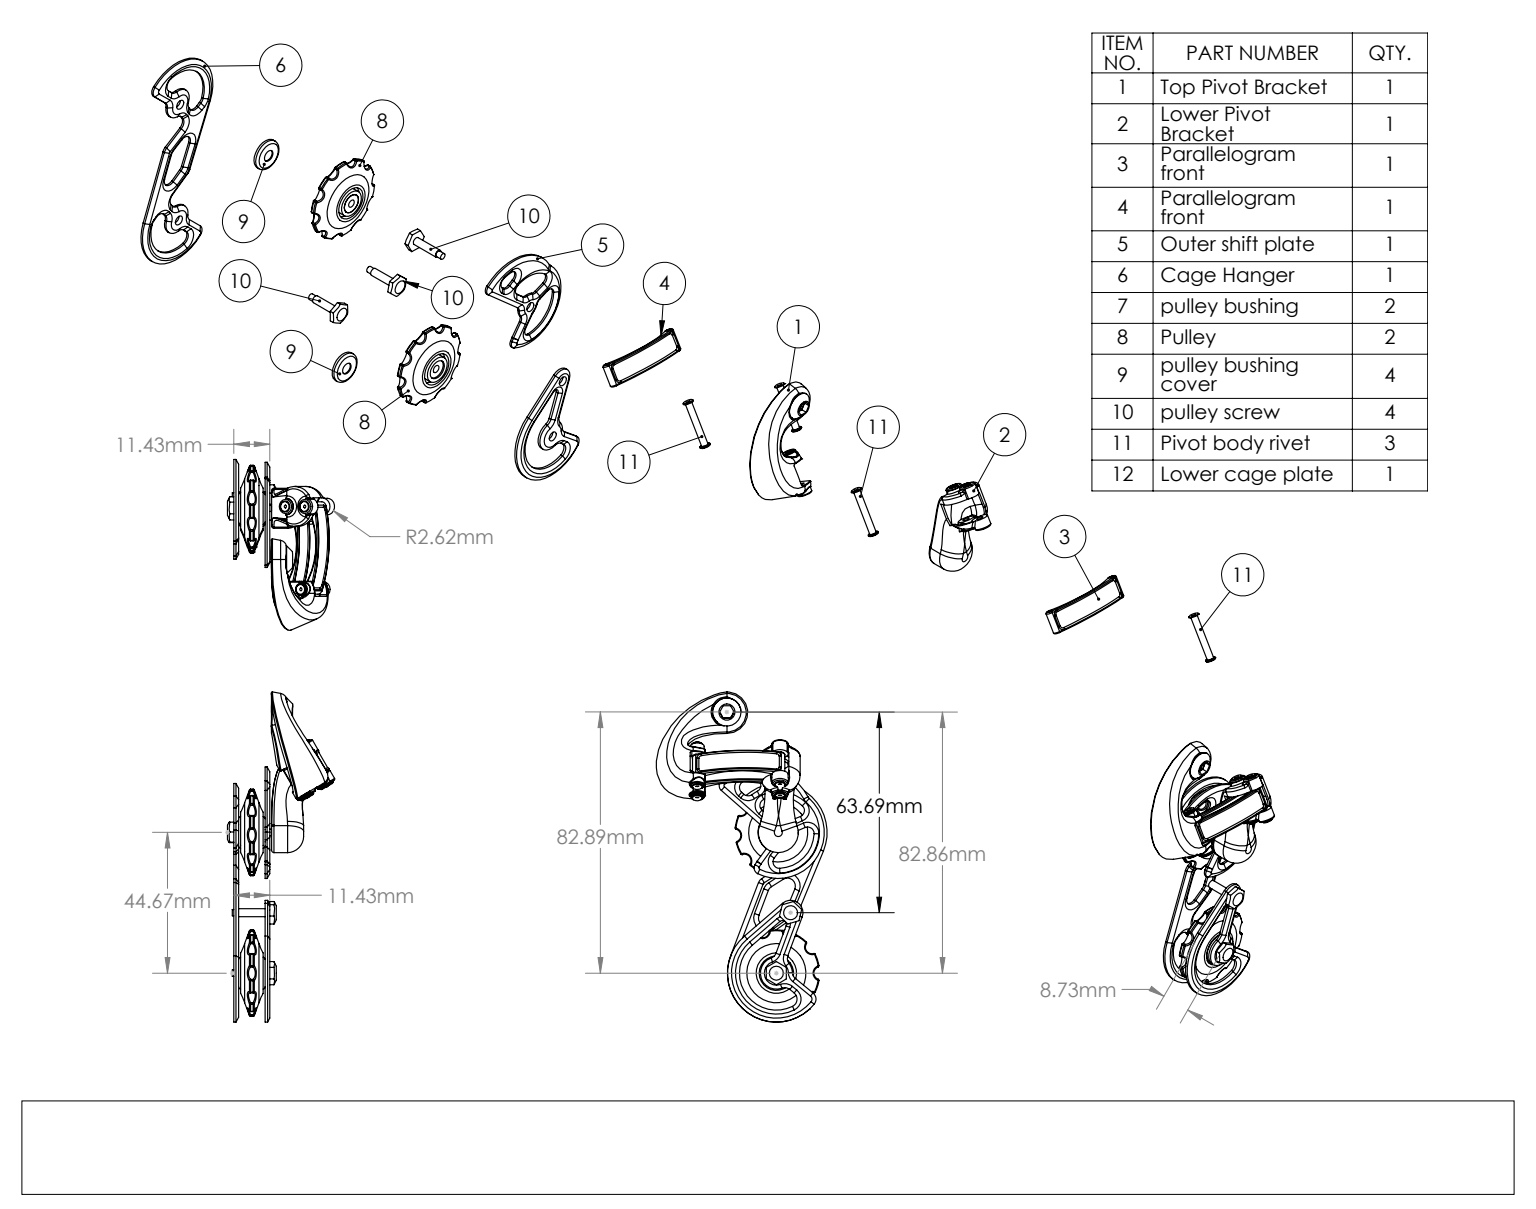
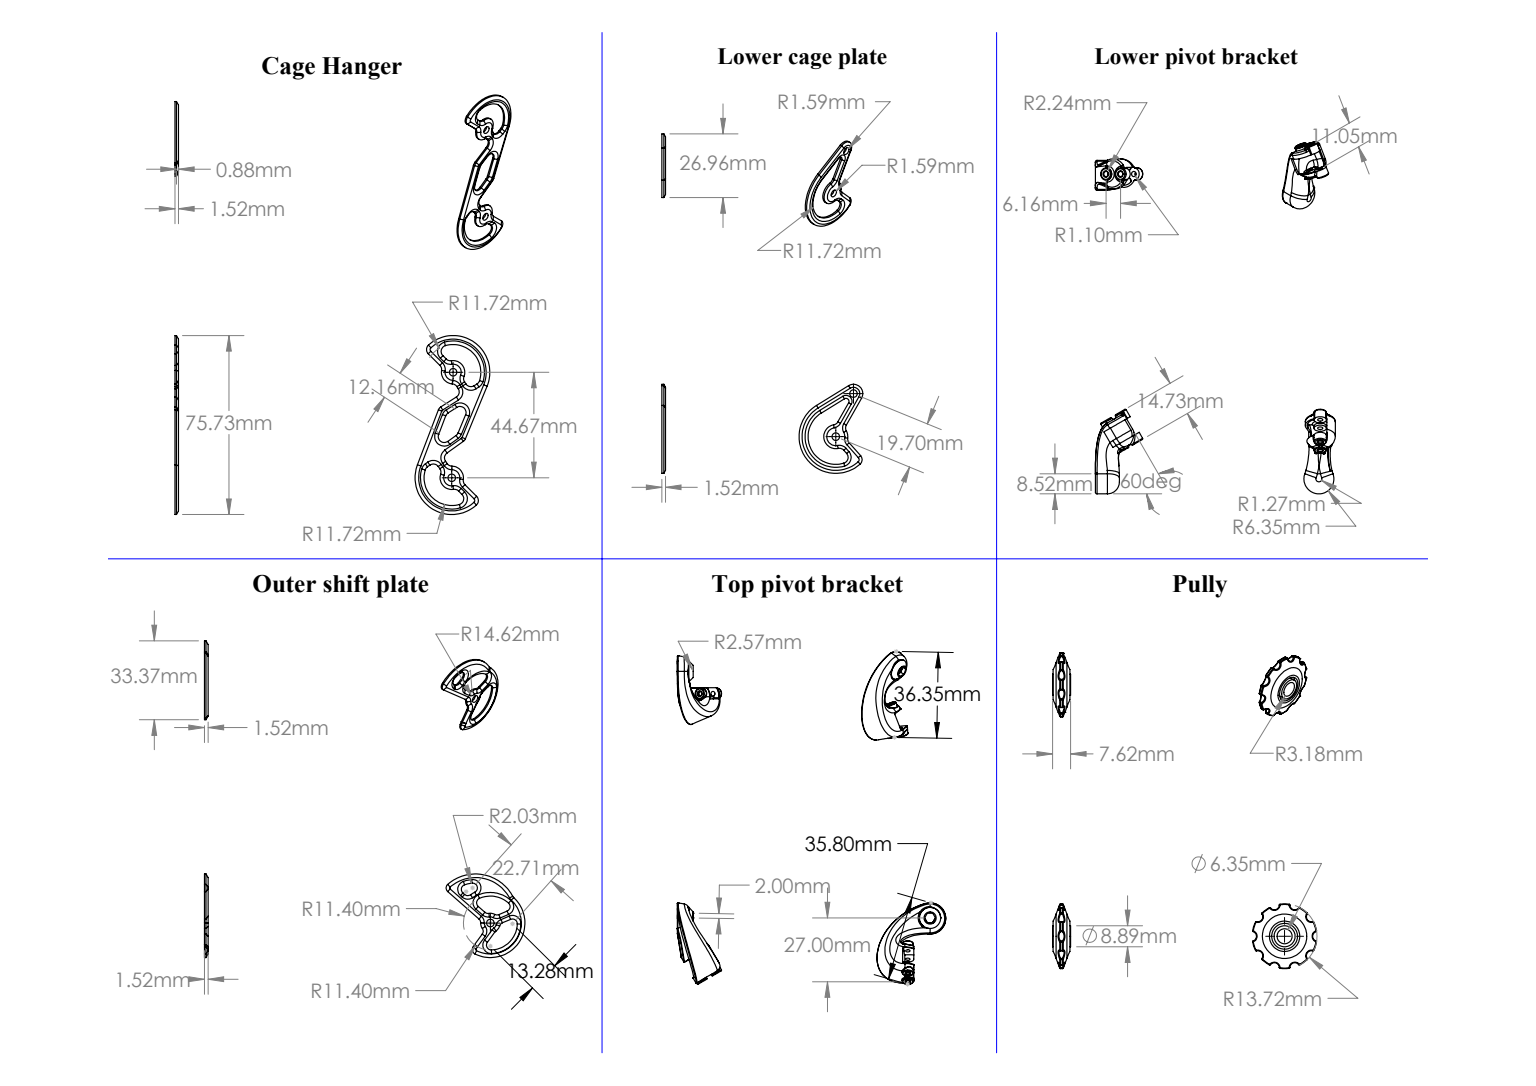
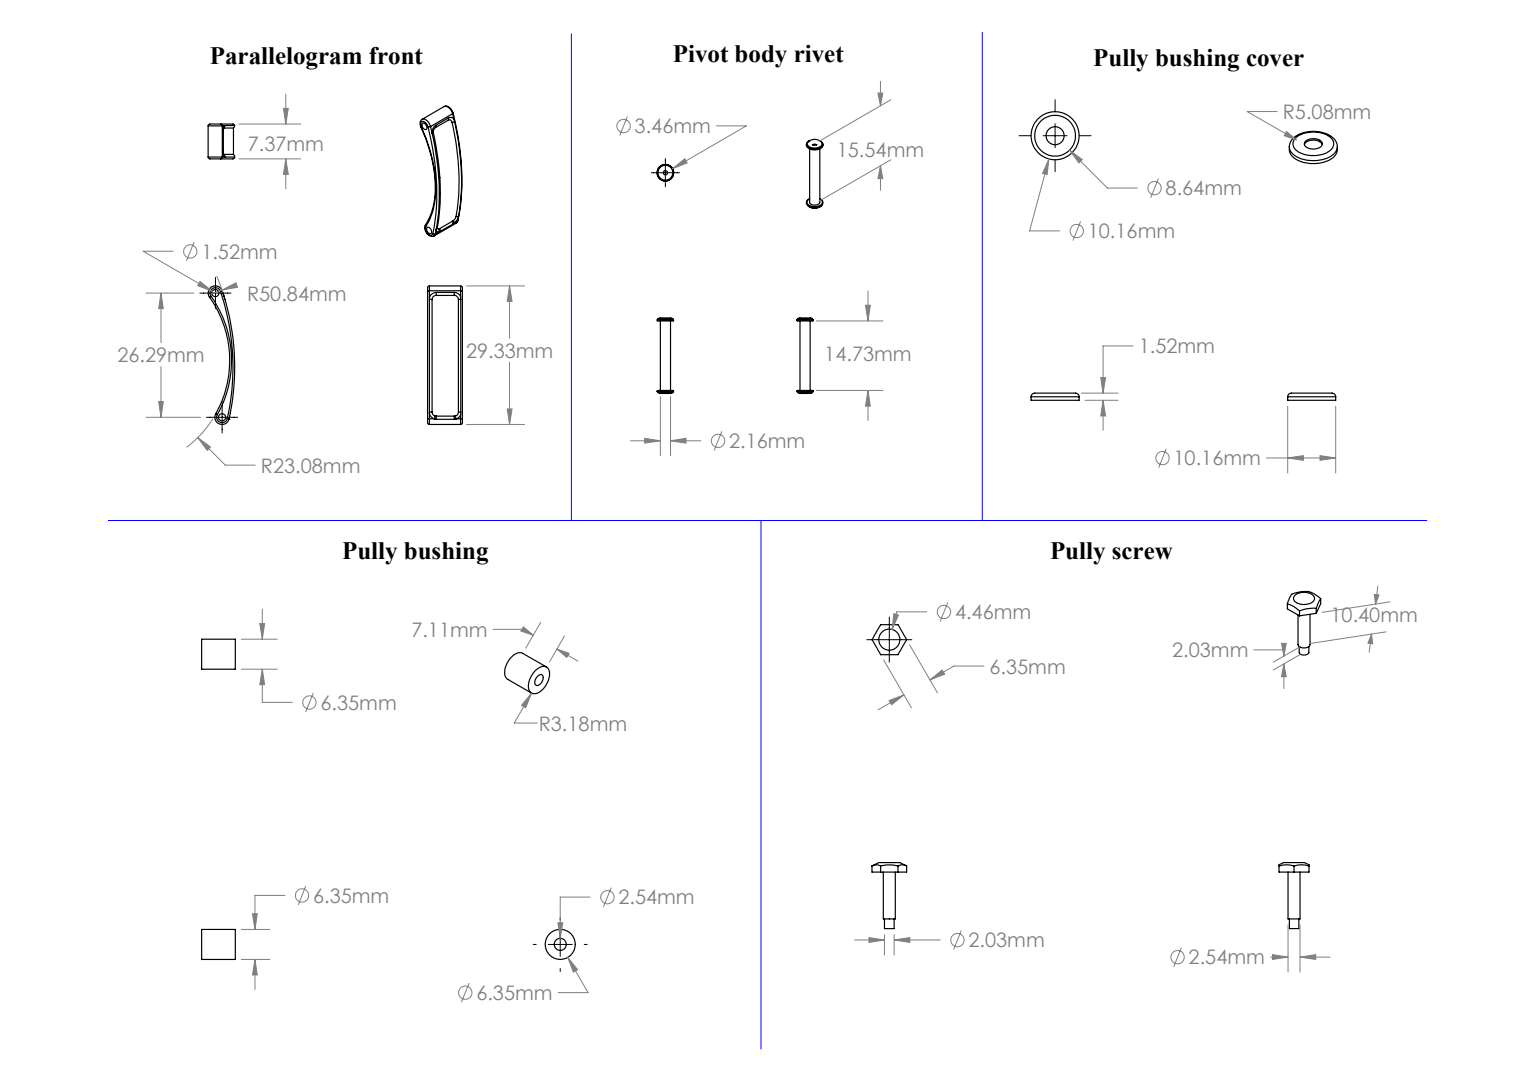
ISO-10303-21;
HEADER;
FILE_DESCRIPTION (('STEP AP214'),
    '1' );
FILE_NAME ('MAT-032',
    '2026-10-12T23:53:07',
    ( '' ),
    ( '' ),
    'SwSTEP 2.0',
    'SolidWorks 2024',
    '' );
FILE_SCHEMA (( 'AUTOMOTIVE_DESIGN' ));
ENDSEC;

DATA;
#1 = CARTESIAN_POINT ( 'NONE',  ( 0.4999436808859595294, -1.292550018364103881, 0.6106580130240608639 ) ) ;
#3 = EDGE_LOOP ( 'NONE', ( #27545, #19145, #8078, #4181 ) ) ;
#2 = CARTESIAN_POINT ( 'NONE',  ( 0.6766858697071348461, -1.447219178500369852, 0.5182417262812423209 ) ) ;
#4 = CARTESIAN_POINT ( 'NONE',  ( 0.4897881687547872565, -1.080982661159355818, 0.5914788577480112330 ) ) ;
#5 = EDGE_LOOP ( 'NONE', ( #28695, #28375, #39300, #8290 ) ) ;
#6 = PERSON_AND_ORGANIZATION ( #28500, #32463 ) ;
#7 = CARTESIAN_POINT ( 'NONE',  ( 0.01548846960707511190, -0.5198120922912051745, -0.07362328916749329155 ) ) ;
#8 = EDGE_LOOP ( 'NONE', ( #25751, #37385, #3783, #18392 ) ) ;
#9 = ORIENTED_EDGE ( 'NONE', *, *, #10978, .F. ) ;
#10 = CARTESIAN_POINT ( 'NONE',  ( 0.3847673884423530866, -1.587979917868051594, 0.7195363636215315051 ) ) ;
#12 = CARTESIAN_POINT ( 'NONE',  ( 0.1868532161955482884, -0.6181774020623623800, -0.006882278619014759076 ) ) ;
#11 = CARTESIAN_POINT ( 'NONE',  ( 0.06449619071327084008, -0.8352737646558907603, 0.1359541117914142838 ) ) ;
#13 = CARTESIAN_POINT ( 'NONE',  ( 0.06860968454252140691, -0.5593946951873564055, 0.07183308462254860138 ) ) ;
#14 = VERTEX_POINT ( 'NONE', #12483 ) ;
#15 = ORIENTED_EDGE ( 'NONE', *, *, #31298, .F. ) ;
#16 = CARTESIAN_POINT ( 'NONE',  ( 0.4409725506264777772, -1.045015864252073712, 0.6370139139982947674 ) ) ;
#17 = CARTESIAN_POINT ( 'NONE',  ( 0.1277648457822606887, -0.6229659815690001823, 0.3707106540332985034 ) ) ;
#18 = ORIENTED_EDGE ( 'NONE', *, *, #35646, .F. ) ;
#19 = CARTESIAN_POINT ( 'NONE',  ( 0.2420619479266831187, -1.321943518198432033, -0.3144976166544464768 ) ) ;
#20 = CARTESIAN_POINT ( 'NONE',  ( 0.6117213743483401744, -1.432107776390856513, -0.6250000000000000000 ) ) ;
#21 = CYLINDRICAL_SURFACE ( 'NONE', #16555, 0.1000000000000000056 ) ;
#22 = ADVANCED_FACE ( 'NONE', ( #25039 ), #12689, .F. ) ;
#23 = CARTESIAN_POINT ( 'NONE',  ( 0.5982604594170003454, -1.483634568127149889, -0.3944719512476840273 ) ) ;
#24 = ADVANCED_FACE ( 'NONE', ( #40477 ), #35210, .T. ) ;
#25 = CARTESIAN_POINT ( 'NONE',  ( 0.3439459955960700865, -1.757593179262507466, 0.4441638180110000222 ) ) ;
#26 = DIRECTION ( 'NONE',  ( 0.000000000000000000, 0.000000000000000000, 1.000000000000000000 ) ) ;
#27 = CARTESIAN_POINT ( 'NONE',  ( 0.1178002186443738025, -1.269485432265525793, 0.6202127893679206805 ) ) ;
#28 = CARTESIAN_POINT ( 'NONE',  ( 0.2462190030042624156, -1.768833963249898611, -0.6590625227467041825 ) ) ;
#29 = CARTESIAN_POINT ( 'NONE',  ( -0.01548846960707524721, 0.000000000000000000, 0.000000000000000000 ) ) ;
#30 = APPROVAL_STATUS ( 'not_yet_approved' ) ;
#31 = CARTESIAN_POINT ( 'NONE',  ( 0.1947294528115406376, -0.9190940877486376559, 0.2754987677893815934 ) ) ;
#32 = PLANE ( 'NONE',  #30520 ) ;
#33 = CARTESIAN_POINT ( 'NONE',  ( 0.4569214742076340707, -1.218928684383336236, 0.5856983068965044836 ) ) ;
#34 = CARTESIAN_POINT ( 'NONE',  ( 0.3193861777821562220, -1.171684894966655399, 0.5563056129421823925 ) ) ;
#35 = CARTESIAN_POINT ( 'NONE',  ( 0.1851448419613674068, -1.516587896426844662, 0.7176110508928341680 ) ) ;
#36 = LINE ( 'NONE', #30842, #35705 ) ;
#37 = DIRECTION ( 'NONE',  ( -6.162975822039154730E-33, 0.000000000000000000, -1.000000000000000000 ) ) ;
#38 = CARTESIAN_POINT ( 'NONE',  ( 0.5966652623928320187, -1.460067201996130271, 0.6057417262805135927 ) ) ;
#39 = EDGE_CURVE ( 'NONE', #17084, #9403, #40506, .T. ) ;
#40 = ORIENTED_EDGE ( 'NONE', *, *, #699, .T. ) ;
#41 = ORIENTED_EDGE ( 'NONE', *, *, #38593, .T. ) ;
#42 = CARTESIAN_POINT ( 'NONE',  ( -0.1105199412301896417, -0.5049077968913929793, 0.1209919789212513253 ) ) ;
#43 = ORIENTED_EDGE ( 'NONE', *, *, #31016, .F. ) ;
#44 = CARTESIAN_POINT ( 'NONE',  ( 0.2625221014770238726, -1.677489247281143347, 0.5299707248247536029 ) ) ;
#45 = CARTESIAN_POINT ( 'NONE',  ( -0.03650581953630592513, -0.4542932396444835375, -0.2355374485430490328 ) ) ;
#46 = CARTESIAN_POINT ( 'NONE',  ( 0.5765142360455419723, -1.424711725393718265, 0.6097170742772620722 ) ) ;
#48 = ORIENTED_EDGE ( 'NONE', *, *, #29288, .T. ) ;
#47 = CARTESIAN_POINT ( 'NONE',  ( 0.001926542279114920901, -0.5275834520082917090, 0.09413269016402606160 ) ) ;
#49 = EDGE_LOOP ( 'NONE', ( #33530, #28150, #39778, #7630 ) ) ;
#50 = FACE_OUTER_BOUND ( 'NONE', #29896, .T. ) ;
#51 = VERTEX_POINT ( 'NONE', #15776 ) ;
#52 = CARTESIAN_POINT ( 'NONE',  ( 0.2972168835034767476, -1.656689438746897558, 0.5739732049407664238 ) ) ;
#54 = CARTESIAN_POINT ( 'NONE',  ( 0.08190433410803919789, -1.308169647316527184, 0.5665045013630258808 ) ) ;
#53 = CARTESIAN_POINT ( 'NONE',  ( 0.5200734380266420764, -1.679028703643771436, -0.4374651140121203485 ) ) ;
#55 = LINE ( 'NONE', #28391, #16768 ) ;
#56 = CALENDAR_DATE ( 2026, 13, 10 ) ;
#58 = ORIENTED_EDGE ( 'NONE', *, *, #32260, .T. ) ;
#57 = EDGE_LOOP ( 'NONE', ( #4186, #2029, #37849, #1328 ) ) ;
#59 = FACE_OUTER_BOUND ( 'NONE', #105, .T. ) ;
#60 = DIRECTION ( 'NONE',  ( 0.8660512985181130219, 0.4999551463232377868, 0.000000000000000000 ) ) ;
#61 = PERSON ( 'NAUO-PER8', 'UNSPECIFIED', 'UNSPECIFIED', ('UNSPECIFIED'), ('UNSPECIFIED'), ('UNSPECIFIED') ) ;
#62 = DIRECTION ( 'NONE',  ( 0.3468893892380631727, 0.9373665302208734618, -0.03180785525186744650 ) ) ;
#63 = CARTESIAN_POINT ( 'NONE',  ( 0.2884976522880303706, -0.9761975876302364519, 0.7460397395601686688 ) ) ;
#64 = CARTESIAN_POINT ( 'NONE',  ( 0.1828007326059407633, -0.8784064217732538982, 0.5457344770029756154 ) ) ;
#65 = CARTESIAN_POINT ( 'NONE',  ( 0.2745644270868899950, -1.657411742223986018, 0.7254928767627549790 ) ) ;
#66 = ADVANCED_FACE ( 'NONE', ( #33910 ), #4970, .T. ) ;
#67 = CARTESIAN_POINT ( 'NONE',  ( 0.3207235327959215287, -1.760688231293898953, 0.5959548780354907427 ) ) ;
#68 = FACE_OUTER_BOUND ( 'NONE', #7963, .T. ) ;
#69 = FACE_OUTER_BOUND ( 'NONE', #19030, .T. ) ;
#70 = CARTESIAN_POINT ( 'NONE',  ( 0.4763501221259694440, -1.554011115824661893, -0.5166151207188711680 ) ) ;
#71 = DIRECTION ( 'NONE',  ( 2.465190328815661892E-32, 1.000000000000000000, -5.978086547377980964E-31 ) ) ;
#72 = DIRECTION ( 'NONE',  ( -0.9999999999999998890, -5.551115123125780853E-17, -5.551115123125781470E-17 ) ) ;
#73 = AXIS2_PLACEMENT_3D ( 'NONE', #22419, #1050, #19125 ) ;
#74 = PLANE ( 'NONE',  #31747 ) ;
#75 = CARTESIAN_POINT ( 'NONE',  ( 0.07120675875603865723, -0.8149881486554784171, 0.8228864848196146831 ) ) ;
#76 = CARTESIAN_POINT ( 'NONE',  ( 0.09717445250287677638, -1.337075187059802994, 0.7110840001749388906 ) ) ;
#77 = APPLICATION_PROTOCOL_DEFINITION ( 'international standard', 'automotive_design', 2000, #10342 ) ;
#78 = CARTESIAN_POINT ( 'NONE',  ( 0.3560095073596968307, -0.8726986411092064744, 0.7484988241699506162 ) ) ;
#79 = AXIS2_PLACEMENT_3D ( 'NONE', #37935, #9745, #19216 ) ;
#80 = CARTESIAN_POINT ( 'NONE',  ( -0.04157143636675594833, 0.4416880288200871196, 0.1614235308635322275 ) ) ;
#81 = CARTESIAN_POINT ( 'NONE',  ( 0.6872956252228072938, -1.545186843986040115, 0.5945327379366810439 ) ) ;
#82 = CARTESIAN_POINT ( 'NONE',  ( 0.4855256156385516775, -1.649569844525025530, -0.6308821889615696676 ) ) ;
#83 = PLANE ( 'NONE',  #29685 ) ;
#84 = ORIENTED_EDGE ( 'NONE', *, *, #28072, .F. ) ;
#85 = FACE_OUTER_BOUND ( 'NONE', #18714, .T. ) ;
#86 = CARTESIAN_POINT ( 'NONE',  ( 0.1825910822803085698, -1.345967781949698239, 0.9412546887375772275 ) ) ;
#87 = CARTESIAN_POINT ( 'NONE',  ( 0.5953442517954894431, -1.487188481951640773, 0.5814371352277787341 ) ) ;
#89 = ORIENTED_EDGE ( 'NONE', *, *, #20270, .F. ) ;
#88 = DIRECTION ( 'NONE',  ( 1.000000000000000000, 0.000000000000000000, 0.000000000000000000 ) ) ;
#90 = CARTESIAN_POINT ( 'NONE',  ( 0.1967848402874973202, -0.7048484731626001309, 0.3032743993732655574 ) ) ;
#92 = ORIENTED_EDGE ( 'NONE', *, *, #28854, .F. ) ;
#91 = ORIENTED_EDGE ( 'NONE', *, *, #5942, .F. ) ;
#93 = DIRECTION ( 'NONE',  ( 0.000000000000000000, 0.9510565162951657436, 0.3090169943749095927 ) ) ;
#94 = CARTESIAN_POINT ( 'NONE',  ( 0.3337487181682026183, -1.684227851221292038, -0.6212492361075898639 ) ) ;
#95 = LINE ( 'NONE', #12201, #34463 ) ;
#96 = PERSON_AND_ORGANIZATION_ROLE ( 'classification_officer' ) ;
#97 = CIRCLE ( 'NONE', #11204, 0.5399999999999999245 ) ;
#98 = ORIENTED_EDGE ( 'NONE', *, *, #22101, .F. ) ;
#99 = CARTESIAN_POINT ( 'NONE',  ( 0.09103128088014370012, -0.7737444593052549280, 0.2676987870228014210 ) ) ;
#100 = CARTESIAN_POINT ( 'NONE',  ( 0.3114310930860528792, -1.743835956959021161, 0.7216218591552465700 ) ) ;
#101 = AXIS2_PLACEMENT_3D ( 'NONE', #14971, #21565, #27524 ) ;
#102 = CARTESIAN_POINT ( 'NONE',  ( 0.5255678041659990196, -1.526919996939806623, 0.5791403307438186543 ) ) ;
#103 = CARTESIAN_POINT ( 'NONE',  ( -0.08000000000000000167, -2.183180860297908144, -0.4937760292030871079 ) ) ;
#104 = CARTESIAN_POINT ( 'NONE',  ( -0.1710642717957937542, 0.4986889573705819423, 0.1482573527501182542 ) ) ;
#105 = EDGE_LOOP ( 'NONE', ( #14125, #9497, #24205 ) ) ;
#106 = VECTOR ( 'NONE', #18794, 39.37007874015748143 ) ;
#107 = CARTESIAN_POINT ( 'NONE',  ( -0.01736481776669303659, -0.6872203660140440151, -0.01676916986599873496 ) ) ;
#108 = CARTESIAN_POINT ( 'NONE',  ( 0.6985683150901143001, -1.438855895731389056, 0.5688516854839209547 ) ) ;
#109 = CARTESIAN_POINT ( 'NONE',  ( 0.5745725605903601041, -1.619018034204693146, 0.5636810530413540743 ) ) ;
#110 = CARTESIAN_POINT ( 'NONE',  ( -0.002236529766539807878, -0.8463514994925549484, 0.1275420592413386567 ) ) ;
#111 = CYLINDRICAL_SURFACE ( 'NONE', #1726, 0.7043128707267513056 ) ;
#112 = CARTESIAN_POINT ( 'NONE',  ( 0.4203826191881492313, -1.700944664958275343, -0.4172566670736511107 ) ) ;
#113 = CARTESIAN_POINT ( 'NONE',  ( 0.01632176102313256591, -1.052923364454138255, 0.5995154855756178458 ) ) ;
#114 = CARTESIAN_POINT ( 'NONE',  ( 0.5138184642618360831, -1.118801421376873551, 0.5693865086028936373 ) ) ;
#115 = DATE_AND_TIME ( #15705, #6911 ) ;
#116 = CARTESIAN_POINT ( 'NONE',  ( 0.3610818047233222972, -1.951413994126270257, -0.4993772958782550786 ) ) ;
#117 = AXIS2_PLACEMENT_3D ( 'NONE', #32026, #16389, #31621 ) ;
#118 = CARTESIAN_POINT ( 'NONE',  ( 0.6078054091579164764, -1.478899637288701996, 0.5472081702953829341 ) ) ;
#119 = VECTOR ( 'NONE', #8950, 39.37007874015748143 ) ;
#120 = CARTESIAN_POINT ( 'NONE',  ( -0.04762200653274516887, 0.04294689284307845467, 0.4802757286815055315 ) ) ;
#121 = ORIENTED_EDGE ( 'NONE', *, *, #38880, .F. ) ;
#122 = CARTESIAN_POINT ( 'NONE',  ( -0.1212602504878775439, -0.5073146173917505442, 0.3032895567580813356 ) ) ;
#123 = CIRCLE ( 'NONE', #23102, 0.02999999999999997113 ) ;
#124 = DIRECTION ( 'NONE',  ( -1.000000000000000000, -2.341930812374887555E-31, 1.664003471950578127E-31 ) ) ;
#125 = CIRCLE ( 'NONE', #26384, 0.1000000000000000194 ) ;
#126 = CARTESIAN_POINT ( 'NONE',  ( 0.08704502409080258629, -0.7188400997375623547, 0.02651060292151286024 ) ) ;
#127 = ORIENTED_EDGE ( 'NONE', *, *, #21048, .F. ) ;
#128 = EDGE_CURVE ( 'NONE', #3309, #37479, #16156, .T. ) ;
#129 = ADVANCED_FACE ( 'NONE', ( #22978 ), #24068, .T. ) ;
#130 = CARTESIAN_POINT ( 'NONE',  ( -0.004104496411111036719, -0.9055868175180781243, 0.5348166647311645150 ) ) ;
#132 = ORIENTED_EDGE ( 'NONE', *, *, #28235, .F. ) ;
#131 = ORIENTED_EDGE ( 'NONE', *, *, #7728, .F. ) ;
#133 = ADVANCED_FACE ( 'NONE', ( #4027 ), #10817, .T. ) ;
#134 = DIRECTION ( 'NONE',  ( -1.000000000000000000, 0.000000000000000000, 0.000000000000000000 ) ) ;
#135 = ORIENTED_EDGE ( 'NONE', *, *, #17010, .F. ) ;
#136 = DIRECTION ( 'NONE',  ( 1.000000000000000000, 2.276539994720204558E-15, -1.138269997360102279E-15 ) ) ;
#137 = CARTESIAN_POINT ( 'NONE',  ( 0.3648774902654713936, -1.763897834913869644, -0.5277763367469582301 ) ) ;
#138 = EDGE_CURVE ( 'NONE', #15118, #39770, #26750, .T. ) ;
#140 = DIRECTION ( 'NONE',  ( -0.9823715787225880680, 0.000000000000000000, -0.1869387100578417116 ) ) ;
#139 = CARTESIAN_POINT ( 'NONE',  ( 0.05491348488830435220, 0.4316112672892343238, 0.1667783590291176121 ) ) ;
#141 = CARTESIAN_POINT ( 'NONE',  ( 0.04762035657658141713, -0.2475516194925235502, -0.4138014489398372242 ) ) ;
#142 = ORIENTED_EDGE ( 'NONE', *, *, #5731, .F. ) ;
#143 = EDGE_CURVE ( 'NONE', #32215, #37335, #22584, .T. ) ;
#144 = CARTESIAN_POINT ( 'NONE',  ( 0.1448932857592245271, -0.7256843399750660950, 0.5340175887863652937 ) ) ;
#145 = EDGE_LOOP ( 'NONE', ( #25548, #19484 ) ) ;
#146 = DIRECTION ( 'NONE',  ( 0.000000000000000000, 0.000000000000000000, 1.000000000000000000 ) ) ;
#147 = CARTESIAN_POINT ( 'NONE',  ( 0.4408799025385287673, -1.573480893639235711, 0.5609592079540931531 ) ) ;
#149 = CARTESIAN_POINT ( 'NONE',  ( 0.5621007238609228018, -1.618750287028627222, 0.5241914645917098436 ) ) ;
#148 = CARTESIAN_POINT ( 'NONE',  ( 0.5164807395112145372, -1.614047142484251740, -0.4728386827019681049 ) ) ;
#150 = CYLINDRICAL_SURFACE ( 'NONE', #28383, 0.1249999999999999584 ) ;
#151 = CARTESIAN_POINT ( 'NONE',  ( 0.1406250000000003053, -0.9233928627580062498, 0.1457185332388702126 ) ) ;
#152 = VECTOR ( 'NONE', #11344, 39.37007874015748854 ) ;
#153 = CARTESIAN_POINT ( 'NONE',  ( 0.2614565024141663474, -0.7584087153545726601, 0.1023043458361302949 ) ) ;
#154 = CARTESIAN_POINT ( 'NONE',  ( 0.2153966442130109959, -1.622051466259873287, -0.3272083645034317145 ) ) ;
#155 = CARTESIAN_POINT ( 'NONE',  ( 0.5811800998074035940, -1.495285155999573012, 0.5781461679035739820 ) ) ;
#156 = CARTESIAN_POINT ( 'NONE',  ( -0.04574984450155351878, 0.3363984555176486313, -0.3523422282978309616 ) ) ;
#157 = VECTOR ( 'NONE', #34614, 39.37007874015748143 ) ;
#158 =( BOUNDED_SURFACE ( )  B_SPLINE_SURFACE ( 3, 2, ( 
 ( #37955, #25824, #4400 ),
 ( #1341, #3597, #16958 ),
 ( #29091, #25426, #31783 ),
 ( #29309, #38557, #10179 ),
 ( #16166, #7070, #22943 ),
 ( #35460, #3797, #13468 ),
 ( #22335, #22748, #16353 ),
 ( #28703, #19641, #16549 ),
 ( #567, #9766, #13063 ),
 ( #749, #35275, #26035 ),
 ( #23144, #13657, #1157 ),
 ( #25614, #32175, #3986 ),
 ( #9969, #38145, #28888 ),
 ( #35066, #26222, #4194 ),
 ( #6872, #19447, #10570 ),
 ( #35672, #7261, #19835 ),
 ( #31985, #32369, #7475 ),
 ( #16761, #20052, #32585 ),
 ( #8302, #7875, #1760 ),
 ( #23745, #5201, #39365 ),
 ( #10788, #32982, #35881 ),
 ( #33586, #30307, #14068 ),
 ( #30113, #14672, #23360 ),
 ( #7693, #30518, #11184 ),
 ( #21059, #4581, #20448 ),
 ( #39175, #20873, #26422 ),
 ( #5396, #17958, #13849 ),
 ( #38958, #20258, #17571 ),
 ( #32780, #14272, #17754 ),
 ( #36267, #17153, #29702 ),
 ( #27027, #1547, #39554 ),
 ( #4788, #26644, #2134 ),
 ( #33394, #17363, #11000 ),
 ( #23558, #23959, #20665 ),
 ( #36076, #26836, #29918 ),
 ( #8088, #33199, #27242 ),
 ( #11387, #5004, #1944 ),
 ( #39773, #14459, #36488 ),
 ( #11603, #24165, #36689 ),
 ( #8495, #40164, #36882 ),
 ( #5611, #8690, #39969 ),
 ( #18367, #37696, #18167 ),
 ( #12206, #18792, #21268 ),
 ( #33805, #40579, #11994 ),
 ( #100, #31343, #6225 ),
 ( #27841, #30721, #24953 ),
 ( #37289, #15080, #31131 ),
 ( #9103, #30913, #3148 ) ),
 .UNSPECIFIED., .F., .F., .T. ) 
 B_SPLINE_SURFACE_WITH_KNOTS ( ( 4, 2, 2, 2, 2, 2, 2, 2, 2, 2, 2, 2, 2, 2, 2, 2, 2, 2, 2, 2, 2, 2, 2, 4 ),
 ( 3, 3 ),
 ( 0.009784760482578789414, 0.01303178080197338849, 0.01465529096167068890, 0.01627880112136798757, 0.01952582144076258491, 0.02114933160045988358, 0.02277284176015718226, 0.02926688239894638041, 0.03251390271834098122, 0.03576092303773557857, 0.03900794335713017591, 0.04225496367652477325, 0.04387847383622207192, 0.04550198399591937060, 0.04712549415561667621, 0.04874900431531397488, 0.05037251447501127355, 0.05199602463470857916, 0.05361953479440587783, 0.05443128987425452370, 0.05524304495410317650, 0.05686655511380047517, 0.05849006527349777385, 0.06173708559289237119 ),
 ( 0.000000000000000000, 1.000000000000000000 ),
 .UNSPECIFIED. ) 
 GEOMETRIC_REPRESENTATION_ITEM ( )  RATIONAL_B_SPLINE_SURFACE ( (
 ( 1.000000000000000000, 0.6287678658096880202, 1.000000000000000000),
 ( 1.000000000000000000, 0.6288662671286704420, 1.000000000000000000),
 ( 1.000000000000000000, 0.6274741409696639183, 1.000000000000000000),
 ( 1.000000000000000000, 0.6287776757897947100, 1.000000000000000000),
 ( 1.000000000000000000, 0.6296837007773170569, 1.000000000000000000),
 ( 1.000000000000000000, 0.6313229865883394076, 1.000000000000000000),
 ( 1.000000000000000000, 0.6321460476172471310, 1.000000000000000000),
 ( 1.000000000000000000, 0.6347778756843863723, 1.000000000000000000),
 ( 1.000000000000000000, 0.6367158758108866223, 1.000000000000000000),
 ( 1.000000000000000000, 0.6398588341727308171, 1.000000000000000000),
 ( 1.000000000000000000, 0.6409477486316274009, 1.000000000000000000),
 ( 1.000000000000000000, 0.6432257032707729971, 1.000000000000000000),
 ( 1.000000000000000000, 0.6444106978184096501, 1.000000000000000000),
 ( 1.000000000000000000, 0.6505171573845394128, 1.000000000000000000),
 ( 1.000000000000000000, 0.6559831852215063375, 1.000000000000000000),
 ( 1.000000000000000000, 0.6631771220578878134, 1.000000000000000000),
 ( 1.000000000000000000, 0.6653492434363603714, 1.000000000000000000),
 ( 1.000000000000000000, 0.6687561138349609191, 1.000000000000000000),
 ( 1.000000000000000000, 0.6700066037122677232, 1.000000000000000000),
 ( 1.000000000000000000, 0.6713450054086019803, 1.000000000000000000),
 ( 1.000000000000000000, 0.6714450553368720431, 1.000000000000000000),
 ( 1.000000000000000000, 0.6706951819970428108, 1.000000000000000000),
 ( 1.000000000000000000, 0.6697953818427609951, 1.000000000000000000),
 ( 1.000000000000000000, 0.6680617541732161158, 1.000000000000000000),
 ( 1.000000000000000000, 0.6674309137187000029, 1.000000000000000000),
 ( 1.000000000000000000, 0.6661647704555568872, 1.000000000000000000),
 ( 1.000000000000000000, 0.6655247572274053391, 1.000000000000000000),
 ( 1.000000000000000000, 0.6643577078737322728, 1.000000000000000000),
 ( 1.000000000000000000, 0.6638299590325124067, 1.000000000000000000),
 ( 1.000000000000000000, 0.6631078123530266266, 1.000000000000000000),
 ( 1.000000000000000000, 0.6629281639512619728, 1.000000000000000000),
 ( 1.000000000000000000, 0.6631493259863866507, 1.000000000000000000),
 ( 1.000000000000000000, 0.6635445073558746687, 1.000000000000000000),
 ( 1.000000000000000000, 0.6652273697468563673, 1.000000000000000000),
 ( 1.000000000000000000, 0.6664745574001266215, 1.000000000000000000),
 ( 1.000000000000000000, 0.6697857743441212319, 1.000000000000000000),
 ( 1.000000000000000000, 0.6718404721287462023, 1.000000000000000000),
 ( 1.000000000000000000, 0.6753207313297656667, 1.000000000000000000),
 ( 1.000000000000000000, 0.6765490974884642572, 1.000000000000000000),
 ( 1.000000000000000000, 0.6790248312221631721, 1.000000000000000000),
 ( 1.000000000000000000, 0.6802787004308656904, 1.000000000000000000),
 ( 1.000000000000000000, 0.6840080678706492723, 1.000000000000000000),
 ( 1.000000000000000000, 0.6864616782751722379, 1.000000000000000000),
 ( 1.000000000000000000, 0.6908458362598728364, 1.000000000000000000),
 ( 1.000000000000000000, 0.6927390833103468371, 1.000000000000000000),
 ( 1.000000000000000000, 0.6973153832233414118, 1.000000000000000000),
 ( 1.000000000000000000, 0.6988858220003437705, 1.000000000000000000),
 ( 1.000000000000000000, 0.6986036234954329238, 1.000000000000000000) ) ) 
 REPRESENTATION_ITEM ( '' )  SURFACE ( )  );
#159 = AXIS2_PLACEMENT_3D ( 'NONE', #8390, #5286, #20960 ) ;
#160 = EDGE_CURVE ( 'NONE', #40387, #17181, #6292, .T. ) ;
#161 = DIRECTION ( 'NONE',  ( -1.000000000000000000, -0.000000000000000000, -0.000000000000000000 ) ) ;
#162 = APPLIED_PERSON_AND_ORGANIZATION_ASSIGNMENT ( #34122, #22406, ( #37836 ) ) ;
#163 = DIRECTION ( 'NONE',  ( -1.000000000000000000, -0.000000000000000000, -0.000000000000000000 ) ) ;
#164 = VECTOR ( 'NONE', #40560, 39.37007874015748143 ) ;
#165 = CARTESIAN_POINT ( 'NONE',  ( 0.3175065632424611817, -1.048436534473135895, 0.7840659024250604681 ) ) ;
#166 = DIRECTION ( 'NONE',  ( -1.000000000000000000, -2.280301054154495132E-31, 1.664003471950577689E-31 ) ) ;
#167 = CARTESIAN_POINT ( 'NONE',  ( 0.5193158764790237747, -1.143105642405225053, 0.8514134314631569556 ) ) ;
#168 = CARTESIAN_POINT ( 'NONE',  ( -0.05279185365593578455, 0.2420570131477374765, 0.4010466975930304101 ) ) ;
#169 = CARTESIAN_POINT ( 'NONE',  ( 0.04665094350991502714, -1.166787722506144265, 0.6642627002602656816 ) ) ;
#170 = B_SPLINE_CURVE_WITH_KNOTS ( 'NONE', 3,
 ( #2399, #24613, #27897, #39613, #37341, #14514 ),
 .UNSPECIFIED., .F., .F.,
 ( 4, 2, 4 ),
 ( 0.0002303018524726754336, 0.0008163183685728737319, 0.001402334884673072084 ),
 .UNSPECIFIED. ) ;
#171 = B_SPLINE_CURVE_WITH_KNOTS ( 'NONE', 3,
 ( #36912, #8724, #30944, #15317 ),
 .UNSPECIFIED., .F., .F.,
 ( 4, 4 ),
 ( 4.416736787580399614E-17, 0.0002767382645091641977 ),
 .UNSPECIFIED. ) ;
#173 = TOROIDAL_SURFACE ( 'NONE', #9991, 0.06434668806854092205, 0.005000000000000000104 ) ;
#172 = CARTESIAN_POINT ( 'NONE',  ( 0.5874764043858021756, -1.597120814744488193, -0.4448059412197695184 ) ) ;
#174 = CARTESIAN_POINT ( 'NONE',  ( 0.1876874445810236824, -0.7927434498347614156, 0.2846742484563515863 ) ) ;
#175 = DIRECTION ( 'NONE',  ( 0.000000000000000000, 0.7516797646744243222, -0.6595282642760672553 ) ) ;
#176 = CARTESIAN_POINT ( 'NONE',  ( 0.09624682736800391214, 0.06028806207340059453, 0.08329560493130624965 ) ) ;
#177 = EDGE_CURVE ( 'NONE', #19587, #15800, #10226, .T. ) ;
#178 = CARTESIAN_POINT ( 'NONE',  ( 0.1779133654309061896, -1.234518891347017533, -0.6184399470714002645 ) ) ;
#179 = ORIENTED_EDGE ( 'NONE', *, *, #9391, .T. ) ;
#180 = CARTESIAN_POINT ( 'NONE',  ( 0.03113248654051816583, -0.2276394436010286959, -0.1339480508475833498 ) ) ;
#181 = CARTESIAN_POINT ( 'NONE',  ( 0.4006050890619684002, -1.646293961035435460, -0.3940011403029922699 ) ) ;
#182 = CARTESIAN_POINT ( 'NONE',  ( 0.6604279980842809872, -1.474831068641988763, 0.4182417262808776348 ) ) ;
#183 = CIRCLE ( 'NONE', #23151, 2.001674066779347783 ) ;
#184 = CARTESIAN_POINT ( 'NONE',  ( 0.5203474827567471372, -1.645139592123281203, -0.4526729257047640287 ) ) ;
#185 = CARTESIAN_POINT ( 'NONE',  ( 0.3311937503011831985, -1.162386653964609939, 0.5777461324143994270 ) ) ;
#186 = EDGE_LOOP ( 'NONE', ( #31291, #14570, #23539, #27301 ) ) ;
#187 = ADVANCED_FACE ( 'NONE', ( #3432 ), #37791, .T. ) ;
#188 = DIRECTION ( 'NONE',  ( -0.05576617208936890391, -0.2535907321052876529, -0.9657027879429589401 ) ) ;
#189 = AXIS2_PLACEMENT_3D ( 'NONE', #3943, #19789, #32329 ) ;
#190 = CONICAL_SURFACE ( 'NONE', #23156, 0.4614999999999880864, 1.047197551196599408 ) ;
#191 = CARTESIAN_POINT ( 'NONE',  ( 0.2591027371085388720, -1.332731507978919705, 0.5181001316254452149 ) ) ;
#192 = CARTESIAN_POINT ( 'NONE',  ( -0.02000000000000000042, -2.183180860297908144, -0.4937760292030871079 ) ) ;
#193 = CARTESIAN_POINT ( 'NONE',  ( 0.04047170147977072197, 0.2415774042519071296, -0.4392095914548690416 ) ) ;
#194 = EDGE_CURVE ( 'NONE', #7245, #4305, #16385, .T. ) ;
#195 = CARTESIAN_POINT ( 'NONE',  ( 0.5122077321654537885, -1.314614967837785198, 0.5911197364003766275 ) ) ;
#197 = DIRECTION ( 'NONE',  ( 0.000000000000000000, 0.000000000000000000, 1.000000000000000000 ) ) ;
#196 = CARTESIAN_POINT ( 'NONE',  ( -1.019575837292305831, -0.04310840302198155199, 0.3750000000000002220 ) ) ;
#198 = CARTESIAN_POINT ( 'NONE',  ( 0.1892170003689550017, -0.8723299121346327345, 0.2416867767302488257 ) ) ;
#199 = VERTEX_POINT ( 'NONE', #1000 ) ;
#200 = DATE_TIME_ROLE ( 'creation_date' ) ;
#201 = EDGE_CURVE ( 'NONE', #33071, #36154, #13038, .T. ) ;
#202 = CARTESIAN_POINT ( 'NONE',  ( 0.04650976029988308780, -1.055486831112860902, 0.7228979986002838087 ) ) ;
#203 = ORIENTED_EDGE ( 'NONE', *, *, #10449, .T. ) ;
#204 = CARTESIAN_POINT ( 'NONE',  ( 0.04803016009707758438, -0.5362635619093905071, 0.1457185332388692967 ) ) ;
#206 = CARTESIAN_POINT ( 'NONE',  ( 0.1846550159866843510, -0.8403219816448772583, 0.07989493322373726614 ) ) ;
#205 = DIRECTION ( 'NONE',  ( 1.000000000000000000, -0.000000000000000000, -0.000000000000000000 ) ) ;
#207 = CARTESIAN_POINT ( 'NONE',  ( 0.06829125384024312129, -0.5762991475062954061, 0.04819365463926665594 ) ) ;
#208 = ORIENTED_EDGE ( 'NONE', *, *, #30408, .T. ) ;
#209 = ORIENTED_EDGE ( 'NONE', *, *, #39795, .T. ) ;
#210 = CARTESIAN_POINT ( 'NONE',  ( 0.5379134690603978308, -1.159344755639895030, 0.5916774385555967353 ) ) ;
#211 = CARTESIAN_POINT ( 'NONE',  ( 0.2895267596155666756, -1.012179684896779674, 0.7737674755748008559 ) ) ;
#212 = ORIENTED_EDGE ( 'NONE', *, *, #27885, .F. ) ;
#213 = CARTESIAN_POINT ( 'NONE',  ( 0.1867098991225878413, -0.7409322124881813076, 0.03654140106717494729 ) ) ;
#214 = CARTESIAN_POINT ( 'NONE',  ( 0.4697623592636160361, -1.061459377010899541, -0.6056023639864149821 ) ) ;
#215 = CARTESIAN_POINT ( 'NONE',  ( 0.01548846960707511190, 0.09061086148575973886, 0.5171215251571029681 ) ) ;
#216 = EDGE_CURVE ( 'NONE', #890, #37816, #37994, .T. ) ;
#217 = CARTESIAN_POINT ( 'NONE',  ( 0.6518945859131652920, -1.452672594389344596, -0.6204649030305892099 ) ) ;
#218 = CARTESIAN_POINT ( 'NONE',  ( 0.05999999999999990757, 0.4357424459509064985, 0.2678820090948821342 ) ) ;
#219 = CIRCLE ( 'NONE', #2141, 0.04330708661417340122 ) ;
#220 = CARTESIAN_POINT ( 'NONE',  ( -0.1172401355130585354, -0.4876450271194930908, 0.3356658914665637816 ) ) ;
#221 = CARTESIAN_POINT ( 'NONE',  ( -0.1212602504878774051, -0.5073146173917495450, 0.1497995784944541608 ) ) ;
#222 = DIRECTION ( 'NONE',  ( 0.01455087615875037474, 0.9998941303973200023, 4.192763588336697022E-17 ) ) ;
#223 = CIRCLE ( 'NONE', #16616, 0.009999999999999996739 ) ;
#224 = DIRECTION ( 'NONE',  ( 0.4999551463232372317, -0.8660512985181135770, 0.000000000000000000 ) ) ;
#225 = AXIS2_PLACEMENT_3D ( 'NONE', #2754, #12223, #24786 ) ;
#226 = CARTESIAN_POINT ( 'NONE',  ( -0.02000000000000000042, -1.999693152383498207, -0.3073943322174670922 ) ) ;
#227 = CARTESIAN_POINT ( 'NONE',  ( -0.005948725901132494338, -2.107936428766274073, -0.7005084057759867200 ) ) ;
#228 = CARTESIAN_POINT ( 'NONE',  ( 0.3622253751127874066, -1.756884464425453984, -0.4902987826081479650 ) ) ;
#229 = PERSON_AND_ORGANIZATION_ROLE ( 'design_supplier' ) ;
#230 = LINE ( 'NONE', #12724, #21231 ) ;
#231 = CARTESIAN_POINT ( 'NONE',  ( 0.1959177972118346378, -1.369282659305815386, 0.4807434598345527443 ) ) ;
#232 = PLANE ( 'NONE',  #32346 ) ;
#233 = CARTESIAN_POINT ( 'NONE',  ( -0.2746410161513782033, -1.835749455202394298, -0.2938319975228648739 ) ) ;
#234 = CIRCLE ( 'NONE', #1526, 0.01499999999999997689 ) ;
#235 = CARTESIAN_POINT ( 'NONE',  ( 0.1623712441042921006, -1.412506991498796660, 0.8192480828659791658 ) ) ;
#236 = CARTESIAN_POINT ( 'NONE',  ( 6.601686217279748340E-05, -0.6230491400307559546, -0.09540615510927821785 ) ) ;
#237 = CARTESIAN_POINT ( 'NONE',  ( 0.1717449021412840726, -1.802002661843876696, -0.6814448880503549688 ) ) ;
#238 = CYLINDRICAL_SURFACE ( 'NONE', #20468, 0.06000000000000031697 ) ;
#239 = ORIENTED_EDGE ( 'NONE', *, *, #16957, .F. ) ;
#240 = ORIENTED_EDGE ( 'NONE', *, *, #36669, .T. ) ;
#241 = EDGE_CURVE ( 'NONE', #4902, #25362, #16461, .T. ) ;
#242 = CARTESIAN_POINT ( 'NONE',  ( 0.6473787150721044270, -1.455279521797666176, -0.6250000000000000000 ) ) ;
#243 = VERTEX_POINT ( 'NONE', #32631 ) ;
#244 = DIRECTION ( 'NONE',  ( 0.000000000000000000, 0.000000000000000000, -1.000000000000000000 ) ) ;
#245 = CARTESIAN_POINT ( 'NONE',  ( -0.03309057659885150660, -0.5154121718708730704, -0.07470590733143653295 ) ) ;
#246 = VECTOR ( 'NONE', #25682, 39.37007874015748143 ) ;
#247 = EDGE_CURVE ( 'NONE', #13465, #5600, #27350, .T. ) ;
#248 = CARTESIAN_POINT ( 'NONE',  ( 0.5830587952300703147, -1.433043469348942667, 0.7044988243964402930 ) ) ;
#250 = EDGE_LOOP ( 'NONE', ( #22940, #10850, #32575, #22840 ) ) ;
#249 = CARTESIAN_POINT ( 'NONE',  ( -0.1045574869087414066, -0.4741643323009803734, 0.09813923389047436718 ) ) ;
#251 = ORIENTED_EDGE ( 'NONE', *, *, #36675, .F. ) ;
#252 = DIRECTION ( 'NONE',  ( -7.000205099780314469E-17, -1.000000000000000000, 6.590151126658399604E-16 ) ) ;
#253 = VECTOR ( 'NONE', #21136, 39.37007874015748143 ) ;
#254 = ORIENTED_EDGE ( 'NONE', *, *, #22555, .F. ) ;
#255 = AXIS2_PLACEMENT_3D ( 'NONE', #6297, #37978, #40241 ) ;
#256 = CARTESIAN_POINT ( 'NONE',  ( 0.01082074132985459333, -0.5320958912064523982, 0.1749010329950502485 ) ) ;
#258 = DIRECTION ( 'NONE',  ( -0.1520288461498812416, 0.000000000000000000, -0.9883760569430726228 ) ) ;
#257 = CARTESIAN_POINT ( 'NONE',  ( 0.5254844390776584051, -1.675905034379785441, -0.4432393896124048327 ) ) ;
#259 = DIRECTION ( 'NONE',  ( 0.000000000000000000, 0.000000000000000000, -1.000000000000000000 ) ) ;
#260 = EDGE_CURVE ( 'NONE', #19095, #7024, #37850, .T. ) ;
#261 = CARTESIAN_POINT ( 'NONE',  ( 0.1896903302788489343, -0.9196856789278203825, -0.03797464539687132185 ) ) ;
#262 = AXIS2_PLACEMENT_3D ( 'NONE', #17751, #2132, #10998 ) ;
#263 = LINE ( 'NONE', #2895, #2757 ) ;
#265 = ORIENTED_EDGE ( 'NONE', *, *, #7185, .T. ) ;
#264 = ORIENTED_EDGE ( 'NONE', *, *, #34115, .T. ) ;
#266 = CYLINDRICAL_SURFACE ( 'NONE', #14545, 0.08139150547213670761 ) ;
#267 = DIRECTION ( 'NONE',  ( 0.000000000000000000, 0.000000000000000000, 1.000000000000000000 ) ) ;
#268 = AXIS2_PLACEMENT_3D ( 'NONE', #15055, #5784, #18341 ) ;
#269 = CARTESIAN_POINT ( 'NONE',  ( 0.1499999999999994671, 0.3880410510314737382, -0.3755318131855000519 ) ) ;
#270 = DIRECTION ( 'NONE',  ( 0.8660512985181133550, 0.4999551463232373982, 0.000000000000000000 ) ) ;
#271 = AXIS2_PLACEMENT_3D ( 'NONE', #761, #13482, #6887 ) ;
#272 = CARTESIAN_POINT ( 'NONE',  ( 0.2940074227696489184, -1.028172634779288996, 0.7298538202148366905 ) ) ;
#273 = CARTESIAN_POINT ( 'NONE',  ( 0.2184614013223490359, -1.436573476884752676, 0.9287958070571558089 ) ) ;
#274 = EDGE_CURVE ( 'NONE', #16107, #30911, #31280, .T. ) ;
#275 = B_SPLINE_CURVE_WITH_KNOTS ( 'NONE', 3,
 ( #22885, #22270, #22466, #4121, #25752, #3529, #19580, #35404, #26164, #7198, #13001, #13395, #38277, #34994, #25549, #32115, #16292, #38493 ),
 .UNSPECIFIED., .F., .F.,
 ( 4, 2, 2, 2, 2, 2, 2, 2, 4 ),
 ( 0.001290851923713245844, 0.001894763156073155964, 0.002498674388433065868, 0.003102585620792975771, 0.003706496853152886108, 0.004310408085512795577, 0.004914319317872705914, 0.005518230550232615383, 0.006122141782592525720 ),
 .UNSPECIFIED. ) ;
#276 = CARTESIAN_POINT ( 'NONE',  ( 0.2650312354662574532, -1.481736570352484073, 1.013012391360898823 ) ) ;
#277 = EDGE_CURVE ( 'NONE', #20339, #32089, #8062, .T. ) ;
#278 = DIRECTION ( 'NONE',  ( 0.000000000000000000, -3.330669073875469621E-16, -1.000000000000000000 ) ) ;
#279 = DIRECTION ( 'NONE',  ( -1.387778780781449620E-15, -6.590151126658398618E-16, -1.000000000000000000 ) ) ;
#280 = CARTESIAN_POINT ( 'NONE',  ( -0.3000000000000000999, -4.289222312108804225, -0.5708809693675255259 ) ) ;
#281 = CARTESIAN_POINT ( 'NONE',  ( 0.3787041472384312102, -1.708164842082610768, -0.4136294741777339912 ) ) ;
#282 = DIRECTION ( 'NONE',  ( 1.000000000000000000, 0.000000000000000000, 0.000000000000000000 ) ) ;
#283 = CIRCLE ( 'NONE', #37664, 0.07999999999999996003 ) ;
#284 = CARTESIAN_POINT ( 'NONE',  ( -0.3000000000000000999, -2.457388234162025675, -0.5792354969483111127 ) ) ;
#285 = CARTESIAN_POINT ( 'NONE',  ( -0.1743922129835730472, -0.5166151207188712791, 0.08499999999999964528 ) ) ;
#286 = CARTESIAN_POINT ( 'NONE',  ( 0.05954370505521044965, -1.068900277825352907, 0.7381710695662248023 ) ) ;
#287 = DATE_AND_TIME ( #31912, #1733 ) ;
#288 = VECTOR ( 'NONE', #22622, 39.37007874015748143 ) ;
#289 = CARTESIAN_POINT ( 'NONE',  ( -0.05268932808080252495, 0.4428506128075219150, 0.1535014714534106983 ) ) ;
#290 = VECTOR ( 'NONE', #11669, 39.37007874015748143 ) ;
#291 = AXIS2_PLACEMENT_3D ( 'NONE', #15248, #34163, #18534 ) ;
#292 = ORIENTED_EDGE ( 'NONE', *, *, #19551, .T. ) ;
#293 = DIRECTION ( 'NONE',  ( 0.000000000000000000, 0.000000000000000000, -1.000000000000000000 ) ) ;
#294 = EDGE_LOOP ( 'NONE', ( #20612, #17660, #15719, #33560 ) ) ;
#295 = CARTESIAN_POINT ( 'NONE',  ( 0.1145935282722230358, -1.416615153024734397, 0.5154658030382857081 ) ) ;
#296 = CARTESIAN_POINT ( 'NONE',  ( 0.2587121583883757459, -1.613885124491862610, 0.8258352243388695779 ) ) ;
#297 = EDGE_CURVE ( 'NONE', #16265, #14568, #3667, .T. ) ;
#298 = CARTESIAN_POINT ( 'NONE',  ( 0.1324595997283633808, -0.5754775961032010390, 0.2510594539120258872 ) ) ;
#300 = ORIENTED_EDGE ( 'NONE', *, *, #29321, .T. ) ;
#299 = CARTESIAN_POINT ( 'NONE',  ( 0.3434800707737146741, -1.169184835483404905, 0.4282596159937968605 ) ) ;
#302 = ORIENTED_EDGE ( 'NONE', *, *, #13793, .F. ) ;
#301 = ORIENTED_EDGE ( 'NONE', *, *, #27603, .T. ) ;
#303 = CARTESIAN_POINT ( 'NONE',  ( 0.6611732595943385915, -1.536511864384403125, 0.7149362408420358861 ) ) ;
#304 = ORIENTED_EDGE ( 'NONE', *, *, #18503, .T. ) ;
#305 = FACE_OUTER_BOUND ( 'NONE', #5750, .T. ) ;
#306 = APPROVAL_STATUS ( 'not_yet_approved' ) ;
#307 = VECTOR ( 'NONE', #3224, 39.37007874015748143 ) ;
#308 = CARTESIAN_POINT ( 'NONE',  ( 0.3098923999789689465, -1.765709567672198554, 0.5653262919047477020 ) ) ;
#309 = ORIENTED_EDGE ( 'NONE', *, *, #24920, .F. ) ;
#310 = CARTESIAN_POINT ( 'NONE',  ( 0.08557407651291307205, -0.7673689209508794962, 0.1706946678738483492 ) ) ;
#311 = AXIS2_PLACEMENT_3D ( 'NONE', #4661, #14149, #11266 ) ;
#312 = DIRECTION ( 'NONE',  ( 8.881784197001246407E-16, -2.361472542561082612E-16, 1.000000000000000000 ) ) ;
#313 = CARTESIAN_POINT ( 'NONE',  ( 0.4632380810071169974, -1.418384998081447357, 0.8128757890859310553 ) ) ;
#314 = CARTESIAN_POINT ( 'NONE',  ( 0.5747203984579013492, -1.612743926285909346, -0.5166151207188712791 ) ) ;
#315 = CARTESIAN_POINT ( 'NONE',  ( -0.1542132178619276262, 0.4779941576916627022, 0.1100664889103354915 ) ) ;
#316 = ORIENTED_EDGE ( 'NONE', *, *, #23007, .T. ) ;
#317 = CARTESIAN_POINT ( 'NONE',  ( 0.4382936615902019439, -1.691409853567093613, 0.6111383081645538340 ) ) ;
#318 = CARTESIAN_POINT ( 'NONE',  ( 0.6861498661271836497, -1.412370093654202963, 0.8150029156550121501 ) ) ;
#319 = VECTOR ( 'NONE', #8754, 39.37007874015748854 ) ;
#320 = DIRECTION ( 'NONE',  ( 0.000000000000000000, 0.8159412518334724362, 0.5781348229923756188 ) ) ;
#321 = CARTESIAN_POINT ( 'NONE',  ( 0.6089727181761853680, -1.479025121845506385, 0.5718834518386042287 ) ) ;
#322 = AXIS2_PLACEMENT_3D ( 'NONE', #31448, #24882, #34726 ) ;
#323 = CARTESIAN_POINT ( 'NONE',  ( -0.1553124468364829591, 0.4816356660588166916, 0.3589899338161261499 ) ) ;
#324 =( CONVERSION_BASED_UNIT ( 'INCH', #19000 ) LENGTH_UNIT ( ) NAMED_UNIT ( #4430 ) );
#325 = EDGE_CURVE ( 'NONE', #12308, #507, #36520, .T. ) ;
#326 = CARTESIAN_POINT ( 'NONE',  ( 0.05583995664670776682, -1.335624775257321817, 0.3157417262808777658 ) ) ;
#327 = CARTESIAN_POINT ( 'NONE',  ( -0.2746410161513776482, -3.941790907013290823, -0.009415996779116623042 ) ) ;
#328 = DIRECTION ( 'NONE',  ( 0.000000000000000000, 0.8660477418057301868, -0.4999613074160793036 ) ) ;
#329 = CARTESIAN_POINT ( 'NONE',  ( 0.1932042024315755446, -0.7994606748157702114, 0.2910003379690608294 ) ) ;
#330 = APPROVAL_STATUS ( 'not_yet_approved' ) ;
#331 = DIRECTION ( 'NONE',  ( -7.771561172376107616E-16, 7.170354002788761615E-17, -1.000000000000000000 ) ) ;
#332 = VECTOR ( 'NONE', #28229, 39.37007874015748143 ) ;
#333 = AXIS2_PLACEMENT_3D ( 'NONE', #23656, #17661, #2039 ) ;
#334 = CARTESIAN_POINT ( 'NONE',  ( 0.5142508901037518010, -1.533077155716542572, 0.5735235060962670106 ) ) ;
#335 = CARTESIAN_POINT ( 'NONE',  ( -0.04085667396267392976, -0.02117046819984700137, 0.4712948116111314589 ) ) ;
#336 = AXIS2_PLACEMENT_3D ( 'NONE', #23789, #35713, #20491 ) ;
#337 = ORIENTED_EDGE ( 'NONE', *, *, #31529, .T. ) ;
#338 = CARTESIAN_POINT ( 'NONE',  ( 0.3516101416147200953, -1.741639419776285891, -0.7019724635597545115 ) ) ;
#339 = DIRECTION ( 'NONE',  ( 0.000000000000000000, 0.000000000000000000, -1.000000000000000000 ) ) ;
#340 = CARTESIAN_POINT ( 'NONE',  ( 0.1860255769997808117, -0.8548752387040396972, 0.1809200802102173822 ) ) ;
#341 = EDGE_LOOP ( 'NONE', ( #30120, #14606, #19680, #33856 ) ) ;
#342 = CARTESIAN_POINT ( 'NONE',  ( 0.4091335057472371695, -1.131547141905885789, 0.4177417262808780229 ) ) ;
#343 = CIRCLE ( 'NONE', #37090, 0.1000000000000008521 ) ;
#344 = CARTESIAN_POINT ( 'NONE',  ( -0.009649777317831131213, -0.8763596202099832588, 0.4395725020134745309 ) ) ;
#346 = ORIENTED_EDGE ( 'NONE', *, *, #34113, .T. ) ;
#345 = EDGE_LOOP ( 'NONE', ( #25760, #18511, #17241, #27769 ) ) ;
#347 = CARTESIAN_POINT ( 'NONE',  ( -0.01548846960707531660, -0.2306506793134033284, 0.4716198300880330985 ) ) ;
#348 = AXIS2_PLACEMENT_3D ( 'NONE', #34589, #18959, #3519 ) ;
#349 = EDGE_LOOP ( 'NONE', ( #38087, #24896, #35519, #8395 ) ) ;
#350 = DIRECTION ( 'NONE',  ( 1.664003471950577032E-31, 3.330669073875470607E-16, 1.000000000000000000 ) ) ;
#351 = CARTESIAN_POINT ( 'NONE',  ( 0.3840974138826053763, -1.688245147359099363, -0.3350098725068151317 ) ) ;
#352 = CARTESIAN_POINT ( 'NONE',  ( -0.2399999999999999079, -1.804235510932644004, -0.1501860188971498311 ) ) ;
#353 = CARTESIAN_POINT ( 'NONE',  ( 0.1909286924077255032, -1.257064795538239022, -0.7462941026102624109 ) ) ;
#354 = VERTEX_POINT ( 'NONE', #32817 ) ;
#355 = CARTESIAN_POINT ( 'NONE',  ( -0.2399999999999999079, -1.739646749720735741, -0.3661865639197241507 ) ) ;
#356 = VERTEX_POINT ( 'NONE', #17196 ) ;
#357 = VERTEX_POINT ( 'NONE', #20912 ) ;
#358 = CARTESIAN_POINT ( 'NONE',  ( 0.1233651857933633078, -0.6859638927695101973, 0.4603130361914588020 ) ) ;
#359 = ORIENTED_EDGE ( 'NONE', *, *, #38638, .T. ) ;
#360 = ORIENTED_EDGE ( 'NONE', *, *, #18286, .F. ) ;
#361 = CYLINDRICAL_SURFACE ( 'NONE', #26001, 0.06250000000000001388 ) ;
#362 = CARTESIAN_POINT ( 'NONE',  ( 0.1767352294523506506, -0.9049482756361506564, 0.7300595450672812126 ) ) ;
#364 = DIRECTION ( 'NONE',  ( 0.8150167559926670968, 0.5794373887239150367, 0.000000000000000000 ) ) ;
#363 = CARTESIAN_POINT ( 'NONE',  ( 0.002296835029420831766, -0.5198933010532058585, 0.1654604498185965056 ) ) ;
#365 = LINE ( 'NONE', #31390, #21816 ) ;
#366 = CARTESIAN_POINT ( 'NONE',  ( 0.4548150350199453018, -1.105354657904178861, 0.5682417262808776570 ) ) ;
#367 = ORIENTED_EDGE ( 'NONE', *, *, #29637, .T. ) ;
#368 = AXIS2_PLACEMENT_3D ( 'NONE', #20608, #11332, #1490 ) ;
#369 = DIRECTION ( 'NONE',  ( 0.000000000000000000, 0.000000000000000000, 1.000000000000000000 ) ) ;
#370 = CARTESIAN_POINT ( 'NONE',  ( 0.3938780453836632223, -1.723328632354485634, -0.3054719800402591612 ) ) ;
#371 = CIRCLE ( 'NONE', #14113, 0.08000000000000000167 ) ;
#372 = CARTESIAN_POINT ( 'NONE',  ( 0.1936977043547155886, -0.7769779101379276076, 0.5892091259747814780 ) ) ;
#373 = B_SPLINE_CURVE_WITH_KNOTS ( 'NONE', 3,
 ( #29818, #10683, #13963, #23257 ),
 .UNSPECIFIED., .F., .F.,
 ( 4, 4 ),
 ( 8.673617379883828435E-19, 0.0003934542678113513874 ),
 .UNSPECIFIED. ) ;
#374 = CARTESIAN_POINT ( 'NONE',  ( -0.03654364704248851820, 0.3642884434513001812, 0.3592365245254293682 ) ) ;
#375 = TOROIDAL_SURFACE ( 'NONE', #39044, 0.04500000000000032446, 0.01499999999999999944 ) ;
#376 = AXIS2_PLACEMENT_3D ( 'NONE', #39921, #11130, #1488 ) ;
#377 = CYLINDRICAL_SURFACE ( 'NONE', #1513, 0.08749999999977554899 ) ;
#378 = APPLIED_APPROVAL_ASSIGNMENT ( #13213, ( #20515 ) ) ;
#379 = LINE ( 'NONE', #28716, #2161 ) ;
#380 = CARTESIAN_POINT ( 'NONE',  ( 0.4446247626930326380, -1.240635375613917901, 0.8187945045632878394 ) ) ;
#381 = CARTESIAN_POINT ( 'NONE',  ( -0.002282498291095993656, -0.8555267327002353817, 0.1457185332388701293 ) ) ;
#382 = EDGE_CURVE ( 'NONE', #8839, #6763, #10547, .T. ) ;
#383 = VECTOR ( 'NONE', #13117, 39.37007874015748143 ) ;
#384 = CARTESIAN_POINT ( 'NONE',  ( 0.2254586261693722060, -0.6723955984770768612, 0.4589204916406527945 ) ) ;
#385 = CARTESIAN_POINT ( 'NONE',  ( 0.5383058276557359800, -1.161081979360616190, 0.5534299176528929554 ) ) ;
#386 = CARTESIAN_POINT ( 'NONE',  ( 0.02977708404944962722, -1.115570236398492066, 0.6630177360434016398 ) ) ;
#387 = EDGE_CURVE ( 'NONE', #5797, #36330, #29303, .T. ) ;
#388 = CARTESIAN_POINT ( 'NONE',  ( 0.05279755784604305002, 0.4315508301037734862, -0.1821553064136585964 ) ) ;
#389 = CARTESIAN_POINT ( 'NONE',  ( 0.2110034642138055860, -1.187742706213460453, -0.5155029497116575543 ) ) ;
#390 = B_SPLINE_CURVE_WITH_KNOTS ( 'NONE', 3,
 ( #34289, #36761, #25033, #40256, #31227, #40473, #12295, #18058, #9393, #6095 ),
 .UNSPECIFIED., .F., .F.,
 ( 4, 2, 2, 2, 4 ),
 ( 0.0003323657284514935093, 0.0008074047817991935900, 0.001282443835146893779, 0.001757482888494593751, 0.002232521941842293724 ),
 .UNSPECIFIED. ) ;
#391 = ADVANCED_FACE ( 'NONE', ( #29743 ), #11571, .T. ) ;
#392 = CARTESIAN_POINT ( 'NONE',  ( 0.02231181081520647314, 0.2417894035777236605, -0.4519954025055041846 ) ) ;
#393 = CARTESIAN_POINT ( 'NONE',  ( 0.6298776228253546439, -1.586001970545553252, 0.4270054416526937735 ) ) ;
#394 = VERTEX_POINT ( 'NONE', #5240 ) ;
#395 = DIRECTION ( 'NONE',  ( -0.8660512985181134660, -0.4999551463232372872, 0.000000000000000000 ) ) ;
#396 = CARTESIAN_POINT ( 'NONE',  ( 0.2698036132048247104, -0.9625005881386677897, 0.7146062034794288254 ) ) ;
#397 = AXIS2_PLACEMENT_3D ( 'NONE', #958, #6665, #10380 ) ;
#398 = CARTESIAN_POINT ( 'NONE',  ( 0.3641487592347181779, -1.992207614157224249, -0.4748857690446578461 ) ) ;
#399 = CARTESIAN_POINT ( 'NONE',  ( 0.5319948190214550676, -1.638784817636518287, -0.4758175433331751081 ) ) ;
#400 = CARTESIAN_POINT ( 'NONE',  ( 0.03113248654051816583, 0.5209315849442470725, 0.3202538583802974070 ) ) ;
#401 = AXIS2_PLACEMENT_3D ( 'NONE', #26984, #15048, #39733 ) ;
#402 = ORIENTED_EDGE ( 'NONE', *, *, #3753, .T. ) ;
#403 = CARTESIAN_POINT ( 'NONE',  ( 0.1999999999999787226, -2.097675824466502803, -0.4688691127277801463 ) ) ;
#404 = ADVANCED_FACE ( 'NONE', ( #14313 ), #17794, .F. ) ;
#405 = CARTESIAN_POINT ( 'NONE',  ( 0.1873756208929918121, -1.374400995849163198, 0.4173619172664751464 ) ) ;
#406 = LOCAL_TIME ( 0, 53, 7.000000000000000000, #6026 ) ;
#407 = DIRECTION ( 'NONE',  ( 0.000000000000000000, 0.000000000000000000, -1.000000000000000000 ) ) ;
#408 = APPROVAL ( #6631, 'UNSPECIFIED' ) ;
#409 = SPHERICAL_SURFACE ( 'NONE', #10121, 0.01499999999999999944 ) ;
#410 = CARTESIAN_POINT ( 'NONE',  ( 0.5095436923513168015, -1.308647369734698085, 0.6228639752712391564 ) ) ;
#412 = CARTESIAN_POINT ( 'NONE',  ( -0.05464101615137763324, -1.772778095317936620, -0.3120197613628935551 ) ) ;
#411 = LINE ( 'NONE', #35317, #2910 ) ;
#413 = CARTESIAN_POINT ( 'NONE',  ( 0.4929465528686915454, -1.082715557938388029, 0.5653634300333020279 ) ) ;
#414 = ORIENTED_EDGE ( 'NONE', *, *, #21024, .T. ) ;
#415 = APPROVAL_ROLE ( '' ) ;
#416 = VECTOR ( 'NONE', #18339, 39.37007874015748143 ) ;
#417 = ORIENTED_EDGE ( 'NONE', *, *, #17337, .F. ) ;
#418 =( BOUNDED_SURFACE ( )  B_SPLINE_SURFACE ( 3, 2, ( 
 ( #38846, #4085, #28600 ),
 ( #35565, #1253, #6769 ),
 ( #34961, #10292, #22857 ),
 ( #35775, #4301, #13147 ),
 ( #7364, #19941, #16866 ),
 ( #3495, #19138, #19347 ),
 ( #25936, #31677, #16055 ),
 ( #3704, #25711, #38242 ),
 ( #10073, #19552, #4493 ),
 ( #39066, #10892, #23650 ),
 ( #2246, #24251, #26526 ),
 ( #5099, #33483, #26737 ),
 ( #17055, #20556, #36171 ),
 ( #17464, #39663, #33090 ),
 ( #29601, #39459, #26926 ),
 ( #14785, #11284, #4686 ),
 ( #13956, #29809, #23464 ),
 ( #17256, #32688, #23851 ),
 ( #1443, #35980, #4898 ),
 ( #30203, #7585, #1847 ),
 ( #36376, #11500, #8195 ),
 ( #7786, #27132, #11696 ),
 ( #36590, #17853, #20355 ),
 ( #20767, #32876, #1650 ),
 ( #8392, #7980, #39877 ),
 ( #33290, #30017, #2034 ),
 ( #14362, #14169, #17657 ),
 ( #14565, #39267, #11090 ),
 ( #24064, #20963, #5289 ),
 ( #27346, #30415, #20160 ) ),
 .UNSPECIFIED., .F., .F., .F. ) 
 B_SPLINE_SURFACE_WITH_KNOTS ( ( 4, 2, 2, 2, 2, 2, 2, 2, 2, 2, 2, 2, 2, 2, 4 ),
 ( 3, 3 ),
 ( 1.192622389734054877E-18, 0.0008889885672519496837, 0.001333482850877924092, 0.001777977134503898283, 0.002222471418129872475, 0.002666965701755846883, 0.003111459985381820857, 0.003555954269007795265, 0.004000448552633769674, 0.004444942836259744082, 0.004889437119885718490, 0.005333931403511692898, 0.005778425687137667306, 0.006222919970763641714, 0.007111908538015589663 ),
 ( 0.000000000000000000, 1.000000000000000000 ),
 .UNSPECIFIED. ) 
 GEOMETRIC_REPRESENTATION_ITEM ( )  RATIONAL_B_SPLINE_SURFACE ( (
 ( 1.000000000000000000, 0.7087966873486397645, 1.000000000000000000),
 ( 1.000000000000000000, 0.7254043283289703936, 1.000000000000000000),
 ( 1.000000000000000000, 0.7477302227775445287, 1.000000000000000000),
 ( 1.000000000000000000, 0.7823973320993324876, 1.000000000000000000),
 ( 1.000000000000000000, 0.7940349421475684233, 1.000000000000000000),
 ( 1.000000000000000000, 0.8170648074608825029, 1.000000000000000000),
 ( 1.000000000000000000, 0.8285120912207648569, 1.000000000000000000),
 ( 1.000000000000000000, 0.8502521819941248893, 1.000000000000000000),
 ( 1.000000000000000000, 0.8606365733870987578, 1.000000000000000000),
 ( 1.000000000000000000, 0.8803670527789597688, 1.000000000000000000),
 ( 1.000000000000000000, 0.8897136316908171860, 1.000000000000000000),
 ( 1.000000000000000000, 0.9068004400909128737, 1.000000000000000000),
 ( 1.000000000000000000, 0.9146221070091428151, 1.000000000000000000),
 ( 1.000000000000000000, 0.9288284161271825878, 1.000000000000000000),
 ( 1.000000000000000000, 0.9352460323245295193, 1.000000000000000000),
 ( 1.000000000000000000, 0.9462102292809775328, 1.000000000000000000),
 ( 1.000000000000000000, 0.9508087505105436987, 1.000000000000000000),
 ( 1.000000000000000000, 0.9581430234375604149, 1.000000000000000000),
 ( 1.000000000000000000, 0.9608521639589725494, 1.000000000000000000),
 ( 1.000000000000000000, 0.9639951171735293700, 1.000000000000000000),
 ( 1.000000000000000000, 0.9644675829175349824, 1.000000000000000000),
 ( 1.000000000000000000, 0.9630894221799249921, 1.000000000000000000),
 ( 1.000000000000000000, 0.9612789446135701077, 1.000000000000000000),
 ( 1.000000000000000000, 0.9555297994135374395, 1.000000000000000000),
 ( 1.000000000000000000, 0.9515877792135777336, 1.000000000000000000),
 ( 1.000000000000000000, 0.9419945274880047181, 1.000000000000000000),
 ( 1.000000000000000000, 0.9363124543101019048, 1.000000000000000000),
 ( 1.000000000000000000, 0.9165938519170033771, 1.000000000000000000),
 ( 1.000000000000000000, 0.9002247319857109575, 1.000000000000000000),
 ( 1.000000000000000000, 0.8810606863760693797, 1.000000000000000000) ) ) 
 REPRESENTATION_ITEM ( '' )  SURFACE ( )  );
#419 = CARTESIAN_POINT ( 'NONE',  ( 0.04148277367085517059, -0.5962918094959076543, 0.3490695081863538496 ) ) ;
#421 = CARTESIAN_POINT ( 'NONE',  ( 0.2484857473122376870, -1.339293634572156000, -0.5155029497116575543 ) ) ;
#420 = CARTESIAN_POINT ( 'NONE',  ( 0.08668618681611810206, -0.7427351849914437532, 0.03552623599536654242 ) ) ;
#422 = CARTESIAN_POINT ( 'NONE',  ( 0.5054609057099638258, -1.017757956463559710, -0.5155029497116575543 ) ) ;
#423 = ORIENTED_EDGE ( 'NONE', *, *, #13770, .T. ) ;
#424 = ORIENTED_EDGE ( 'NONE', *, *, #40222, .F. ) ;
#425 = CARTESIAN_POINT ( 'NONE',  ( -0.1157263453858495550, -0.4799749855354071837, 0.1178658435936998650 ) ) ;
#426 = CARTESIAN_POINT ( 'NONE',  ( 0.5604574556245232042, -1.488111770035372983, 0.6880931705970741996 ) ) ;
#427 = ORIENTED_EDGE ( 'NONE', *, *, #16448, .F. ) ;
#428 = CARTESIAN_POINT ( 'NONE',  ( 0.06747690200236802771, -1.330070943150462925, 0.5060650602545776477 ) ) ;
#429 = B_SPLINE_CURVE_WITH_KNOTS ( 'NONE', 3,
 ( #33409, #30321, #2154, #27259, #8510, #21076, #33600, #25899, #40396, #39981, #9535, #33825, #37107, #27858, #12221, #14899, #24784, #31148, #37303, #15091, #9116, #21681, #34211, #36898, #18379, #6023 ),
 .UNSPECIFIED., .F., .F.,
 ( 4, 2, 2, 2, 2, 2, 2, 2, 2, 2, 2, 2, 4 ),
 ( 0.02890318467689641582, 0.02962064806864088753, 0.03033811146038536272, 0.03177303824387431308, 0.03320796502736327038, 0.03464289181085222769, 0.03607781859434118499, 0.03751274537783013535, 0.04038259894480807077, 0.04325245251178599926, 0.04612230607876392774, 0.04899215964574185622, 0.05186201321271978470 ),
 .UNSPECIFIED. ) ;
#430 = CARTESIAN_POINT ( 'NONE',  ( 0.06724117332272876169, -1.895739979645849838, -0.3418766208214948921 ) ) ;
#431 = CARTESIAN_POINT ( 'NONE',  ( 0.1499999999999994948, 0.2306506793134049660, -0.4716198300880325434 ) ) ;
#432 = DIRECTION ( 'NONE',  ( -7.000205099780314469E-17, -1.000000000000000000, 6.590151126658399604E-16 ) ) ;
#433 = VERTEX_POINT ( 'NONE', #39601 ) ;
#434 = CARTESIAN_POINT ( 'NONE',  ( -0.02000000000000000042, -1.599201040860868339, 0.1642182323853691728 ) ) ;
#435 = DIRECTION ( 'NONE',  ( 0.000000000000000000, 0.000000000000000000, -1.000000000000000000 ) ) ;
#436 = CARTESIAN_POINT ( 'NONE',  ( -0.1211772861969157844, -0.5069185045468641571, 0.1468025672055966735 ) ) ;
#437 = AXIS2_PLACEMENT_3D ( 'NONE', #21342, #24418, #27501 ) ;
#438 = ADVANCED_FACE ( 'NONE', ( #1586, #1798 ), #33433, .F. ) ;
#439 = DIRECTION ( 'NONE',  ( 0.000000000000000000, 0.000000000000000000, -1.000000000000000000 ) ) ;
#440 = EDGE_CURVE ( 'NONE', #15736, #13839, #35714, .T. ) ;
#441 = SPHERICAL_SURFACE ( 'NONE', #7998, 0.01499999999999999944 ) ;
#442 = DIRECTION ( 'NONE',  ( 0.4999551463232373427, -0.8660512985181134660, 0.000000000000000000 ) ) ;
#443 = DIRECTION ( 'NONE',  ( 0.000000000000000000, -0.9215515678030121727, -0.3882559824134206306 ) ) ;
#444 = PERSON_AND_ORGANIZATION ( #28500, #32463 ) ;
#445 = SECURITY_CLASSIFICATION ( '', '', #25659 ) ;
#446 = EDGE_CURVE ( 'NONE', #15271, #15727, #25800, .T. ) ;
#447 = EDGE_CURVE ( 'NONE', #8445, #7904, #17904, .T. ) ;
#448 = CARTESIAN_POINT ( 'NONE',  ( 0.4885592119991905014, -1.080308374838712782, 0.5952236481819053182 ) ) ;
#449 = CARTESIAN_POINT ( 'NONE',  ( 0.1676694287369189240, -1.385544946528693089, 0.5182417262812420988 ) ) ;
#450 = EDGE_CURVE ( 'NONE', #9282, #2281, #5151, .T. ) ;
#451 = CARTESIAN_POINT ( 'NONE',  ( 0.5494247343383880100, -1.165528289934207429, 0.5856983068965392336 ) ) ;
#452 = CARTESIAN_POINT ( 'NONE',  ( 0.2633622372885912610, -1.685028111793015926, 0.5636491875944877883 ) ) ;
#453 = CARTESIAN_POINT ( 'NONE',  ( 0.1861033513463754285, -1.549633035783825497, 0.5860151309145639198 ) ) ;
#454 = CARTESIAN_POINT ( 'NONE',  ( 0.5843363353628658885, -1.492391990693552328, -0.4353912382336290188 ) ) ;
#455 = DIRECTION ( 'NONE',  ( 0.000000000000000000, 3.330669073875469621E-16, 1.000000000000000000 ) ) ;
#456 = CARTESIAN_POINT ( 'NONE',  ( 0.3377018382744822467, -1.172509963254503518, 0.4282583286688060875 ) ) ;
#457 = ORIENTED_EDGE ( 'NONE', *, *, #17968, .F. ) ;
#458 = ORIENTED_EDGE ( 'NONE', *, *, #30646, .F. ) ;
#459 = ADVANCED_FACE ( 'NONE', ( #34241 ), #21807, .T. ) ;
#460 = ORIENTED_EDGE ( 'NONE', *, *, #16592, .T. ) ;
#461 = CARTESIAN_POINT ( 'NONE',  ( 0.7053289366243524761, -1.513890837374202158, 0.5668602961216192559 ) ) ;
#462 = CARTESIAN_POINT ( 'NONE',  ( -0.04582889109739221589, -0.4790149006698679046, -0.08746027838083869632 ) ) ;
#463 = CARTESIAN_POINT ( 'NONE',  ( 0.3843292633124594238, -1.119501845244787130, 0.8107229143054137666 ) ) ;
#465 = ORIENTED_EDGE ( 'NONE', *, *, #25908, .T. ) ;
#464 = DIRECTION ( 'NONE',  ( 0.000000000000000000, -0.5877852522924817968, -0.8090169943749412340 ) ) ;
#466 = VECTOR ( 'NONE', #25583, 39.37007874015748854 ) ;
#467 = ORIENTED_EDGE ( 'NONE', *, *, #19807, .T. ) ;
#468 = CARTESIAN_POINT ( 'NONE',  ( 0.5641757645307916569, -1.616462539050035785, 0.4683090780955098120 ) ) ;
#469 = ORIENTED_EDGE ( 'NONE', *, *, #4281, .F. ) ;
#470 = CARTESIAN_POINT ( 'NONE',  ( 0.3010413997904062278, -1.655300281042359600, 0.6398421476192419632 ) ) ;
#472 = CARTESIAN_POINT ( 'NONE',  ( -0.02869712619511769966, -0.4519224903895721068, 0.2102851490355757691 ) ) ;
#471 = CARTESIAN_POINT ( 'NONE',  ( 0.5368241748133022462, -1.669358817950476137, -0.4818844110025696237 ) ) ;
#473 = CARTESIAN_POINT ( 'NONE',  ( -0.2399999999999999079, -2.427691829037316396, -0.9241619397096791921 ) ) ;
#474 = DIRECTION ( 'NONE',  ( 0.8660512985181135770, 0.4999551463232370652, 0.000000000000000000 ) ) ;
#475 = CARTESIAN_POINT ( 'NONE',  ( 0.01173648626945268322, -0.6872203660140956405, -0.1131804859792006068 ) ) ;
#476 = CARTESIAN_POINT ( 'NONE',  ( -0.1127677449505191248, -0.5183788106019665554, 0.3108513529153781318 ) ) ;
#478 = VERTEX_POINT ( 'NONE', #40208 ) ;
#477 = ORIENTED_EDGE ( 'NONE', *, *, #21320, .F. ) ;
#479 = CARTESIAN_POINT ( 'NONE',  ( 0.3902040701542698331, -1.764767632342756798, -0.4833641654129184895 ) ) ;
#480 = CIRCLE ( 'NONE', #25394, 0.4615209409081865166 ) ;
#481 = CARTESIAN_POINT ( 'NONE',  ( 0.1854061228264040906, -0.8389673959738600528, 0.1645307725974398116 ) ) ;
#482 = CARTESIAN_POINT ( 'NONE',  ( -0.05078493045284376145, -0.4330747843660891494, 0.1920285438095919728 ) ) ;
#483 = CARTESIAN_POINT ( 'NONE',  ( 0.5876954366397778573, -1.441089883205937117, 0.7245674945195832439 ) ) ;
#484 = CARTESIAN_POINT ( 'NONE',  ( 0.2595046455490389592, -0.9774713019456258145, 0.6992928735491890091 ) ) ;
#485 = CYLINDRICAL_SURFACE ( 'NONE', #13922, 0.1000000000000000194 ) ;
#486 = CARTESIAN_POINT ( 'NONE',  ( 0.4848298080272115396, -1.171730077801051539, 0.4182417262808777458 ) ) ;
#487 = CARTESIAN_POINT ( 'NONE',  ( -0.2399999999999999079, -2.718308734057149678, -0.5229705402004846126 ) ) ;
#488 = EDGE_CURVE ( 'NONE', #27736, #11923, #6051, .T. ) ;
#489 = CARTESIAN_POINT ( 'NONE',  ( 0.7476847780466161497, -1.513986987551942498, 0.3667417262808780887 ) ) ;
#490 = CARTESIAN_POINT ( 'NONE',  ( 0.4237998664792062553, -1.180002069003335929, 0.7229979235705997764 ) ) ;
#491 = CARTESIAN_POINT ( 'NONE',  ( 0.3998481532917401160, -1.682844229318920304, -0.4042724543747899246 ) ) ;
#492 = EDGE_CURVE ( 'NONE', #18074, #24668, #16830, .T. ) ;
#493 = AXIS2_PLACEMENT_3D ( 'NONE', #36564, #2611, #5267 ) ;
#494 = DIRECTION ( 'NONE',  ( 0.000000000000000000, 0.000000000000000000, -1.000000000000000000 ) ) ;
#495 = EDGE_CURVE ( 'NONE', #990, #7711, #37493, .T. ) ;
#496 = CARTESIAN_POINT ( 'NONE',  ( 0.09580854502948936424, -0.9100554415251292939, 0.8942175666832257175 ) ) ;
#497 = CARTESIAN_POINT ( 'NONE',  ( 0.1189259589201130257, -1.413964385820541736, 0.5805317459970470440 ) ) ;
#498 = SHAPE_DEFINITION_REPRESENTATION ( #951, #40103 ) ;
#499 = APPLIED_APPROVAL_ASSIGNMENT ( #11774, ( #30020 ) ) ;
#500 = EDGE_CURVE ( 'NONE', #40212, #36370, #23396, .T. ) ;
#501 = DIRECTION ( 'NONE',  ( 0.000000000000000000, -0.7185945389471800615, 0.6954292836768448671 ) ) ;
#502 = CARTESIAN_POINT ( 'NONE',  ( -0.03875673594170897518, 0.4622647171927845577, 0.1151965740700969104 ) ) ;
#503 = CARTESIAN_POINT ( 'NONE',  ( 0.01548846960721238578, 0.07651041855108486889, -0.5222379212565272377 ) ) ;
#504 = CIRCLE ( 'NONE', #8333, 0.02999999999999995379 ) ;
#505 = ORIENTED_EDGE ( 'NONE', *, *, #13643, .T. ) ;
#506 = CARTESIAN_POINT ( 'NONE',  ( 0.1962654359417508876, -0.5719901442833904559, 0.2972479173850666734 ) ) ;
#507 = VERTEX_POINT ( 'NONE', #18837 ) ;
#508 = CARTESIAN_POINT ( 'NONE',  ( 0.1070125746715546999, -1.413633491471445458, 0.5553720351514388476 ) ) ;
#509 = DIRECTION ( 'NONE',  ( -7.771561172376107616E-16, 7.170354002788761615E-17, -1.000000000000000000 ) ) ;
#510 = EDGE_CURVE ( 'NONE', #1876, #18789, #14721, .T. ) ;
#511 = CARTESIAN_POINT ( 'NONE',  ( 0.1313907764345140505, -0.5643515122363669256, 0.2179657342365748374 ) ) ;
#513 = EDGE_LOOP ( 'NONE', ( #35888, #34743, #40576, #33330 ) ) ;
#512 = CARTESIAN_POINT ( 'NONE',  ( 0.4843318811940854340, -1.649192016167395192, -0.4000974106332781388 ) ) ;
#514 = EDGE_CURVE ( 'NONE', #10550, #11729, #5072, .T. ) ;
#516 = ORIENTED_EDGE ( 'NONE', *, *, #2607, .T. ) ;
#515 = ORIENTED_EDGE ( 'NONE', *, *, #8471, .T. ) ;
#517 = CARTESIAN_POINT ( 'NONE',  ( 0.6572694620505376006, -1.525419925066909155, 0.7402068353553745705 ) ) ;
#518 = ORIENTED_EDGE ( 'NONE', *, *, #17003, .T. ) ;
#519 = CARTESIAN_POINT ( 'NONE',  ( -0.05464101615137796630, -1.646519645934556131, -0.1171471737359304072 ) ) ;
#520 = COORDINATED_UNIVERSAL_TIME_OFFSET ( 0, 0, .AHEAD. ) ;
#521 = DIRECTION ( 'NONE',  ( 1.000000000000000000, 0.000000000000000000, 0.000000000000000000 ) ) ;
#522 = EDGE_LOOP ( 'NONE', ( #22192, #34276, #11323, #16636 ) ) ;
#523 = CARTESIAN_POINT ( 'NONE',  ( 0.1213365863176824183, -0.8079515073422893767, 0.4383441164392827272 ) ) ;
#524 = DIRECTION ( 'NONE',  ( 0.000000000000000000, -0.5877852522924708056, 0.8090169943749491166 ) ) ;
#525 = CARTESIAN_POINT ( 'NONE',  ( 0.5391969560877111212, -1.519063423995081097, 0.5750070075651220192 ) ) ;
#526 = CARTESIAN_POINT ( 'NONE',  ( -0.2746410161513779258, -3.705001275441084818, -0.3950781284944322458 ) ) ;
#527 = CARTESIAN_POINT ( 'NONE',  ( -0.1566201954065912505, 0.4859225043295721247, 0.1133527062597488727 ) ) ;
#528 = VERTEX_POINT ( 'NONE', #1489 ) ;
#529 = CARTESIAN_POINT ( 'NONE',  ( 0.4741118015397497998, -1.670572742253769727, 0.5762195691663208885 ) ) ;
#530 = CARTESIAN_POINT ( 'NONE',  ( 0.6665471296844990290, -1.561491147660964307, 0.5827599307756513580 ) ) ;
#531 = ORIENTED_EDGE ( 'NONE', *, *, #39085, .F. ) ;
#532 = CARTESIAN_POINT ( 'NONE',  ( 0.4528004050422974602, -1.638392014206256020, -0.6172987386429681367 ) ) ;
#533 = CARTESIAN_POINT ( 'NONE',  ( 0.6089456720007967450, -1.479017793199127073, 0.5713140754762677798 ) ) ;
#534 = CARTESIAN_POINT ( 'NONE',  ( 0.05562144613422553147, -0.4441896308501024349, 0.1229845283801415390 ) ) ;
#535 = ADVANCED_FACE ( 'NONE', ( #35824 ), #9561, .F. ) ;
#536 = CARTESIAN_POINT ( 'NONE',  ( 0.1437340355044557927, -1.283861693981850349, 0.4177417262808780229 ) ) ;
#537 = CARTESIAN_POINT ( 'NONE',  ( 0.4422358757816878816, -1.108045738334233254, -0.3965663110662911994 ) ) ;
#538 = ADVANCED_FACE ( 'NONE', ( #23087 ), #29927, .T. ) ;
#539 = CARTESIAN_POINT ( 'NONE',  ( 1.365923996832131609E-16, -0.9481888444201341803, 0.1298224387748352637 ) ) ;
#540 = CARTESIAN_POINT ( 'NONE',  ( 0.5133443775832216005, -1.117606250044787863, 0.5819851345710455037 ) ) ;
#541 = PERSON_AND_ORGANIZATION_ROLE ( 'classification_officer' ) ;
#542 = DIRECTION ( 'NONE',  ( -6.162975822039154730E-33, 0.000000000000000000, -1.000000000000000000 ) ) ;
#543 = CARTESIAN_POINT ( 'NONE',  ( -0.02231181081520762152, 0.5045902076536090686, -0.09028112709016213044 ) ) ;
#544 = CARTESIAN_POINT ( 'NONE',  ( -0.03301200226531592757, 0.08829440931815854543, 0.5134711413293278071 ) ) ;
#545 = VERTEX_POINT ( 'NONE', #9758 ) ;
#546 = CARTESIAN_POINT ( 'NONE',  ( 0.4409062655693438137, -1.690090444797295977, -0.7462941026102624109 ) ) ;
#547 = CARTESIAN_POINT ( 'NONE',  ( -0.2746410161513779258, -3.291368864184587739, -0.6988176298300774469 ) ) ;
#548 = CARTESIAN_POINT ( 'NONE',  ( 0.08873715221104290507, -0.6057874258154822833, 0.05339092507093272377 ) ) ;
#549 = ORIENTED_EDGE ( 'NONE', *, *, #6752, .T. ) ;
#550 = CARTESIAN_POINT ( 'NONE',  ( 0.05560027925352286488, -1.335209592177159843, 0.5707417262808780478 ) ) ;
#551 = AXIS2_PLACEMENT_3D ( 'NONE', #7637, #29451, #26365 ) ;
#552 = CARTESIAN_POINT ( 'NONE',  ( 0.08948292566159925243, -1.134162181311695550, 0.7575026790715814196 ) ) ;
#554 = ORIENTED_EDGE ( 'NONE', *, *, #5489, .T. ) ;
#553 = VERTEX_POINT ( 'NONE', #13801 ) ;
#555 = DIRECTION ( 'NONE',  ( -0.4999551463232372317, 0.8660512985181134660, 0.000000000000000000 ) ) ;
#556 = VERTEX_POINT ( 'NONE', #32526 ) ;
#557 = DIRECTION ( 'NONE',  ( 0.000000000000000000, 0.6595282642760673664, 0.7516797646744242112 ) ) ;
#558 = CARTESIAN_POINT ( 'NONE',  ( 0.2436109149983881617, -1.585023087768267169, -0.3520240440213115996 ) ) ;
#560 = DIRECTION ( 'NONE',  ( 0.000000000000000000, 0.000000000000000000, -1.000000000000000000 ) ) ;
#559 = CARTESIAN_POINT ( 'NONE',  ( 0.04140212552917706818, 0.4420250499596288241, 0.1614397576335226681 ) ) ;
#561 = CARTESIAN_POINT ( 'NONE',  ( -2.112273405726188513E-14, -2.097675824466503691, -0.2588528740066097233 ) ) ;
#562 = ORIENTED_EDGE ( 'NONE', *, *, #194, .F. ) ;
#563 = CARTESIAN_POINT ( 'NONE',  ( 0.008263909818985001182, -0.6872203660130532521, -0.01225013371141639093 ) ) ;
#564 = ORIENTED_EDGE ( 'NONE', *, *, #37908, .F. ) ;
#565 = CARTESIAN_POINT ( 'NONE',  ( 0.09048026637970207897, -0.6074845422973050857, 0.1898228571399218079 ) ) ;
#566 = ORIENTED_EDGE ( 'NONE', *, *, #18209, .T. ) ;
#567 = CARTESIAN_POINT ( 'NONE',  ( 0.01057740630157828245, -0.5480095452971527337, 0.4707834600657733182 ) ) ;
#568 = CARTESIAN_POINT ( 'NONE',  ( 0.4695802469098975807, -1.548054174230837576, 0.6821400120564988789 ) ) ;
#570 = CARTESIAN_POINT ( 'NONE',  ( -0.2666757540196703080, 0.4921670437878978843, 0.3599999999999995981 ) ) ;
#569 = CARTESIAN_POINT ( 'NONE',  ( 0.05836881057500214326, -0.8816445732772075772, 0.7596868123788362848 ) ) ;
#571 = CARTESIAN_POINT ( 'NONE',  ( 0.007603976726586691992, -0.8548043520540634654, 0.3312797348522363849 ) ) ;
#572 = CARTESIAN_POINT ( 'NONE',  ( 0.1428380884784982152, -0.9251932626566119477, 0.2341808872370881034 ) ) ;
#573 = UNCERTAINTY_MEASURE_WITH_UNIT (LENGTH_MEASURE( 1.000000000000000082E-05 ), #35025, 'distance_accuracy_value', 'NONE');
#574 = CARTESIAN_POINT ( 'NONE',  ( 0.3999999999999786504, -2.166079853131637201, -0.5407606602423821185 ) ) ;
#575 = CARTESIAN_POINT ( 'NONE',  ( 0.1887412855916204002, -0.4595320686313496550, 0.1406012133455269986 ) ) ;
#576 = CARTESIAN_POINT ( 'NONE',  ( 0.1264400783069879464, -0.5746782940434723708, 0.2522357024984944740 ) ) ;
#577 = CARTESIAN_POINT ( 'NONE',  ( -0.05082303569918707187, 0.2375724430107450658, 0.4097459652473644520 ) ) ;
#578 = PERSON ( 'NAUO-PER14', 'UNSPECIFIED', 'UNSPECIFIED', ('UNSPECIFIED'), ('UNSPECIFIED'), ('UNSPECIFIED') ) ;
#579 = CYLINDRICAL_SURFACE ( 'NONE', #19254, 0.01500000000000003934 ) ;
#580 = DIRECTION ( 'NONE',  ( 1.000000000000000000, 0.000000000000000000, 0.000000000000000000 ) ) ;
#581 = AXIS2_PLACEMENT_3D ( 'NONE', #9769, #38747, #35070 ) ;
#582 = ORIENTED_EDGE ( 'NONE', *, *, #14495, .T. ) ;
#583 = CARTESIAN_POINT ( 'NONE',  ( 0.1989132775362471572, -0.6135140644431382739, 0.3133236772439795259 ) ) ;
#584 = CARTESIAN_POINT ( 'NONE',  ( 0.3402959632056916650, -1.632552626064600165, -0.5940485371126216219 ) ) ;
#585 = CARTESIAN_POINT ( 'NONE',  ( 0.03820476523828830046, -1.111795898603934907, 0.6475194386861253815 ) ) ;
#586 = CARTESIAN_POINT ( 'NONE',  ( 0.05634402396114631534, 0.4396062797411924294, -0.1319984305213748876 ) ) ;
#587 = CARTESIAN_POINT ( 'NONE',  ( 0.1962011474396041510, -0.6975759447675977665, 0.3321746956187077715 ) ) ;
#588 = CARTESIAN_POINT ( 'NONE',  ( 0.2113308451705910584, -0.9022860825909653215, 0.6394510361928067432 ) ) ;
#589 = CARTESIAN_POINT ( 'NONE',  ( 0.03158843595483473710, -0.05459869295505930670, 0.4890616322892847312 ) ) ;
#590 = DIRECTION ( 'NONE',  ( -1.000000000000000000, 0.000000000000000000, 0.000000000000000000 ) ) ;
#591 = VERTEX_POINT ( 'NONE', #28693 ) ;
#592 = DIRECTION ( 'NONE',  ( -1.000000000000000000, -2.280301054154496446E-31, -1.355854680848613603E-31 ) ) ;
#593 = CARTESIAN_POINT ( 'NONE',  ( 0.3892234394240923212, -1.604307713088686027, -0.4126549618408641429 ) ) ;
#594 = DIRECTION ( 'NONE',  ( 0.000000000000000000, 0.9510565162951594154, -0.3090169943749291326 ) ) ;
#595 = CARTESIAN_POINT ( 'NONE',  ( -0.01548846960721204577, 0.07651041855109251555, 0.5222379212565261275 ) ) ;
#596 = ORIENTED_EDGE ( 'NONE', *, *, #21802, .F. ) ;
#597 = CARTESIAN_POINT ( 'NONE',  ( -0.01548846960712817709, -0.2450655194479502419, -0.4674710490748132941 ) ) ;
#598 = CARTESIAN_POINT ( 'NONE',  ( 0.1514479621444425883, -1.394758587859710852, 0.5685195609790014704 ) ) ;
#599 = CARTESIAN_POINT ( 'NONE',  ( -0.01548846960707477016, 0.4638115001430989648, -0.2459753896937820483 ) ) ;
#600 = CARTESIAN_POINT ( 'NONE',  ( 0.4002945597911881093, -1.748174800066815138, -0.4981529669132083171 ) ) ;
#601 = CARTESIAN_POINT ( 'NONE',  ( 0.4500029371338000184, -1.216587125310998552, 0.7147167669989350491 ) ) ;
#603 = CARTESIAN_POINT ( 'NONE',  ( 0.2664054812813116402, -1.675250450210487241, 0.5049835301735086102 ) ) ;
#602 = CARTESIAN_POINT ( 'NONE',  ( 0.1809966328114128442, -1.222385076516254054, -0.5155029497116575543 ) ) ;
#604 = CARTESIAN_POINT ( 'NONE',  ( 0.4929286275565831765, -1.082705722935900727, 0.5701913825460898089 ) ) ;
#605 = ORIENTED_EDGE ( 'NONE', *, *, #38870, .F. ) ;
#606 = SHAPE_DEFINITION_REPRESENTATION ( #16679, #25967 ) ;
#607 = CARTESIAN_POINT ( 'NONE',  ( 0.07366741488480997579, -1.208427444596519740, 0.7550469801918410218 ) ) ;
#608 = ORIENTED_EDGE ( 'NONE', *, *, #35307, .F. ) ;
#609 = CARTESIAN_POINT ( 'NONE',  ( 0.3400902099693209890, -1.481225204631317904, 0.8578335710567297490 ) ) ;
#611 = DIRECTION ( 'NONE',  ( 0.8660512985181135770, 0.4999551463232370652, 0.000000000000000000 ) ) ;
#610 = CARTESIAN_POINT ( 'NONE',  ( 0.08694964513190821254, -0.7344668046902962377, 0.009253963018792546111 ) ) ;
#612 = CARTESIAN_POINT ( 'NONE',  ( 0.1907332430659512135, -1.952008480481784547, -0.3293335493387484769 ) ) ;
#613 = ORIENTED_EDGE ( 'NONE', *, *, #446, .T. ) ;
#614 = B_SPLINE_CURVE_WITH_KNOTS ( 'NONE', 3,
 ( #11813, #21512, #9126, #40607, #122 ),
 .UNSPECIFIED., .F., .F.,
 ( 4, 1, 4 ),
 ( 0.003975523017580721505, 0.004090739973965705316, 0.004205956930350687392 ),
 .UNSPECIFIED. ) ;
#615 = CARTESIAN_POINT ( 'NONE',  ( -0.1172150163384020338, -0.4875187859579048211, 0.1204312767266917522 ) ) ;
#616 = CARTESIAN_POINT ( 'NONE',  ( 0.5675435908986786737, -1.503183644517305906, 0.5857270473429870838 ) ) ;
#617 = VERTEX_POINT ( 'NONE', #3589 ) ;
#618 = CARTESIAN_POINT ( 'NONE',  ( 0.3885003709713005238, -1.773188177334034110, -0.5275292682893175655 ) ) ;
#619 = CYLINDRICAL_SURFACE ( 'NONE', #2298, 0.2500000000000000000 ) ;
#620 = FACE_BOUND ( 'NONE', #11288, .T. ) ;
#621 = FACE_OUTER_BOUND ( 'NONE', #9902, .T. ) ;
#622 = PRODUCT_DEFINITION_SHAPE ( 'NONE', 'NONE',  #17711 ) ;
#623 = CARTESIAN_POINT ( 'NONE',  ( 0.6634599440086400568, -1.584707707048322867, -0.5155029497116575543 ) ) ;
#624 = CARTESIAN_POINT ( 'NONE',  ( 0.05999999999999990757, 0.6304109427692223822, -0.1442409525262416947 ) ) ;
#625 = CARTESIAN_POINT ( 'NONE',  ( 0.3868393977302779785, -1.755942212376543354, -0.5592601700348395211 ) ) ;
#626 = CARTESIAN_POINT ( 'NONE',  ( 0.5012199843439465452, -1.111650260509063681, 0.8688705274730272876 ) ) ;
#627 = DIRECTION ( 'NONE',  ( 0.8660512985181134660, 0.4999551463232371762, 0.000000000000000000 ) ) ;
#628 = EDGE_CURVE ( 'NONE', #28266, #4670, #1089, .T. ) ;
#629 = CARTESIAN_POINT ( 'NONE',  ( 0.3499317094845083576, -1.754137739073151847, 0.4513909310129906038 ) ) ;
#630 = DIRECTION ( 'NONE',  ( 1.000000000000000000, -0.000000000000000000, -0.000000000000000000 ) ) ;
#631 = DATE_AND_TIME ( #25284, #14123 ) ;
#632 = PRODUCT_RELATED_PRODUCT_CATEGORY ( 'detail', '', ( #39358 ) ) ;
#633 = CARTESIAN_POINT ( 'NONE',  ( 0.6461037703316800940, -1.403558513617581660, -0.6142287214927136807 ) ) ;
#634 = CARTESIAN_POINT ( 'NONE',  ( 0.3445792654416063305, -1.157027493435655918, 0.4460452011843933917 ) ) ;
#635 = DIRECTION ( 'NONE',  ( -0.8660512985181135770, -0.4999551463232370097, 0.000000000000000000 ) ) ;
#636 = DIRECTION ( 'NONE',  ( 1.000000000000000000, 1.138269997360102279E-15, -8.537024980200767584E-16 ) ) ;
#637 = CARTESIAN_POINT ( 'NONE',  ( 0.2520126056674420467, -1.649747432069603059, 0.6712725404530499596 ) ) ;
#638 = CARTESIAN_POINT ( 'NONE',  ( 0.0002505691696624545153, -0.4999728502647474704, -0.01895684034646696187 ) ) ;
#639 = CARTESIAN_POINT ( 'NONE',  ( 0.000000000000000000, 0.000000000000000000, 0.000000000000000000 ) ) ;
#640 = CARTESIAN_POINT ( 'NONE',  ( -0.2300000000000000100, 0.5182417262804744906, 0.3749999999999995559 ) ) ;
#641 = VERTEX_POINT ( 'NONE', #3184 ) ;
#642 = ORIENTED_EDGE ( 'NONE', *, *, #31346, .T. ) ;
#643 =( BOUNDED_SURFACE ( )  B_SPLINE_SURFACE ( 3, 2, ( 
 ( #31943, #16120, #9724 ),
 ( #35014, #9306, #18989 ),
 ( #12403, #315, #6228 ),
 ( #31522, #527, #31347 ),
 ( #22706, #35237, #15690 ),
 ( #12601, #31731, #15897 ),
 ( #37700, #3334, #13022 ),
 ( #25571, #25780, #38100 ),
 ( #34807, #7038, #6611 ),
 ( #9918, #22489, #2952 ),
 ( #15504, #16316, #22293 ),
 ( #28239, #28852, #12820 ),
 ( #24956, #712, #104 ),
 ( #40582, #21885, #34413 ) ),
 .UNSPECIFIED., .F., .F., .T. ) 
 B_SPLINE_SURFACE_WITH_KNOTS ( ( 4, 2, 2, 2, 2, 2, 4 ),
 ( 3, 3 ),
 ( 0.001271275560265211274, 0.001846161198739981746, 0.002133604017977366873, 0.002421046837214752001, 0.002708489656452137129, 0.002995932475689522256, 0.003570818114164292512 ),
 ( 0.000000000000000000, 1.000000000000000000 ),
 .UNSPECIFIED. ) 
 GEOMETRIC_REPRESENTATION_ITEM ( )  RATIONAL_B_SPLINE_SURFACE ( (
 ( 1.000000000000000000, 0.9128709291753037691, 1.000000000000000000),
 ( 1.000000000000000000, 0.9128716273348949084, 1.000000000000000000),
 ( 1.000000000000000000, 0.9128126260588453889, 1.000000000000000000),
 ( 1.000000000000000000, 0.9126599423562549163, 1.000000000000000000),
 ( 1.000000000000000000, 0.9125975471393394933, 1.000000000000000000),
 ( 1.000000000000000000, 0.9124617177696037196, 1.000000000000000000),
 ( 1.000000000000000000, 0.9123879986972855960, 1.000000000000000000),
 ( 1.000000000000000000, 0.9122366710452365357, 1.000000000000000000),
 ( 1.000000000000000000, 0.9121592624379363246, 1.000000000000000000),
 ( 1.000000000000000000, 0.9120163032376494838, 1.000000000000000000),
 ( 1.000000000000000000, 0.9119498413173655615, 1.000000000000000000),
 ( 1.000000000000000000, 0.9117793221106540447, 1.000000000000000000),
 ( 1.000000000000000000, 0.9117124009643396976, 1.000000000000000000),
 ( 1.000000000000000000, 0.9117127123830720548, 1.000000000000000000) ) ) 
 REPRESENTATION_ITEM ( '' )  SURFACE ( )  );
#644 = EDGE_CURVE ( 'NONE', #23751, #21815, #37287, .T. ) ;
#645 = CARTESIAN_POINT ( 'NONE',  ( -0.01548846960707477016, 0.4638115001430989648, -0.2459753896937820483 ) ) ;
#646 = ORIENTED_EDGE ( 'NONE', *, *, #34266, .F. ) ;
#647 = LINE ( 'NONE', #13136, #19124 ) ;
#648 = CARTESIAN_POINT ( 'NONE',  ( 0.1876053338355621880, -0.6785855078148245179, 0.1477569985384105666 ) ) ;
#649 = CARTESIAN_POINT ( 'NONE',  ( 0.4721946110347202130, -1.256212455760594038, 0.8113655170462841237 ) ) ;
#651 = ORIENTED_EDGE ( 'NONE', *, *, #25142, .T. ) ;
#650 = DIRECTION ( 'NONE',  ( 0.8660512985181135770, 0.4999551463232372317, 0.000000000000000000 ) ) ;
#652 = VERTEX_POINT ( 'NONE', #25416 ) ;
#653 = CARTESIAN_POINT ( 'NONE',  ( 0.5670603610380426929, -1.614819920947217824, 0.4627456299544086549 ) ) ;
#654 = ADVANCED_FACE ( 'NONE', ( #34847 ), #18926, .T. ) ;
#655 = EDGE_LOOP ( 'NONE', ( #20187, #33191, #212, #10371 ) ) ;
#656 = CARTESIAN_POINT ( 'NONE',  ( 0.2973196733566817462, -1.656726351290948918, 0.5753164574205285042 ) ) ;
#658 = CARTESIAN_POINT ( 'NONE',  ( 0.1120274473155025569, -0.8465630035012994270, -0.03607198864310506847 ) ) ;
#657 = LINE ( 'NONE', #28987, #16108 ) ;
#659 = LINE ( 'NONE', #6982, #22105 ) ;
#660 = CARTESIAN_POINT ( 'NONE',  ( 0.03113248654051816583, 0.000000000000000000, 0.000000000000000000 ) ) ;
#661 = EDGE_CURVE ( 'NONE', #11375, #1766, #37947, .T. ) ;
#662 = EDGE_CURVE ( 'NONE', #20865, #4083, #9046, .T. ) ;
#663 = DIRECTION ( 'NONE',  ( -1.000000000000000000, -7.857794173099924470E-32, -8.628166150854818811E-32 ) ) ;
#665 = ORIENTED_EDGE ( 'NONE', *, *, #11458, .F. ) ;
#664 = ORIENTED_EDGE ( 'NONE', *, *, #20227, .F. ) ;
#666 = ADVANCED_FACE ( 'NONE', ( #19028 ), #1210, .T. ) ;
#667 = CARTESIAN_POINT ( 'NONE',  ( 0.3211423535335589663, -1.297371328969667337, 0.4638875385414486519 ) ) ;
#668 = CARTESIAN_POINT ( 'NONE',  ( 0.2544129889468665917, -0.8811365994555702130, 0.5079734207411469304 ) ) ;
#669 = LINE ( 'NONE', #6570, #17377 ) ;
#670 = CARTESIAN_POINT ( 'NONE',  ( 0.6077710551370157921, -1.479885162639095642, 0.5931706700332087800 ) ) ;
#671 = CARTESIAN_POINT ( 'NONE',  ( 0.1556509205458345979, -0.8505966782751922528, 0.4456406740063399430 ) ) ;
#672 = CARTESIAN_POINT ( 'NONE',  ( 0.3187641638634987618, -1.760284878867080183, 0.5597302103697527897 ) ) ;
#673 = CARTESIAN_POINT ( 'NONE',  ( -0.2399999999999999079, -3.555454838273126139, -0.1971986823720165982 ) ) ;
#674 = CARTESIAN_POINT ( 'NONE',  ( 0.3409152363046951129, -1.516880185093671063, -0.7462941026102624109 ) ) ;
#675 = CARTESIAN_POINT ( 'NONE',  ( 0.6163017222665648776, -1.575337489768728449, 0.4182417262808778013 ) ) ;
#676 = EDGE_CURVE ( 'NONE', #19999, #32724, #28478, .T. ) ;
#677 = CARTESIAN_POINT ( 'NONE',  ( 0.3176952829412639789, -1.763573368804407293, 0.5240040142934835332 ) ) ;
#678 = DIRECTION ( 'NONE',  ( 0.2335885271325809920, 0.1348462688778665763, 0.9629397093077787240 ) ) ;
#679 = CARTESIAN_POINT ( 'NONE',  ( 0.05561310505367090401, -0.2871713500421218535, 0.3605322861779084453 ) ) ;
#680 = CARTESIAN_POINT ( 'NONE',  ( -0.2789010053595594729, 0.4834754829570393486, 0.3749999999999995559 ) ) ;
#681 = CARTESIAN_POINT ( 'NONE',  ( 0.1088350085164224712, -1.405274509034461161, 0.6288405113567394622 ) ) ;
#682 = COORDINATED_UNIVERSAL_TIME_OFFSET ( 0, 0, .AHEAD. ) ;
#683 = DIRECTION ( 'NONE',  ( 1.000000000000000000, 4.553079989440409115E-15, -1.138269997360102279E-15 ) ) ;
#684 = CARTESIAN_POINT ( 'NONE',  ( 0.3729107345132364748, -1.707610029665299178, -0.6887163269807711208 ) ) ;
#685 = CARTESIAN_POINT ( 'NONE',  ( -0.04230170315644025264, 0.4483301424763313503, 0.1366247710447713870 ) ) ;
#686 = CARTESIAN_POINT ( 'NONE',  ( 0.3795613398208534384, -1.760143698493221942, -0.5723197561600823491 ) ) ;
#687 = EDGE_CURVE ( 'NONE', #37027, #22774, #24185, .T. ) ;
#688 = ORIENTED_EDGE ( 'NONE', *, *, #21311, .T. ) ;
#689 = CARTESIAN_POINT ( 'NONE',  ( -0.2399999999999999079, -3.952397508731088749, -0.4603303359695052888 ) ) ;
#690 = ORIENTED_EDGE ( 'NONE', *, *, #721, .T. ) ;
#691 = CARTESIAN_POINT ( 'NONE',  ( 0.1082355115415229163, -1.414758509789771024, 0.5473920290540288391 ) ) ;
#692 = LINE ( 'NONE', #25755, #31554 ) ;
#693 = CARTESIAN_POINT ( 'NONE',  ( 0.5957873154750314981, -1.486690956665239760, 0.5986609531166485754 ) ) ;
#695 = ORIENTED_EDGE ( 'NONE', *, *, #38154, .F. ) ;
#694 = CARTESIAN_POINT ( 'NONE',  ( 0.5119721139670522225, -1.648521794865212220, -0.4427754798362790734 ) ) ;
#697 = ORIENTED_EDGE ( 'NONE', *, *, #128, .F. ) ;
#696 = ORIENTED_EDGE ( 'NONE', *, *, #15763, .F. ) ;
#698 = DIRECTION ( 'NONE',  ( 1.000000000000000000, 0.000000000000000000, 0.000000000000000000 ) ) ;
#699 = EDGE_CURVE ( 'NONE', #12256, #34558, #5748, .T. ) ;
#700 = ORIENTED_EDGE ( 'NONE', *, *, #14172, .F. ) ;
#701 = DIRECTION ( 'NONE',  ( -9.860761315262649757E-32, -0.8518913899333641071, -0.5237184928541297468 ) ) ;
#702 = CARTESIAN_POINT ( 'NONE',  ( -0.1710642718812835639, 0.4986889572247753533, 0.1481991563822706581 ) ) ;
#703 = EDGE_CURVE ( 'NONE', #23099, #24229, #34003, .T. ) ;
#704 = CARTESIAN_POINT ( 'NONE',  ( 0.002121429450436813045, -0.9534082139883235385, -0.06462206035643694446 ) ) ;
#705 = ORIENTED_EDGE ( 'NONE', *, *, #4864, .T. ) ;
#706 = ADVANCED_FACE ( 'NONE', ( #10944 ), #34677, .T. ) ;
#707 = CARTESIAN_POINT ( 'NONE',  ( 0.08602377501804453486, -0.7462434654154141978, 0.1699095607782871165 ) ) ;
#708 = CYLINDRICAL_SURFACE ( 'NONE', #23368, 0.01500000000000000291 ) ;
#709 = CARTESIAN_POINT ( 'NONE',  ( 0.5385507356656885625, -1.518881873005200722, 0.5634855329511206934 ) ) ;
#710 = ORIENTED_EDGE ( 'NONE', *, *, #5045, .F. ) ;
#711 = CARTESIAN_POINT ( 'NONE',  ( 0.6205222882181153921, -1.535344779211800015, -0.6305106974072310910 ) ) ;
#712 = CARTESIAN_POINT ( 'NONE',  ( -0.1642263572652833681, 0.5103503757440389643, 0.1470331037154066212 ) ) ;
#713 = CIRCLE ( 'NONE', #2666, 0.01000000000000002970 ) ;
#714 = CARTESIAN_POINT ( 'NONE',  ( 0.3524912763923935266, -1.753296592790281716, 0.5876423733645496084 ) ) ;
#715 = CARTESIAN_POINT ( 'NONE',  ( 0.6988690859294481861, -1.438864552056196455, 0.5752383414672479489 ) ) ;
#716 = AXIS2_PLACEMENT_3D ( 'NONE', #34831, #37505, #34436 ) ;
#717 = CARTESIAN_POINT ( 'NONE',  ( 0.5001471755736989211, -1.324671238001419171, 0.8078733825486025255 ) ) ;
#718 = DIRECTION ( 'NONE',  ( 0.7956551220374313838, 0.4593167559955297352, 0.3949190352937462234 ) ) ;
#719 = ADVANCED_FACE ( 'NONE', ( #36020 ), #10368, .F. ) ;
#720 = CARTESIAN_POINT ( 'NONE',  ( 0.05573493074139709846, -1.335442843293342063, 0.4177417262808780229 ) ) ;
#721 = EDGE_CURVE ( 'NONE', #15639, #25087, #28195, .T. ) ;
#722 = DIRECTION ( 'NONE',  ( 2.532366176626905388E-12, 0.3090169943749593862, 0.9510565162951497564 ) ) ;
#723 = CARTESIAN_POINT ( 'NONE',  ( 0.05217694232180475344, -1.283001185023028068, 0.6381678350426021051 ) ) ;
#724 = CARTESIAN_POINT ( 'NONE',  ( 0.5135987199389938640, -1.118799288056715691, 0.5631670202300380623 ) ) ;
#725 = COORDINATED_UNIVERSAL_TIME_OFFSET ( 0, 0, .AHEAD. ) ;
#726 = DIRECTION ( 'NONE',  ( -1.000000000000000000, -0.000000000000000000, -0.000000000000000000 ) ) ;
#727 = CARTESIAN_POINT ( 'NONE',  ( 0.3832962518680279596, -1.721467521351945917, 0.4207717472948147019 ) ) ;
#728 = CARTESIAN_POINT ( 'NONE',  ( 0.4470380544993052263, -1.155950011936287547, 0.4182417262808778013 ) ) ;
#729 = ORIENTED_EDGE ( 'NONE', *, *, #20999, .T. ) ;
#730 = CARTESIAN_POINT ( 'NONE',  ( 0.4676789493019616883, -1.559177855287317005, 0.5735223705611400824 ) ) ;
#731 = FACE_OUTER_BOUND ( 'NONE', #20393, .T. ) ;
#732 = CIRCLE ( 'NONE', #30256, 0.01500000000000007057 ) ;
#733 = CARTESIAN_POINT ( 'NONE',  ( -0.02000000000000000042, -2.266124458208340187, -0.5531721439363799231 ) ) ;
#734 = ORIENTED_EDGE ( 'NONE', *, *, #40360, .T. ) ;
#735 = CARTESIAN_POINT ( 'NONE',  ( 0.3207919832889619127, -1.182535135427784878, 0.4177417262808780229 ) ) ;
#736 = CARTESIAN_POINT ( 'NONE',  ( 0.6778058174389349766, -1.398346805643282620, 0.6444391890521875554 ) ) ;
#738 = ORIENTED_EDGE ( 'NONE', *, *, #38819, .T. ) ;
#737 = ORIENTED_EDGE ( 'NONE', *, *, #19321, .T. ) ;
#739 = FACE_OUTER_BOUND ( 'NONE', #35381, .T. ) ;
#740 = VECTOR ( 'NONE', #38641, 39.37007874015748143 ) ;
#741 = CARTESIAN_POINT ( 'NONE',  ( -0.01548846960721252282, 0.3688619771570396666, 0.3775276577325177296 ) ) ;
#742 = FACE_OUTER_BOUND ( 'NONE', #16658, .T. ) ;
#743 = CIRCLE ( 'NONE', #36174, 0.3698489655878002824 ) ;
#744 = ADVANCED_FACE ( 'NONE', ( #32924 ), #24766, .F. ) ;
#745 = CARTESIAN_POINT ( 'NONE',  ( 0.02881195911414546548, -0.2420394953216108425, -0.4354516087588616302 ) ) ;
#746 = ORIENTED_EDGE ( 'NONE', *, *, #7185, .F. ) ;
#747 = CARTESIAN_POINT ( 'NONE',  ( 0.5264113014007821834, -1.640729993778253126, 0.5682417262808786562 ) ) ;
#748 = CARTESIAN_POINT ( 'NONE',  ( 0.1407641140263237722, -0.7425519615811172480, 0.5154596140880725041 ) ) ;
#749 = CARTESIAN_POINT ( 'NONE',  ( 0.01618926723855275418, -0.5805349003106968775, 0.5268594266229615908 ) ) ;
#750 = CARTESIAN_POINT ( 'NONE',  ( 0.08568842022380158963, -0.5512911918770847519, 0.2017856240869609075 ) ) ;
#752 = DIRECTION ( 'NONE',  ( 0.000000000000000000, 3.330669073875470114E-16, 1.000000000000000000 ) ) ;
#751 = CARTESIAN_POINT ( 'NONE',  ( 0.4642169916328606205, -1.610048112669862030, -0.3779295768151388901 ) ) ;
#753 = CARTESIAN_POINT ( 'NONE',  ( 0.6217057667416072686, -1.470137463580756476, 0.4986251887174529829 ) ) ;
#754 = CARTESIAN_POINT ( 'NONE',  ( 0.1903653584895528827, -0.9166996592303769953, 0.2311698029113070929 ) ) ;
#755 = VERTEX_POINT ( 'NONE', #9061 ) ;
#756 = ORIENTED_EDGE ( 'NONE', *, *, #8755, .T. ) ;
#757 = DIRECTION ( 'NONE',  ( -1.000000000000000000, 1.421355798447627143E-14, -7.801168736956215639E-16 ) ) ;
#758 = B_SPLINE_CURVE_WITH_KNOTS ( 'NONE', 3,
 ( #1641, #39653, #1839, #39449, #4485, #17649, #7577, #33282, #14355, #5089, #11276, #13746, #23843, #35766, #20151, #14160, #5280, #26312 ),
 .UNSPECIFIED., .F., .F.,
 ( 4, 2, 2, 2, 2, 2, 2, 2, 4 ),
 ( -0.003133633995111071054, -0.002350221109836646283, -0.001566808224562221078, -0.0007833953392877958735, 1.754598662889739202E-08, 0.0007834304312610536683, 0.001566843316535479307, 0.002350256201809904077, 0.003133669087084328848 ),
 .UNSPECIFIED. ) ;
#759 = CARTESIAN_POINT ( 'NONE',  ( 0.1897115188215528769, -0.5340561384918134369, 0.1468274819697357736 ) ) ;
#760 = CARTESIAN_POINT ( 'NONE',  ( -0.04087116408467002249, 0.2599586249408767924, -0.3936479624527424725 ) ) ;
#761 = CARTESIAN_POINT ( 'NONE',  ( -0.1969433606228600808, 0.5138636982738217229, 0.1528658435937000626 ) ) ;
#762 = ADVANCED_FACE ( 'NONE', ( #3496 ), #29429, .T. ) ;
#763 = B_SPLINE_CURVE_WITH_KNOTS ( 'NONE', 3,
 ( #13876, #38772, #7720, #17729, #29528, #2111, #13502 ),
 .UNSPECIFIED., .F., .F.,
 ( 4, 3, 4 ),
 ( -6.000000000366142690E-08, 1.760240343512842892E-21, 0.0002642484537205252570 ),
 .UNSPECIFIED. ) ;
#764 = AXIS2_PLACEMENT_3D ( 'NONE', #30199, #23459, #26922 ) ;
#765 = DIRECTION ( 'NONE',  ( -0.8660512985181134660, -0.4999551463232372872, 0.000000000000000000 ) ) ;
#766 = EDGE_CURVE ( 'NONE', #30726, #17298, #14950, .T. ) ;
#767 = CARTESIAN_POINT ( 'NONE',  ( 0.2674444507101633728, -0.7485333398656358606, 0.5795413912256205391 ) ) ;
#768 = VECTOR ( 'NONE', #1242, 39.37007874015748143 ) ;
#769 = EDGE_CURVE ( 'NONE', #31675, #29116, #15627, .T. ) ;
#770 = CARTESIAN_POINT ( 'NONE',  ( 0.5313858342244102140, -1.164972183933710825, 0.5039547296423043665 ) ) ;
#771 = CARTESIAN_POINT ( 'NONE',  ( 0.04540579952787707901, -1.158556396592530513, 0.6631049105669120092 ) ) ;
#772 = CONICAL_SURFACE ( 'NONE', #33580, 0.04999999999999994726, 1.047197551196598964 ) ;
#773 = CARTESIAN_POINT ( 'NONE',  ( -2.070754768975509919, -0.09959325338431655739, 0.1178658435937004478 ) ) ;
#774 = CYLINDRICAL_SURFACE ( 'NONE', #27850, 0.1000000000000000194 ) ;
#775 = CARTESIAN_POINT ( 'NONE',  ( 0.2569662571990922184, -0.9629747482851543916, 0.6869665874150546747 ) ) ;
#776 = CARTESIAN_POINT ( 'NONE',  ( 0.000000000000000000, 0.08637707520836798714, 0.000000000000000000 ) ) ;
#777 = CARTESIAN_POINT ( 'NONE',  ( 0.6940617502335346689, -1.499911880483144166, 0.4737457937229823668 ) ) ;
#778 = ORIENTED_EDGE ( 'NONE', *, *, #15008, .T. ) ;
#779 = CYLINDRICAL_SURFACE ( 'NONE', #8863, 0.2500000000000000000 ) ;
#780 = CARTESIAN_POINT ( 'NONE',  ( 0.5265030742546764619, -1.341057478605462316, 0.7770388537806591778 ) ) ;
#781 = CARTESIAN_POINT ( 'NONE',  ( 0.5435064000818763397, -1.629330203429091739, -0.4449807330069644462 ) ) ;
#782 = DIRECTION ( 'NONE',  ( 1.000000000000000000, -0.000000000000000000, -0.000000000000000000 ) ) ;
#783 = VECTOR ( 'NONE', #35125, 39.37007874015748143 ) ;
#784 = ORIENTED_EDGE ( 'NONE', *, *, #14738, .F. ) ;
#785 = CARTESIAN_POINT ( 'NONE',  ( -0.02235124290213240730, -0.3550643254722131714, -0.3695962758878534316 ) ) ;
#786 = CARTESIAN_POINT ( 'NONE',  ( 0.1891450095147329813, -0.5717505337550861100, 0.2886938745194108646 ) ) ;
#787 = DIRECTION ( 'NONE',  ( 1.000000000000000000, 0.000000000000000000, 0.000000000000000000 ) ) ;
#788 = CARTESIAN_POINT ( 'NONE',  ( 0.1859432605888821921, -0.7573098151843028480, 0.1022962920937455361 ) ) ;
#789 = CARTESIAN_POINT ( 'NONE',  ( 0.4906812380651594530, -1.277603856553843897, 0.5875273083986286560 ) ) ;
#790 = CIRCLE ( 'NONE', #27688, 0.2200000000000000844 ) ;
#791 = EDGE_CURVE ( 'NONE', #21815, #617, #38610, .T. ) ;
#793 = CARTESIAN_POINT ( 'NONE',  ( -0.02000000000000000042, -2.177105168660885326, -0.3918349584362407212 ) ) ;
#792 = PLANE ( 'NONE',  #28543 ) ;
#794 = CARTESIAN_POINT ( 'NONE',  ( 0.3384799338905536970, -0.9979650346196410338, 0.5984318192120324786 ) ) ;
#795 = ORIENTED_EDGE ( 'NONE', *, *, #11536, .F. ) ;
#796 = CIRCLE ( 'NONE', #23764, 0.1000000000000000194 ) ;
#797 = CARTESIAN_POINT ( 'NONE',  ( -0.1731185243557762099, 0.5373335498847187086, 0.3599999999999999867 ) ) ;
#798 = ORIENTED_EDGE ( 'NONE', *, *, #21242, .F. ) ;
#799 = VERTEX_POINT ( 'NONE', #28189 ) ;
#800 = CARTESIAN_POINT ( 'NONE',  ( 0.1226422125323946705, -0.8479982503710601360, 0.6959758587416453590 ) ) ;
#801 = CARTESIAN_POINT ( 'NONE',  ( 0.06475727327243140097, -0.8283951214762328430, 0.1002009769046496579 ) ) ;
#802 = DIRECTION ( 'NONE',  ( 8.326672684688655318E-16, -2.361472542561083598E-16, 1.000000000000000000 ) ) ;
#803 = ORIENTED_EDGE ( 'NONE', *, *, #30064, .T. ) ;
#804 = AXIS2_PLACEMENT_3D ( 'NONE', #15978, #21964, #31217 ) ;
#805 = CARTESIAN_POINT ( 'NONE',  ( 0.1399999999999994582, 1.942890293094021357E-17, 0.05000000000000000971 ) ) ;
#806 = CARTESIAN_POINT ( 'NONE',  ( 0.5662983945365519522, -1.503052247576714961, 0.5610676162927376032 ) ) ;
#807 = ORIENTED_EDGE ( 'NONE', *, *, #4372, .T. ) ;
#808 = CARTESIAN_POINT ( 'NONE',  ( 0.3916693287292108416, -1.957780039576698217, -0.4986156861099343418 ) ) ;
#809 = CARTESIAN_POINT ( 'NONE',  ( -0.004906298587631805104, -2.107936428766274073, -0.2870436526301869407 ) ) ;
#810 = CARTESIAN_POINT ( 'NONE',  ( 0.3219636445852379070, -1.527820583036367141, -0.7368875844864777314 ) ) ;
#811 = DIRECTION ( 'NONE',  ( 0.4999551463232373427, -0.8660512985181134660, 0.000000000000000000 ) ) ;
#812 = CARTESIAN_POINT ( 'NONE',  ( -2.112273405726188513E-14, -1.835409001655643690, -0.3543101909453316156 ) ) ;
#813 = CARTESIAN_POINT ( 'NONE',  ( 0.1169788285577439829, -1.415237608940837388, 0.5049415650359101448 ) ) ;
#814 = LINE ( 'NONE', #16615, #246 ) ;
#815 = CARTESIAN_POINT ( 'NONE',  ( 0.05999999999999990757, 0.5878163732725504298, -0.1704268771689479434 ) ) ;
#816 = DIRECTION ( 'NONE',  ( 0.000000000000000000, 0.3420201433256706003, -0.9396926207859077618 ) ) ;
#817 = DIRECTION ( 'NONE',  ( 0.000000000000000000, 0.000000000000000000, -1.000000000000000000 ) ) ;
#818 = PERSON_AND_ORGANIZATION_ROLE ( 'design_supplier' ) ;
#819 = AXIS2_PLACEMENT_3D ( 'NONE', #17406, #29967, #8743 ) ;
#820 = EDGE_CURVE ( 'NONE', #1211, #35870, #12969, .T. ) ;
#821 = CARTESIAN_POINT ( 'NONE',  ( 0.6491414849553497346, -1.426744591349599967, -0.6169505267336127252 ) ) ;
#822 = DIRECTION ( 'NONE',  ( -0.9378410757839559242, 0.2807814858886551468, -0.2039996905746456479 ) ) ;
#823 = CARTESIAN_POINT ( 'NONE',  ( 0.1841393808565141010, -0.5721394145837870315, 0.006895157961417135856 ) ) ;
#824 = CARTESIAN_POINT ( 'NONE',  ( 0.4103533436992015671, -1.245885857446504374, 0.5182417262812503145 ) ) ;
#825 = FACE_OUTER_BOUND ( 'NONE', #10244, .T. ) ;
#826 = AXIS2_PLACEMENT_3D ( 'NONE', #29812, #40436, #14173 ) ;
#827 = VECTOR ( 'NONE', #40287, 39.37007874015748143 ) ;
#828 = CARTESIAN_POINT ( 'NONE',  ( 0.003142067210302413628, -0.5716151664902620055, 0.1991251360516817781 ) ) ;
#829 = CARTESIAN_POINT ( 'NONE',  ( 0.5915319031500693159, -1.513102603207748365, -0.3972843660575071101 ) ) ;
#830 = CIRCLE ( 'NONE', #10656, 0.01500000000000000291 ) ;
#831 = CARTESIAN_POINT ( 'NONE',  ( -0.08978098643734171158, 0.000000000000000000, 0.000000000000000000 ) ) ;
#832 = CARTESIAN_POINT ( 'NONE',  ( 0.04582713223189451707, -0.2312054150958140764, 0.4285473768184998589 ) ) ;
#833 = CARTESIAN_POINT ( 'NONE',  ( 0.2059273467974226945, -1.283046334493782803, -0.2869361388274795921 ) ) ;
#834 = EDGE_LOOP ( 'NONE', ( #36795, #19771, #24755, #38611 ) ) ;
#835 = B_SPLINE_CURVE_WITH_KNOTS ( 'NONE', 3,
 ( #23386, #4599, #19860, #4219, #29333, #11019, #38762, #1179, #10594, #17174 ),
 .UNSPECIFIED., .F., .F.,
 ( 4, 2, 2, 2, 4 ),
 ( 4.793059745592843663E-05, 0.001006021979757477577, 0.001964113362059026827, 0.002922204744360576076, 0.003880296126662125325 ),
 .UNSPECIFIED. ) ;
#837 = ORIENTED_EDGE ( 'NONE', *, *, #8785, .F. ) ;
#836 = B_SPLINE_SURFACE_WITH_KNOTS ( 'NONE', 5, 5, ( 
 ( #31533, #22111, #19202, #720, #25171, #326 ),
 ( #12829, #25391, #16517, #536, #13032, #13220 ),
 ( #7045, #37492, #21896, #16324, #34422, #22714 ),
 ( #38111, #6237, #38311, #31744, #9930, #35246 ),
 ( #19614, #37922, #37709, #9533, #4755, #29277 ),
 ( #1514, #35847, #20228, #38720, #10541, #32549 ) ),
 .UNSPECIFIED., .F., .F., .F.,
 ( 6, 6 ),
 ( 6, 6 ),
 ( -6.477000000001651436, 6.477000000001639002 ),
 ( -2.080605796196421498, 4.396394203803585476 ),
 .UNSPECIFIED. ) ;
#838 = CARTESIAN_POINT ( 'NONE',  ( 0.05561176441985724722, -0.2871508736821620222, -0.3605511861568529430 ) ) ;
#839 = VERTEX_POINT ( 'NONE', #28601 ) ;
#840 = DIRECTION ( 'NONE',  ( 1.000000000000000000, 2.403560570595279103E-31, -1.725633230170969455E-31 ) ) ;
#841 = CARTESIAN_POINT ( 'NONE',  ( 0.5797229963041876655, -1.607661183008572969, -0.4675097618473461059 ) ) ;
#842 = CARTESIAN_POINT ( 'NONE',  ( 0.4354831391633621207, -1.199087596169247094, 0.7698817195160777560 ) ) ;
#844 = ORIENTED_EDGE ( 'NONE', *, *, #14510, .F. ) ;
#843 = DIRECTION ( 'NONE',  ( 1.000000000000000000, 0.000000000000000000, 0.000000000000000000 ) ) ;
#845 = CARTESIAN_POINT ( 'NONE',  ( 0.5544279432241370209, -1.187676084274785548, 0.5985052393047670671 ) ) ;
#846 = DIRECTION ( 'NONE',  ( 1.000000000000000000, 0.000000000000000000, 0.000000000000000000 ) ) ;
#847 = ORIENTED_EDGE ( 'NONE', *, *, #8033, .T. ) ;
#848 = DIRECTION ( 'NONE',  ( -0.1280454979611833077, 0.000000000000000000, 0.9917682947401941229 ) ) ;
#849 = VERTEX_POINT ( 'NONE', #9460 ) ;
#850 = CARTESIAN_POINT ( 'NONE',  ( 0.2997655131913015136, -1.638171704166688558, 0.7345980899167104949 ) ) ;
#852 = CARTESIAN_POINT ( 'NONE',  ( -0.01548846960721259221, -0.2450655194478906784, 0.4674710490746316616 ) ) ;
#851 = CARTESIAN_POINT ( 'NONE',  ( -0.2399999999999999079, -2.183180860297908144, -0.4937760292030871079 ) ) ;
#853 = DIRECTION ( 'NONE',  ( -8.881784197001246407E-16, 2.361472542561082612E-16, -1.000000000000000000 ) ) ;
#854 = CARTESIAN_POINT ( 'NONE',  ( 0.1867780286631144093, -0.7337134285967986669, -0.08446770797961487831 ) ) ;
#855 = VECTOR ( 'NONE', #26540, 39.37007874015748143 ) ;
#856 = CARTESIAN_POINT ( 'NONE',  ( 0.07288795999653738256, -1.414255277265392907, -0.3388138788922953060 ) ) ;
#858 = VERTEX_POINT ( 'NONE', #6373 ) ;
#857 = ORIENTED_EDGE ( 'NONE', *, *, #27787, .T. ) ;
#859 = DIRECTION ( 'NONE',  ( 0.000000000000000000, 0.000000000000000000, -1.000000000000000000 ) ) ;
#860 = CARTESIAN_POINT ( 'NONE',  ( 0.1109053458322742519, -0.9286334977625223530, 0.1468672030441772469 ) ) ;
#861 = CARTESIAN_POINT ( 'NONE',  ( -0.02869712619511922275, -0.06034133159975870603, -0.4947855140619938918 ) ) ;
#862 = CARTESIAN_POINT ( 'NONE',  ( 0.5864976212241491682, -1.491712091267360263, 0.6107045218380184881 ) ) ;
#863 = VECTOR ( 'NONE', #31648, 39.37007874015748143 ) ;
#864 = AXIS2_PLACEMENT_3D ( 'NONE', #285, #6192, #12993 ) ;
#865 = CARTESIAN_POINT ( 'NONE',  ( 0.4248423436954585908, -1.212122267013820753, 0.6558017523709199770 ) ) ;
#866 = CARTESIAN_POINT ( 'NONE',  ( 0.01056671636551369080, -0.5306646670528684107, 0.1647702481118153983 ) ) ;
#867 = AXIS2_PLACEMENT_3D ( 'NONE', #16303, #28430, #10117 ) ;
#868 = FACE_OUTER_BOUND ( 'NONE', #23037, .T. ) ;
#869 = CARTESIAN_POINT ( 'NONE',  ( -0.1683849832494448140, 0.4901165368553581092, 0.3263506530378934012 ) ) ;
#870 = DIRECTION ( 'NONE',  ( 1.000000000000000000, 0.000000000000000000, 0.000000000000000000 ) ) ;
#871 = CARTESIAN_POINT ( 'NONE',  ( 0.01548846960707528191, -0.09061086148585918709, 0.5171215251570857596 ) ) ;
#872 = CARTESIAN_POINT ( 'NONE',  ( 0.4333792208851959815, -1.117102659751931792, -0.6448351790779591752 ) ) ;
#873 = PERSON_AND_ORGANIZATION_ROLE ( 'creator' ) ;
#874 = CARTESIAN_POINT ( 'NONE',  ( 0.04229974373173746999, -0.2684538943183488180, 0.3841910309322000838 ) ) ;
#875 = EDGE_CURVE ( 'NONE', #7023, #10339, #36997, .T. ) ;
#876 = EDGE_CURVE ( 'NONE', #33794, #23035, #20325, .T. ) ;
#877 = CARTESIAN_POINT ( 'NONE',  ( 0.1788174026987448817, -0.4928320601422241931, 0.1325682524468290158 ) ) ;
#878 = DIRECTION ( 'NONE',  ( 1.386669559958804888E-32, 0.8983234858819696411, 0.4393346272636231564 ) ) ;
#879 = EDGE_CURVE ( 'NONE', #19095, #17240, #22904, .T. ) ;
#880 = LINE ( 'NONE', #19969, #39598 ) ;
#881 = CARTESIAN_POINT ( 'NONE',  ( 0.1741751201940545390, -1.802433987137200599, -0.6515250642801660996 ) ) ;
#882 = ADVANCED_FACE ( 'NONE', ( #3705 ), #35378, .F. ) ;
#883 = AXIS2_PLACEMENT_3D ( 'NONE', #24131, #20412, #8048 ) ;
#884 = CARTESIAN_POINT ( 'NONE',  ( -0.02872242845530577349, 0.5252126300208015408, 0.08844866507292889479 ) ) ;
#885 = DIRECTION ( 'NONE',  ( -1.000000000000000000, -2.276539994720197063E-15, 0.000000000000000000 ) ) ;
#886 = B_SPLINE_CURVE_WITH_KNOTS ( 'NONE', 3,
 ( #29139, #8133, #1587, #11038, #14314, #7524, #10418, #35498, #20708, #13892, #33240, #14111, #16809, #20102, #39002, #7305, #32818, #7733, #17197, #13699, #10834, #35926, #4833, #26266, #4439, #16999 ),
 .UNSPECIFIED., .F., .F.,
 ( 4, 2, 2, 2, 2, 2, 2, 2, 2, 2, 2, 2, 4 ),
 ( 0.000000000000000000, 0.0006636363572759321466, 0.001327272714551864293, 0.001659090893189832426, 0.001990909071827800560, 0.002322727250465768476, 0.002654545429103736826, 0.003318181786379673093, 0.003649999965017641009, 0.003981818143655608058, 0.004313636322293576408, 0.004645454500931543891, 0.005309090858207477122 ),
 .UNSPECIFIED. ) ;
#887 = EDGE_CURVE ( 'NONE', #19917, #25255, #28631, .T. ) ;
#888 = AXIS2_PLACEMENT_3D ( 'NONE', #11720, #40510, #18097 ) ;
#889 = AXIS2_PLACEMENT_3D ( 'NONE', #14092, #32801, #28026 ) ;
#890 = VERTEX_POINT ( 'NONE', #1064 ) ;
#891 = CARTESIAN_POINT ( 'NONE',  ( 0.1905436384893607615, -0.5945559727383887827, 0.3046096357648226949 ) ) ;
#892 = VERTEX_POINT ( 'NONE', #10676 ) ;
#893 = DIRECTION ( 'NONE',  ( 1.000000000000000000, 0.000000000000000000, 0.000000000000000000 ) ) ;
#894 = DIRECTION ( 'NONE',  ( 1.000000000000000000, 1.707404996040165152E-15, 0.000000000000000000 ) ) ;
#895 = AXIS2_PLACEMENT_3D ( 'NONE', #6787, #28205, #31908 ) ;
#896 = CARTESIAN_POINT ( 'NONE',  ( 0.1315527212125843504, -0.5529222810202329974, 0.1699692310456895061 ) ) ;
#898 = ORIENTED_EDGE ( 'NONE', *, *, #29268, .T. ) ;
#897 = CARTESIAN_POINT ( 'NONE',  ( -0.05464101615137773038, -2.698373762442814350, -0.2370085142459261718 ) ) ;
#900 = ORIENTED_EDGE ( 'NONE', *, *, #32662, .T. ) ;
#899 = ORIENTED_EDGE ( 'NONE', *, *, #34731, .T. ) ;
#901 = DIRECTION ( 'NONE',  ( -0.8660512985181135770, -0.4999551463232370652, 0.000000000000000000 ) ) ;
#902 = EDGE_LOOP ( 'NONE', ( #39014, #5058, #6053, #24549 ) ) ;
#903 = CIRCLE ( 'NONE', #4766, 0.02999999999999999195 ) ;
#904 = EDGE_CURVE ( 'NONE', #20709, #39668, #32268, .T. ) ;
#905 = CARTESIAN_POINT ( 'NONE',  ( 0.3757471142192211344, -1.766731021160330428, -0.5680748514784754732 ) ) ;
#906 = APPROVAL ( #38025, 'UNSPECIFIED' ) ;
#907 = CARTESIAN_POINT ( 'NONE',  ( 0.6273212425683272198, -1.617116560674602521, -0.5218031926565810386 ) ) ;
#908 = COORDINATED_UNIVERSAL_TIME_OFFSET ( 0, 0, .AHEAD. ) ;
#909 = DIRECTION ( 'NONE',  ( -4.930380657631323784E-32, -0.7472307839325098566, -0.6645646360916346307 ) ) ;
#910 = ORIENTED_EDGE ( 'NONE', *, *, #11433, .T. ) ;
#911 = CARTESIAN_POINT ( 'NONE',  ( 0.1954888443903809170, -0.9019706710010376716, 0.6101278593650538706 ) ) ;
#912 = CARTESIAN_POINT ( 'NONE',  ( 0.06924657340765723312, -0.5400045880099078044, 0.1460913089649399643 ) ) ;
#913 = CARTESIAN_POINT ( 'NONE',  ( 0.5403952185064613278, -1.517255356709687808, 0.6224652973508716380 ) ) ;
#914 = DIRECTION ( 'NONE',  ( 1.445848444424219201E-15, -1.000000000000000000, -2.361472542561095431E-16 ) ) ;
#915 = CARTESIAN_POINT ( 'NONE',  ( -0.02000000000000000042, -2.626773565144302935, -0.2526934094652523721 ) ) ;
#916 = CARTESIAN_POINT ( 'NONE',  ( 0.6987898065016509008, -1.520117587203002607, 0.5151143090318311968 ) ) ;
#917 = AXIS2_PLACEMENT_3D ( 'NONE', #1456, #13588, #13971 ) ;
#918 = CARTESIAN_POINT ( 'NONE',  ( 0.3061809949057166524, -1.759155323846213204, 0.5693298920811382668 ) ) ;
#919 = CARTESIAN_POINT ( 'NONE',  ( 0.2927350798622619377, -1.544518291098220697, -0.6925464747855744063 ) ) ;
#920 = CARTESIAN_POINT ( 'NONE',  ( 0.4284865639878338017, -1.682583770571502990, 0.4182417262808776903 ) ) ;
#921 = B_SPLINE_CURVE_WITH_KNOTS ( 'NONE', 3,
 ( #12992, #9882, #6791, #3728, #35998, #1865, #32499, #7606, #4323, #23667, #23271, #10493, #23877, #14379, #30040, #13777, #10914, #19964, #8006, #26157, #20374, #26341, #4512, #16886, #32705, #38675, #26945, #30219, #2051, #23060, #39477, #36401, #11308, #1674, #36192, #10701, #29427, #35590, #8216, #1465 ),
 .UNSPECIFIED., .F., .F.,
 ( 4, 2, 2, 2, 2, 2, 2, 2, 2, 2, 2, 2, 2, 2, 2, 2, 2, 2, 2, 4 ),
 ( 0.000000000000000000, 0.002694941689597518588, 0.005389883379195037176, 0.008084825068792557065, 0.009432295913591315709, 0.01077976675839007435, 0.01212723760318883647, 0.01347470844798758990, 0.01414844387038696923, 0.01482217929278635028, 0.01549591471518572787, 0.01616965013758510719, 0.01684338555998448825, 0.01751712098238386930, 0.01886459182718262795, 0.02021206267198139006, 0.02088579809438077459, 0.02122266580558046858, 0.02139109966118031905, 0.02155953351678016952 ),
 .UNSPECIFIED. ) ;
#922 = VECTOR ( 'NONE', #37613, 39.37007874015748143 ) ;
#923 = CARTESIAN_POINT ( 'NONE',  ( 0.3158858043796832216, -1.003067975662501832, 0.7589385492876046246 ) ) ;
#924 = CARTESIAN_POINT ( 'NONE',  ( -3.231615316776240918E-05, -0.7201627993511090509, -0.1017344997239397197 ) ) ;
#925 =( CONVERSION_BASED_UNIT ( 'INCH', #9929 ) LENGTH_UNIT ( ) NAMED_UNIT ( #28861 ) );
#926 = CARTESIAN_POINT ( 'NONE',  ( 0.006276500232904156859, -0.8404987286125837898, 0.1047677167647131508 ) ) ;
#927 = CARTESIAN_POINT ( 'NONE',  ( 0.01548846960721238578, -0.4730347584884322942, -0.2341461249027902980 ) ) ;
#928 = CARTESIAN_POINT ( 'NONE',  ( -0.002023118427450016753, -0.8974731051190899533, 0.1948784381876195460 ) ) ;
#929 = CARTESIAN_POINT ( 'NONE',  ( 0.3302065591133839240, -0.9317669992161012882, 0.6252562391197076241 ) ) ;
#930 = EDGE_CURVE ( 'NONE', #7674, #5500, #39914, .T. ) ;
#931 = COORDINATED_UNIVERSAL_TIME_OFFSET ( 0, 0, .AHEAD. ) ;
#932 = CARTESIAN_POINT ( 'NONE',  ( 0.3740960844805631957, -1.108072201694596526, 0.5182417262812423209 ) ) ;
#933 = EDGE_CURVE ( 'NONE', #13311, #30248, #7555, .T. ) ;
#934 = CARTESIAN_POINT ( 'NONE',  ( 0.1835961851041346959, -0.5126270562563732813, 0.08826789480522242992 ) ) ;
#935 = ADVANCED_FACE ( 'NONE', ( #4687 ), #15006, .T. ) ;
#936 = CARTESIAN_POINT ( 'NONE',  ( 0.4861084675450336734, -1.181744968368830584, 0.4182417262808778569 ) ) ;
#937 = ORIENTED_EDGE ( 'NONE', *, *, #32050, .F. ) ;
#938 = CARTESIAN_POINT ( 'NONE',  ( -0.2399999999999999079, -3.893469231891077520, -0.3535776419057993225 ) ) ;
#939 = CARTESIAN_POINT ( 'NONE',  ( 0.01055999354153808190, -0.5296565605740091165, 0.1443450864220710561 ) ) ;
#940 = AXIS2_PLACEMENT_3D ( 'NONE', #30986, #31207, #2810 ) ;
#941 = CARTESIAN_POINT ( 'NONE',  ( 0.08738337528432148227, -0.6948978725876520102, 0.02266917563589926354 ) ) ;
#942 = ORIENTED_EDGE ( 'NONE', *, *, #39899, .F. ) ;
#943 = DIRECTION ( 'NONE',  ( 0.000000000000000000, 0.000000000000000000, -1.000000000000000000 ) ) ;
#944 = CARTESIAN_POINT ( 'NONE',  ( 0.4504239474101026652, -1.039103266886249655, 0.7909361398939754872 ) ) ;
#946 = ORIENTED_EDGE ( 'NONE', *, *, #10762, .T. ) ;
#945 = ORIENTED_EDGE ( 'NONE', *, *, #20570, .T. ) ;
#947 = DIRECTION ( 'NONE',  ( -1.000000000000000000, 0.000000000000000000, 0.000000000000000000 ) ) ;
#948 = ORIENTED_EDGE ( 'NONE', *, *, #21075, .T. ) ;
#949 = CARTESIAN_POINT ( 'NONE',  ( -0.2746410161513776482, -3.791721498889941255, -0.2726869407194119077 ) ) ;
#950 = EDGE_CURVE ( 'NONE', #27945, #16911, #15654, .T. ) ;
#951 = PRODUCT_DEFINITION_SHAPE ( 'NONE', 'NONE',  #8373 ) ;
#952 = CARTESIAN_POINT ( 'NONE',  ( 0.3817983344580043181, -1.702428809890406125, -0.3364609660280786785 ) ) ;
#953 = CARTESIAN_POINT ( 'NONE',  ( -0.03174036153403859972, 0.5170813853140294736, -0.08825077997795674478 ) ) ;
#954 = ORIENTED_EDGE ( 'NONE', *, *, #21625, .F. ) ;
#955 = CARTESIAN_POINT ( 'NONE',  ( 0.04687500000000000694, -0.4345172148286636782, 0.1921395889696510262 ) ) ;
#956 = CARTESIAN_POINT ( 'NONE',  ( 0.09733160485405090157, -0.6654810868242956312, 0.3090395299204725110 ) ) ;
#957 = AXIS2_PLACEMENT_3D ( 'NONE', #14940, #29606, #7592 ) ;
#958 = CARTESIAN_POINT ( 'NONE',  ( -0.02000000000000000042, -1.699711333021935777, -0.9366211149475224262 ) ) ;
#959 = CARTESIAN_POINT ( 'NONE',  ( 0.4692883835019161509, -1.557836661473111395, 0.5661479686463081196 ) ) ;
#960 = AXIS2_PLACEMENT_3D ( 'NONE', #23321, #29667, #23920 ) ;
#962 = CARTESIAN_POINT ( 'NONE',  ( -0.2267371898560526788, -0.4872893062166341327, 0.09999999999999975575 ) ) ;
#961 = CARTESIAN_POINT ( 'NONE',  ( 0.08034914622429441267, -0.9725984063009643910, 0.8263393459352617043 ) ) ;
#963 = CARTESIAN_POINT ( 'NONE',  ( 0.1967796840110664081, -0.9202189791215042991, 0.2910963043859624566 ) ) ;
#964 = ORIENTED_EDGE ( 'NONE', *, *, #36877, .T. ) ;
#965 = DIRECTION ( 'NONE',  ( -0.4999551463232373427, 0.8660512985181134660, -0.000000000000000000 ) ) ;
#966 = CARTESIAN_POINT ( 'NONE',  ( 0.1961146565040154666, -0.5779037128980665239, 0.3019974763434182807 ) ) ;
#967 = CARTESIAN_POINT ( 'NONE',  ( -0.03877220711930364633, 0.2524486846094415871, -0.4039751870151973567 ) ) ;
#968 = CARTESIAN_POINT ( 'NONE',  ( -0.2746410161513779258, -3.647187793141847045, -0.4766722536777797115 ) ) ;
#969 = CARTESIAN_POINT ( 'NONE',  ( 0.4634712904840416758, -1.711704060178988129, -0.5155029497116575543 ) ) ;
#970 = CARTESIAN_POINT ( 'NONE',  ( 0.6742391038958878147, -1.391540648348956966, 0.6661449684938977045 ) ) ;
#971 = CIRCLE ( 'NONE', #8802, 0.1033070866141734129 ) ;
#972 = ADVANCED_FACE ( 'NONE', ( #11697 ), #23462, .T. ) ;
#973 = TOROIDAL_SURFACE ( 'NONE', #21338, 0.05000000000000000971, 0.2000000000000000111 ) ;
#974 = CARTESIAN_POINT ( 'NONE',  ( -0.2399999999999999079, -3.899630010830198668, -0.3430483616844877681 ) ) ;
#975 = EDGE_CURVE ( 'NONE', #4341, #5197, #7083, .T. ) ;
#976 = CARTESIAN_POINT ( 'NONE',  ( 0.03875523708677772183, 0.4416911308383487667, -0.1785246905291516251 ) ) ;
#977 = CARTESIAN_POINT ( 'NONE',  ( 0.4872883505774054380, -1.680912827369504425, -0.6127499270552401178 ) ) ;
#978 = EDGE_LOOP ( 'NONE', ( #32766, #807, #4569, #16901 ) ) ;
#979 = CARTESIAN_POINT ( 'NONE',  ( 0.2640953184584151625, -0.9556158622373929212, 0.7086077991120209862 ) ) ;
#980 = DIRECTION ( 'NONE',  ( -1.000000000000000000, -2.280301054154495132E-31, 1.664003471950577689E-31 ) ) ;
#981 = AXIS2_PLACEMENT_3D ( 'NONE', #34205, #18797, #21888 ) ;
#982 = FACE_OUTER_BOUND ( 'NONE', #34433, .T. ) ;
#983 = AXIS2_PLACEMENT_3D ( 'NONE', #32286, #10909, #29616 ) ;
#984 = ORIENTED_EDGE ( 'NONE', *, *, #9908, .F. ) ;
#985 = DIRECTION ( 'NONE',  ( -0.4999551463232371762, 0.8660512985181134660, -0.000000000000000000 ) ) ;
#986 = PLANE ( 'NONE',  #27207 ) ;
#987 = CARTESIAN_POINT ( 'NONE',  ( 0.3051773648903314817, -1.756515850768020304, 0.5493070528972983091 ) ) ;
#988 = CARTESIAN_POINT ( 'NONE',  ( -0.03650577977170611083, -0.08362514765351501678, 0.5048437183011775797 ) ) ;
#989 = CARTESIAN_POINT ( 'NONE',  ( 0.06595730239831418262, -0.8537221610436072083, 0.3900050273732788564 ) ) ;
#990 = VERTEX_POINT ( 'NONE', #22805 ) ;
#991 = CARTESIAN_POINT ( 'NONE',  ( -0.1552056223146404124, 0.4812861443614839807, 0.3591723288241695511 ) ) ;
#992 = ADVANCED_FACE ( 'NONE', ( #34911 ), #9813, .T. ) ;
#993 = DIRECTION ( 'NONE',  ( 1.000000000000000000, 2.341930812374887555E-31, -1.664003471950578127E-31 ) ) ;
#994 = LINE ( 'NONE', #10008, #35547 ) ;
#995 = EDGE_CURVE ( 'NONE', #29245, #13061, #28783, .T. ) ;
#996 = CARTESIAN_POINT ( 'NONE',  ( -2.115421433687637455E-14, -2.107936428766274073, -0.7005084057759867200 ) ) ;
#997 = CIRCLE ( 'NONE', #26580, 0.5302738246768102792 ) ;
#998 = CARTESIAN_POINT ( 'NONE',  ( 0.4104893297753217096, -1.161006097983400709, 0.7058587609593679479 ) ) ;
#1000 = CARTESIAN_POINT ( 'NONE',  ( 0.05999999999999990757, 0.8066736284972624293, -0.2400112280131874720 ) ) ;
#999 = LINE ( 'NONE', #9610, #37082 ) ;
#1001 = CARTESIAN_POINT ( 'NONE',  ( 0.1875000000000002498, -0.9151275355372966436, 0.1457185332388701016 ) ) ;
#1002 = EDGE_LOOP ( 'NONE', ( #38695, #33633, #31555, #292 ) ) ;
#1003 = ADVANCED_FACE ( 'NONE', ( #28935 ), #31589, .T. ) ;
#1005 = CIRCLE ( 'NONE', #38392, 0.1600000000000016964 ) ;
#1004 = CALENDAR_DATE ( 2026, 13, 10 ) ;
#1006 = CARTESIAN_POINT ( 'NONE',  ( 0.3784855106043947814, -1.091058466892998347, -0.5155029497116575543 ) ) ;
#1007 = ORIENTED_EDGE ( 'NONE', *, *, #36131, .T. ) ;
#1008 = CIRCLE ( 'NONE', #33149, 0.1699999999999999012 ) ;
#1009 = AXIS2_PLACEMENT_3D ( 'NONE', #23689, #17303, #8240 ) ;
#1010 = CARTESIAN_POINT ( 'NONE',  ( 0.3934995777983899545, -1.530652811628217425, 0.7930223495936653544 ) ) ;
#1012 = CARTESIAN_POINT ( 'NONE',  ( 0.1905436384893574309, -0.5945559727383904480, 0.3046096357648198638 ) ) ;
#1011 = CARTESIAN_POINT ( 'NONE',  ( -0.1167294259372888832, -0.5331983348239501819, 0.3749999999999990008 ) ) ;
#1013 = CARTESIAN_POINT ( 'NONE',  ( -0.08000000000000000167, -2.183180860297908144, -0.3317586832283064280 ) ) ;
#1014 = PRODUCT_DEFINITION_FORMATION_WITH_SPECIFIED_SOURCE ( 'ANY', '', #19635, .NOT_KNOWN. ) ;
#1015 = ORIENTED_EDGE ( 'NONE', *, *, #2225, .F. ) ;
#1016 = ORIENTED_EDGE ( 'NONE', *, *, #12873, .F. ) ;
#1017 = CARTESIAN_POINT ( 'NONE',  ( 0.4137411116391392918, -1.124414850558264733, 0.5933932595712226865 ) ) ;
#1018 = CARTESIAN_POINT ( 'NONE',  ( 0.1199036801841761174, -0.5680492792121983880, 0.2364068004411575830 ) ) ;
#1019 = ORIENTED_EDGE ( 'NONE', *, *, #18787, .T. ) ;
#1020 = AXIS2_PLACEMENT_3D ( 'NONE', #17478, #14372, #39469 ) ;
#1021 = PLANE ( 'NONE',  #32255 ) ;
#1022 = CARTESIAN_POINT ( 'NONE',  ( 0.03328606440775329356, -1.535999360653146573, -0.3785507177379214272 ) ) ;
#1023 = DIRECTION ( 'NONE',  ( -0.8660512985181139101, -0.4999551463232362325, 5.802457945118985070E-16 ) ) ;
#1024 = DIRECTION ( 'NONE',  ( 0.7956551220374307176, 0.4593167559955306789, -0.3949190352937466675 ) ) ;
#1025 = DIRECTION ( 'NONE',  ( 1.000000000000000000, -0.000000000000000000, -0.000000000000000000 ) ) ;
#1026 = CARTESIAN_POINT ( 'NONE',  ( 0.3927990398488649393, -1.752501822930178310, -0.5454427608432544927 ) ) ;
#1027 = CARTESIAN_POINT ( 'NONE',  ( 0.6791199086483500347, -1.400839286187941957, 0.8214794356666539343 ) ) ;
#1028 = CARTESIAN_POINT ( 'NONE',  ( 0.3916540994123360875, -1.783423193857804234, -0.4823378820693604574 ) ) ;
#1029 = CARTESIAN_POINT ( 'NONE',  ( 0.07556315841227354002, -1.331191507351498160, 0.4849083929475443422 ) ) ;
#1030 = CARTESIAN_POINT ( 'NONE',  ( 0.03159140494780052905, -0.3316214887069903750, -0.3635694333040951909 ) ) ;
#1031 = COORDINATED_UNIVERSAL_TIME_OFFSET ( 0, 0, .AHEAD. ) ;
#1032 = AXIS2_PLACEMENT_3D ( 'NONE', #1803, #8137, #39223 ) ;
#1033 = EDGE_CURVE ( 'NONE', #31843, #3047, #36000, .T. ) ;
#1034 = CARTESIAN_POINT ( 'NONE',  ( 0.6613984642527299673, -1.498580572238303876, -0.6190489083608020637 ) ) ;
#1035 = CIRCLE ( 'NONE', #2321, 0.08000000000000000167 ) ;
#1036 = DIRECTION ( 'NONE',  ( -7.771561172376107616E-16, 7.170354002788761615E-17, -1.000000000000000000 ) ) ;
#1037 = CARTESIAN_POINT ( 'NONE',  ( 0.1848741932763747764, -0.8057379068672942957, 0.02534018588883596781 ) ) ;
#1038 = ADVANCED_FACE ( 'NONE', ( #4840 ), #1389, .F. ) ;
#1039 = CARTESIAN_POINT ( 'NONE',  ( -0.2399999999999999079, -2.109195954094405856, -0.3137251058216021793 ) ) ;
#1040 = CARTESIAN_POINT ( 'NONE',  ( -0.1743922129835729085, -0.5166151207188712791, 0.3599999999999990430 ) ) ;
#1041 = AXIS2_PLACEMENT_3D ( 'NONE', #12619, #5828, #2977 ) ;
#1042 = LOCAL_TIME ( 0, 53, 7.000000000000000000, #10758 ) ;
#1043 = CARTESIAN_POINT ( 'NONE',  ( 0.03132541776874769868, -0.7585458590990268313, 0.6287131927338691639 ) ) ;
#1044 = CARTESIAN_POINT ( 'NONE',  ( 0.5932811311191399373, -1.498634114660479133, -0.3907251365715369573 ) ) ;
#1045 = DIRECTION ( 'NONE',  ( 1.000000000000000000, 1.864905829289486282E-14, 8.132394101956133308E-16 ) ) ;
#1046 = DIRECTION ( 'NONE',  ( 0.000000000000000000, 0.000000000000000000, 1.000000000000000000 ) ) ;
#1047 = DIRECTION ( 'NONE',  ( 0.4999999999999972800, 0.5006794435238202112, -0.7066258520834632906 ) ) ;
#1048 = ORIENTED_EDGE ( 'NONE', *, *, #13178, .F. ) ;
#1049 = ORIENTED_EDGE ( 'NONE', *, *, #6247, .T. ) ;
#1050 = DIRECTION ( 'NONE',  ( -7.000205099780314469E-17, -1.000000000000000000, 6.590151126658399604E-16 ) ) ;
#1051 = ORIENTED_EDGE ( 'NONE', *, *, #37100, .T. ) ;
#1052 = DIRECTION ( 'NONE',  ( 2.682900528199994008E-31, -0.9510565162951504226, 0.3090169943749569437 ) ) ;
#1053 = CARTESIAN_POINT ( 'NONE',  ( 0.5747203984579013492, -1.612743926285909346, -0.5166151207188712791 ) ) ;
#1054 = CARTESIAN_POINT ( 'NONE',  ( 0.5536405708538106873, -1.384481591576937509, 0.6244451514967195305 ) ) ;
#1056 = ORIENTED_EDGE ( 'NONE', *, *, #26817, .F. ) ;
#1055 = CARTESIAN_POINT ( 'NONE',  ( 0.07216878364870175921, 0.000000000000000000, -0.1249999999999971689 ) ) ;
#1057 = CARTESIAN_POINT ( 'NONE',  ( 0.2043709925794569282, -0.7174950807506157435, 0.3538749514786183048 ) ) ;
#1058 = CYLINDRICAL_SURFACE ( 'NONE', #21114, 0.2500000000000000000 ) ;
#1059 = ORIENTED_EDGE ( 'NONE', *, *, #33898, .F. ) ;
#1060 = PLANE ( 'NONE',  #23186 ) ;
#1061 = VERTEX_POINT ( 'NONE', #36322 ) ;
#1062 = CARTESIAN_POINT ( 'NONE',  ( 0.3133035272563549078, -1.575440432857677431, 0.8162228474935855349 ) ) ;
#1064 = CARTESIAN_POINT ( 'NONE',  ( -0.05464101615137762630, -1.772778095317936620, -0.3120197613628934441 ) ) ;
#1063 = CARTESIAN_POINT ( 'NONE',  ( 0.6335899703865320864, -1.596177751663357736, -0.4443638777805991591 ) ) ;
#1065 = CARTESIAN_POINT ( 'NONE',  ( -0.05464101615137785528, -2.314906514113384883, -0.5881050943081593818 ) ) ;
#1066 = CIRCLE ( 'NONE', #11535, 0.1000000000000000194 ) ;
#1067 = CARTESIAN_POINT ( 'NONE',  ( 0.1365034152848375870, -1.346425269259858615, -0.3192896525261769702 ) ) ;
#1068 = ORIENTED_EDGE ( 'NONE', *, *, #17280, .F. ) ;
#1069 = TOROIDAL_SURFACE ( 'NONE', #16131, 0.04749999999977547877, 0.01000000000000000021 ) ;
#1070 = CARTESIAN_POINT ( 'NONE',  ( 0.3211452305271019769, -1.297376312664729081, 0.5471643355025310740 ) ) ;
#1071 = CARTESIAN_POINT ( 'NONE',  ( 0.1862185816537504646, -0.9153565697885686081, 0.1497573156717260934 ) ) ;
#1072 = DIRECTION ( 'NONE',  ( -0.4999551463232372317, 0.8660512985181134660, -0.000000000000000000 ) ) ;
#1073 = CARTESIAN_POINT ( 'NONE',  ( 0.5931681649608109286, -1.450353124920298331, 0.7100355140729243120 ) ) ;
#1074 = CARTESIAN_POINT ( 'NONE',  ( 0.1687818703766520989, -0.9104748073852155787, 0.6043791483695026834 ) ) ;
#1075 = ORGANIZATION ( 'NAUO-ORG1', 'UNSPECIFIED', 'UNSPECIFIED' ) ;
#1076 = CARTESIAN_POINT ( 'NONE',  ( 0.1487034783640427960, -1.203069224257576897, 0.9182092241904131757 ) ) ;
#1077 = CARTESIAN_POINT ( 'NONE',  ( 0.4232662408345057026, -1.152421473039004995, 0.4182417262808778013 ) ) ;
#1078 = CARTESIAN_POINT ( 'NONE',  ( 0.4385112828469532875, -1.229609716458687441, 0.5557375479387191008 ) ) ;
#1079 = DIRECTION ( 'NONE',  ( 0.4999551463232373427, -0.8660512985181134660, 0.000000000000000000 ) ) ;
#1080 = CARTESIAN_POINT ( 'NONE',  ( 0.1999999999999789724, -2.183180860297921466, -0.4937760292030871079 ) ) ;
#1081 = CARTESIAN_POINT ( 'NONE',  ( -0.2399999999999999079, -3.849534981189179028, -0.1910928155360645808 ) ) ;
#1082 = PERSON_AND_ORGANIZATION ( #28500, #32463 ) ;
#1083 = CARTESIAN_POINT ( 'NONE',  ( 0.05269111014006107319, -0.2828051265736319930, 0.3737594984297867851 ) ) ;
#1084 = LINE ( 'NONE', #23272, #31039 ) ;
#1085 = CARTESIAN_POINT ( 'NONE',  ( 0.2737193247896483328, -1.556389522379076906, -0.6850497769148254923 ) ) ;
#1086 = CARTESIAN_POINT ( 'NONE',  ( 0.3453377680719361131, -1.749458763706787545, 0.4498113177181523037 ) ) ;
#1087 = CARTESIAN_POINT ( 'NONE',  ( 0.3580912810175859162, -1.816808367081122366, -0.4824505002470479420 ) ) ;
#1088 = CARTESIAN_POINT ( 'NONE',  ( 0.3059973874268072103, -1.701798401340633982, 0.8340740219765057084 ) ) ;
#1089 = CIRCLE ( 'NONE', #18239, 0.03000000000000022787 ) ;
#1090 = AXIS2_PLACEMENT_3D ( 'NONE', #30733, #23972, #2555 ) ;
#1091 = CARTESIAN_POINT ( 'NONE',  ( 0.3625960434667531151, -1.762758894398492204, -0.5926935080085831142 ) ) ;
#1092 = LINE ( 'NONE', #3739, #26311 ) ;
#1093 = ORIENTED_EDGE ( 'NONE', *, *, #33885, .F. ) ;
#1094 = APPLIED_APPROVAL_ASSIGNMENT ( #40039, ( #6983 ) ) ;
#1095 = CARTESIAN_POINT ( 'NONE',  ( 0.2675603648060154716, -1.673609121357023666, 0.5605535550759273011 ) ) ;
#1096 = CARTESIAN_POINT ( 'NONE',  ( 0.5888117849411206306, -1.461768036186659847, 0.6982214778808412126 ) ) ;
#1098 = ORIENTED_EDGE ( 'NONE', *, *, #7725, .F. ) ;
#1097 = CARTESIAN_POINT ( 'NONE',  ( 0.4799438572844808015, -1.658878325107475904, -0.4199344158348157774 ) ) ;
#1099 = CIRCLE ( 'NONE', #7599, 2.001674066779347783 ) ;
#1101 = ORIENTED_EDGE ( 'NONE', *, *, #2482, .F. ) ;
#1100 = ORIENTED_EDGE ( 'NONE', *, *, #3166, .F. ) ;
#1102 = CARTESIAN_POINT ( 'NONE',  ( 0.6672755688376807992, -1.557826434319784514, 0.6345042746411464485 ) ) ;
#1103 = VERTEX_POINT ( 'NONE', #2193 ) ;
#1104 = CARTESIAN_POINT ( 'NONE',  ( -0.05464101615137796630, -1.706654027108509997, -0.06438491259384498955 ) ) ;
#1105 = CARTESIAN_POINT ( 'NONE',  ( 0.6291611629923075100, -1.616054409175744278, -0.4658884253126942543 ) ) ;
#1106 = PERSON_AND_ORGANIZATION_ROLE ( 'classification_officer' ) ;
#1107 = FACE_OUTER_BOUND ( 'NONE', #32350, .T. ) ;
#1108 = EDGE_LOOP ( 'NONE', ( #15223, #30868, #10948, #31753 ) ) ;
#1109 = CARTESIAN_POINT ( 'NONE',  ( 0.09149069872302392770, -0.8181431826323624090, 0.2735856555635383103 ) ) ;
#1110 = CARTESIAN_POINT ( 'NONE',  ( 0.3336325236675090067, -1.050835064020409160, 0.7593003920438236021 ) ) ;
#1111 = CARTESIAN_POINT ( 'NONE',  ( 0.5388828585122440451, -1.518987218245586135, 0.5695592972482714789 ) ) ;
#1112 = ORIENTED_EDGE ( 'NONE', *, *, #28978, .F. ) ;
#1113 = CARTESIAN_POINT ( 'NONE',  ( 0.1765406453986485269, -0.4888679620873611631, 0.1632814624852850782 ) ) ;
#1114 = CARTESIAN_POINT ( 'NONE',  ( 0.4438420790631848467, -1.592365463309330709, -0.4209907625009123300 ) ) ;
#1115 = DIRECTION ( 'NONE',  ( 0.000000000000000000, 0.9510565162951575280, 0.3090169943749354053 ) ) ;
#1116 = CARTESIAN_POINT ( 'NONE',  ( 0.3915481144911456268, -1.718409356248215447, 0.6204489441750801193 ) ) ;
#1117 = CARTESIAN_POINT ( 'NONE',  ( 0.4999694634270406834, -1.038248053136179960, -0.5155029497116575543 ) ) ;
#1118 = CIRCLE ( 'NONE', #36553, 0.5515209409081861525 ) ;
#1119 = CARTESIAN_POINT ( 'NONE',  ( 0.5053588047760253499, -1.583603243833816787, -0.5401600205605632254 ) ) ;
#1120 = AXIS2_PLACEMENT_3D ( 'NONE', #1706, #14226, #5154 ) ;
#1121 = DIRECTION ( 'NONE',  ( -0.4999551463232371762, 0.8660512985181134660, -0.000000000000000000 ) ) ;
#1122 = FACE_OUTER_BOUND ( 'NONE', #19630, .T. ) ;
#1123 = CARTESIAN_POINT ( 'NONE',  ( 3.244074353476664772E-08, -0.6526340382750903668, -0.1135225766990422963 ) ) ;
#1124 = CARTESIAN_POINT ( 'NONE',  ( 0.3515944374025173902, -1.098270542177856912, 0.7997119400958316859 ) ) ;
#1125 = APPLIED_SECURITY_CLASSIFICATION_ASSIGNMENT ( #20163, ( #40663 ) ) ;
#1126 =( CONVERSION_BASED_UNIT ( 'INCH', #10967 ) LENGTH_UNIT ( ) NAMED_UNIT ( #23398 ) );
#1127 = CARTESIAN_POINT ( 'NONE',  ( 0.2225889308918536924, -1.238345268919997855, 0.5682417262808776570 ) ) ;
#1128 = CARTESIAN_POINT ( 'NONE',  ( 0.02869942827333409746, -0.4892109928530976037, -0.09550568247006177569 ) ) ;
#1129 = AXIS2_PLACEMENT_3D ( 'NONE', #18383, #36706, #24181 ) ;
#1130 = CARTESIAN_POINT ( 'NONE',  ( 0.1227332031174801358, -1.426450801877330088, 0.6430247681006037164 ) ) ;
#1131 = CARTESIAN_POINT ( 'NONE',  ( 0.4929433234940127639, -1.082713786091526353, 0.5692160337251114255 ) ) ;
#1132 = PERSON_AND_ORGANIZATION_ROLE ( 'design_owner' ) ;
#1133 = ADVANCED_FACE ( 'NONE', ( #20922 ), #15017, .T. ) ;
#1134 = APPLIED_PERSON_AND_ORGANIZATION_ASSIGNMENT ( #6396, #18763, ( #8373 ) ) ;
#1135 = FACE_OUTER_BOUND ( 'NONE', #11630, .T. ) ;
#1136 = DIRECTION ( 'NONE',  ( -1.000000000000000000, -2.341930812374887555E-31, 1.664003471950578127E-31 ) ) ;
#1137 = VERTEX_POINT ( 'NONE', #7741 ) ;
#1138 = CARTESIAN_POINT ( 'NONE',  ( 0.3666666666666453800, -2.097675824466503691, -0.7286991843995640483 ) ) ;
#1139 = CARTESIAN_POINT ( 'NONE',  ( -0.3000000000000000999, -3.941790907013290823, -0.5334369376873030477 ) ) ;
#1140 = CARTESIAN_POINT ( 'NONE',  ( -0.01548846960707504251, -0.09061086148575646371, 0.5171215251571040783 ) ) ;
#1141 = ORIENTED_EDGE ( 'NONE', *, *, #11510, .T. ) ;
#1142 = VECTOR ( 'NONE', #31540, 39.37007874015748854 ) ;
#1143 = DIRECTION ( 'NONE',  ( 0.000000000000000000, 0.1725921171157338008, -0.9849933812516248333 ) ) ;
#1144 = CARTESIAN_POINT ( 'NONE',  ( 0.6387812025505826830, -1.332167957021822557, 0.7527387398627037873 ) ) ;
#1146 = ORIENTED_EDGE ( 'NONE', *, *, #3396, .T. ) ;
#1145 = ORIENTED_EDGE ( 'NONE', *, *, #12551, .T. ) ;
#1147 = B_SPLINE_CURVE_WITH_KNOTS ( 'NONE', 3,
 ( #33606, #5416, #27653, #30931, #17981, #19424, #28673, #28867 ),
 .UNSPECIFIED., .F., .F.,
 ( 4, 2, 2, 4 ),
 ( -8.478460988836644674E-17, 0.0008552058350302836837, 0.001282808752545466129, 0.001710411670060648683 ),
 .UNSPECIFIED. ) ;
#1148 = CARTESIAN_POINT ( 'NONE',  ( -0.3000000000000000999, -3.812085038045152974, -0.02801711824816576976 ) ) ;
#1149 = CARTESIAN_POINT ( 'NONE',  ( 0.02953079040095700838, -0.09152108205202422186, -0.5223162075576424090 ) ) ;
#1150 = CARTESIAN_POINT ( 'NONE',  ( 0.3048570497350418518, -1.756853555320991189, 0.5694442476137144826 ) ) ;
#1151 = CARTESIAN_POINT ( 'NONE',  ( -0.03672309138969752362, 0.4682479968340359511, -0.1092356788912411114 ) ) ;
#1152 = VERTEX_POINT ( 'NONE', #1594 ) ;
#1153 = CARTESIAN_POINT ( 'NONE',  ( 0.7175296490783633629, -1.539929330036125421, 0.8144692937752638917 ) ) ;
#1154 = EDGE_CURVE ( 'NONE', #1703, #17938, #16900, .T. ) ;
#1155 = CARTESIAN_POINT ( 'NONE',  ( 0.08811120843107830836, -0.6855307903982026385, 0.1873295917847169478 ) ) ;
#1156 = EDGE_CURVE ( 'NONE', #433, #25927, #7747, .T. ) ;
#1157 = CARTESIAN_POINT ( 'NONE',  ( 0.03015888383791201846, -0.5831136045742685292, 0.5494185303259956354 ) ) ;
#1158 = CARTESIAN_POINT ( 'NONE',  ( 0.4645154715899988407, -1.476824984445624711, 0.7857104932153542443 ) ) ;
#1160 = CARTESIAN_POINT ( 'NONE',  ( -0.1044436713285742807, -0.4741860147766008837, 0.3606502365330823690 ) ) ;
#1159 = CARTESIAN_POINT ( 'NONE',  ( 0.1460326451217981436, -1.211929559011373891, 0.9332704621650906862 ) ) ;
#1161 = CARTESIAN_POINT ( 'NONE',  ( 0.1073778561850880914, -0.9490620967497181981, 0.3854551792646946917 ) ) ;
#1162 = VERTEX_POINT ( 'NONE', #11046 ) ;
#1163 = ADVANCED_FACE ( 'NONE', ( #7927, #20504, #20717, #14322 ), #26881, .F. ) ;
#1164 = CARTESIAN_POINT ( 'NONE',  ( 0.01548846960707511190, 0.09061086148586082467, -0.5171215251570855376 ) ) ;
#1165 = CARTESIAN_POINT ( 'NONE',  ( 0.2082119840840267744, -0.7174231593591114953, 0.6726620554019909770 ) ) ;
#1166 = ADVANCED_FACE ( 'NONE', ( #18848, #18012 ), #37750, .T. ) ;
#1167 = LINE ( 'NONE', #26048, #3608 ) ;
#1168 = CARTESIAN_POINT ( 'NONE',  ( -0.05078493045284195040, -0.4632364064579148066, -0.09920061604309324266 ) ) ;
#1169 = DIRECTION ( 'NONE',  ( 0.000000000000000000, -4.555315873022820117E-16, -1.000000000000000000 ) ) ;
#1170 = APPLICATION_CONTEXT ( 'configuration controlled 3d designs of mechanical parts and assemblies' ) ;
#1171 = CARTESIAN_POINT ( 'NONE',  ( -0.2746410161513779258, -1.804235510932644004, -0.1501860188971498311 ) ) ;
#1172 = CARTESIAN_POINT ( 'NONE',  ( 0.3628146410451159598, -0.9034970372909253422, 0.7254628211502860413 ) ) ;
#1173 = B_SPLINE_SURFACE_WITH_KNOTS ( 'NONE', 3, 3, ( 
 ( #14993, #37206, #12320, #5514, #18686, #2647, #37397, #27955, #24875, #18078, #15609, #9209, #21781 ),
 ( #34310, #27742, #40278, #9026, #6120, #30631, #12506, #27546, #8813, #3065, #21391, #21587, #28155 ),
 ( #19, #19692, #25478, #28557, #31637, #31846, #38409, #28346, #3452, #430, #16010, #22394, #26097 ),
 ( #12926, #18905, #25271, #16608, #38613, #1022, #28944, #13531, #32226, #21996, #22602, #31442, #809 ) ),
 .UNSPECIFIED., .F., .F., .F.,
 ( 4, 4 ),
 ( 4, 3, 3, 3, 4 ),
 ( 0.4849526895556616202, 1.012265746469021233 ),
 ( -2.219619483495854910E-15, 0.2500000000000086597, 0.5000000000000195399, 0.7500000000000304201, 1.000000000000041300 ),
 .UNSPECIFIED. ) ;
#1174 = CARTESIAN_POINT ( 'NONE',  ( 0.5001593862222446507, -1.120530468926300927, 0.4879659633826187171 ) ) ;
#1175 = EDGE_CURVE ( 'NONE', #35830, #5083, #22257, .T. ) ;
#1176 = CARTESIAN_POINT ( 'NONE',  ( 0.01334304990240413324, -0.9205301472758444792, 0.5571205034865969186 ) ) ;
#1177 = PRODUCT_DEFINITION ( 'UNKNOWN', '', #19398, #5857 ) ;
#1178 = CARTESIAN_POINT ( 'NONE',  ( 0.02881408050860729403, 0.4517606495562046520, -0.2100211630561587550 ) ) ;
#1179 = CARTESIAN_POINT ( 'NONE',  ( 0.3264027515311576644, -1.294324649726913634, 0.4430263674525740658 ) ) ;
#1180 = CARTESIAN_POINT ( 'NONE',  ( 0.3700259886275120702, -1.148283099900891058, 0.7265771563811994627 ) ) ;
#1181 = CARTESIAN_POINT ( 'NONE',  ( 0.02869942827333529442, 0.06034320897027924124, 0.4947801815387842250 ) ) ;
#1182 = CYLINDRICAL_SURFACE ( 'NONE', #40304, 0.1946589359789742957 ) ;
#1183 = ORIENTED_EDGE ( 'NONE', *, *, #19480, .T. ) ;
#1184 = CARTESIAN_POINT ( 'NONE',  ( 0.4806319512830223850, -1.112120366466635257, -0.6266239386966213631 ) ) ;
#1185 = CARTESIAN_POINT ( 'NONE',  ( 0.09360223597190081568, -0.5959407479578081590, 0.2661619178395356333 ) ) ;
#1186 = CARTESIAN_POINT ( 'NONE',  ( -1.019575837292303166, -0.04310840302197994911, 0.3749999999999990008 ) ) ;
#1187 = CARTESIAN_POINT ( 'NONE',  ( 0.1169788285577439829, -1.415237608940837388, 0.5049415650359101448 ) ) ;
#1188 = CARTESIAN_POINT ( 'NONE',  ( 0.2764376405909636514, -1.316227483431351875, 0.6113284502048742519 ) ) ;
#1189 = ORIENTED_EDGE ( 'NONE', *, *, #24109, .T. ) ;
#1190 = CARTESIAN_POINT ( 'NONE',  ( -0.03664605387828172994, -0.3149102792626771730, -0.3635688186731564353 ) ) ;
#1191 = DIRECTION ( 'NONE',  ( 0.000000000000000000, 0.000000000000000000, -1.000000000000000000 ) ) ;
#1192 = DIRECTION ( 'NONE',  ( 1.000000000000000000, 2.341930812374887555E-31, -1.664003471950578127E-31 ) ) ;
#1193 = CARTESIAN_POINT ( 'NONE',  ( 0.4806401579603196139, -1.259507117968132528, 0.6434039063252821045 ) ) ;
#1195 = DIRECTION ( 'NONE',  ( 4.622231866529357837E-33, -0.6954292836767063113, -0.7185945389473142875 ) ) ;
#1194 = DIRECTION ( 'NONE',  ( 0.000000000000000000, 0.000000000000000000, -1.000000000000000000 ) ) ;
#1196 = CARTESIAN_POINT ( 'NONE',  ( 0.2734279889346977188, -0.9622732688880970553, 0.5233991146725487376 ) ) ;
#1197 = VERTEX_POINT ( 'NONE', #24398 ) ;
#1198 = CARTESIAN_POINT ( 'NONE',  ( -0.1531325081225953788, 0.4743613400439437022, 0.3600421117866457466 ) ) ;
#1199 = VERTEX_POINT ( 'NONE', #30966 ) ;
#1200 = EDGE_CURVE ( 'NONE', #15916, #5177, #13017, .T. ) ;
#1201 = CARTESIAN_POINT ( 'NONE',  ( 0.04900772023046805204, -0.5599104050450269821, 0.2516739294092621426 ) ) ;
#1203 = CARTESIAN_POINT ( 'NONE',  ( 0.1954949921222078613, -0.7168102854172049287, 0.3287466980362075963 ) ) ;
#1202 = DIRECTION ( 'NONE',  ( 0.4999551463232372317, -0.8660512985181135770, 0.000000000000000000 ) ) ;
#1204 = CARTESIAN_POINT ( 'NONE',  ( 0.1980860629012485552, -1.670291652337890342, -0.3592990252404365537 ) ) ;
#1205 = ORIENTED_EDGE ( 'NONE', *, *, #15467, .T. ) ;
#1206 = EDGE_CURVE ( 'NONE', #1887, #18158, #5122, .T. ) ;
#1207 = CARTESIAN_POINT ( 'NONE',  ( -0.08000000000000000167, -1.750394882718339762, -0.1142373872069606250 ) ) ;
#1208 = ADVANCED_FACE ( 'NONE', ( #24612 ), #5032, .F. ) ;
#1209 = CARTESIAN_POINT ( 'NONE',  ( 0.1191842311548099581, -0.5541223904023430125, 0.1890049277065241062 ) ) ;
#1210 = TOROIDAL_SURFACE ( 'NONE', #30078, 0.04249999999999999611, 0.02499999999999995628 ) ;
#1211 = VERTEX_POINT ( 'NONE', #15552 ) ;
#1212 = CARTESIAN_POINT ( 'NONE',  ( 0.07499999999999960865, 0.000000000000000000, 0.000000000000000000 ) ) ;
#1213 = CARTESIAN_POINT ( 'NONE',  ( 0.02872242845529756824, -0.5252126300208226350, 0.08844866507292684088 ) ) ;
#1214 = DIRECTION ( 'NONE',  ( 1.000000000000000000, 0.000000000000000000, 0.000000000000000000 ) ) ;
#1215 = DIRECTION ( 'NONE',  ( 1.000000000000000000, 0.000000000000000000, 0.000000000000000000 ) ) ;
#1216 = CARTESIAN_POINT ( 'NONE',  ( 0.3693619091536758936, -1.731651576748437948, 0.6146617367520950115 ) ) ;
#1217 = DIRECTION ( 'NONE',  ( 5.551115123125799958E-17, -4.553079989440443628E-16, -1.000000000000000000 ) ) ;
#1218 = CARTESIAN_POINT ( 'NONE',  ( 0.7412791958894395794, -1.507305061506947430, 0.6536223584324379887 ) ) ;
#1219 = EDGE_CURVE ( 'NONE', #37479, #23130, #40629, .T. ) ;
#1220 = CARTESIAN_POINT ( 'NONE',  ( -0.2399999999999999079, -4.289222312108804225, -0.5708809693675255259 ) ) ;
#1221 = EDGE_CURVE ( 'NONE', #20994, #2590, #10391, .T. ) ;
#1222 = FACE_OUTER_BOUND ( 'NONE', #3689, .T. ) ;
#1223 = PERSON_AND_ORGANIZATION ( #28500, #32463 ) ;
#1224 = EDGE_CURVE ( 'NONE', #9524, #13839, #31428, .T. ) ;
#1225 = CARTESIAN_POINT ( 'NONE',  ( 0.6164351338053631890, -1.544991685130753911, -0.6274595476820803430 ) ) ;
#1226 = EDGE_CURVE ( 'NONE', #23547, #31675, #11053, .T. ) ;
#1227 = CARTESIAN_POINT ( 'NONE',  ( 0.04157143636675632997, 0.2900120080285063517, 0.3701876636500653350 ) ) ;
#1228 = CARTESIAN_POINT ( 'NONE',  ( -0.2399999999999999079, -3.985676108854518507, -0.7623095129438225426 ) ) ;
#1229 = PLANE ( 'NONE',  #29063 ) ;
#1230 = CARTESIAN_POINT ( 'NONE',  ( -0.04293701532779588964, 0.4875995331660218923, -0.08291810260646380326 ) ) ;
#1231 =( BOUNDED_SURFACE ( )  B_SPLINE_SURFACE ( 3, 2, ( 
 ( #10864, #13545, #11064 ),
 ( #23437, #11256, #32449 ),
 ( #32660, #35953, #16840 ),
 ( #10646, #23011, #23221 ),
 ( #20524, #36347, #8164 ),
 ( #17435, #1823, #14339 ),
 ( #1618, #29382, #38626 ),
 ( #1227, #29572, #32850 ),
 ( #13726, #1413, #7558 ),
 ( #35746, #4653, #26116 ),
 ( #29777, #26902, #23825 ),
 ( #14141, #32238, #10445 ),
 ( #16625, #29172, #4465 ),
 ( #7334, #17032, #26292 ),
 ( #20132, #5473, #21133 ),
 ( #5266, #8368, #39847 ),
 ( #27319, #33265, #37170 ),
 ( #24838, #5074, #8985 ) ),
 .UNSPECIFIED., .F., .F., .F. ) 
 B_SPLINE_SURFACE_WITH_KNOTS ( ( 4, 2, 2, 2, 2, 2, 2, 2, 4 ),
 ( 3, 3 ),
 ( -0.001532620576208852279, -0.0007637936630077650328, 5.033250193322322090E-06, 0.0007738601633944096770, 0.001542687076595496923, 0.002311513989796584387, 0.003080340902997671416, 0.003849167816198758880, 0.004617994729399846343 ),
 ( 0.000000000000000000, 1.000000000000000000 ),
 .UNSPECIFIED. ) 
 GEOMETRIC_REPRESENTATION_ITEM ( )  RATIONAL_B_SPLINE_SURFACE ( (
 ( 1.000000000000000000, 0.7283825911960446486, 1.000000000000000000),
 ( 1.000000000000000000, 0.7404385082113230654, 1.000000000000000000),
 ( 1.000000000000000000, 0.7521504257739481947, 1.000000000000000000),
 ( 1.000000000000000000, 0.7744497410760382561, 1.000000000000000000),
 ( 1.000000000000000000, 0.7845654757373583532, 1.000000000000000000),
 ( 1.000000000000000000, 0.8022083990892612260, 1.000000000000000000),
 ( 1.000000000000000000, 0.8094167424699770796, 1.000000000000000000),
 ( 1.000000000000000000, 0.8194491993616178638, 1.000000000000000000),
 ( 1.000000000000000000, 0.8220634900779653087, 1.000000000000000000),
 ( 1.000000000000000000, 0.8220705070824310123, 1.000000000000000000),
 ( 1.000000000000000000, 0.8194468812480258935, 1.000000000000000000),
 ( 1.000000000000000000, 0.8094220769840151375, 1.000000000000000000),
 ( 1.000000000000000000, 0.8022659121985437070, 1.000000000000000000),
 ( 1.000000000000000000, 0.7845681159035545749, 1.000000000000000000),
 ( 1.000000000000000000, 0.7744426415185606816, 1.000000000000000000),
 ( 1.000000000000000000, 0.7522890290928357926, 1.000000000000000000),
 ( 1.000000000000000000, 0.7403540167215627577, 1.000000000000000000),
 ( 1.000000000000000000, 0.7283825911960218891, 1.000000000000000000) ) ) 
 REPRESENTATION_ITEM ( '' )  SURFACE ( )  );
#1232 = CARTESIAN_POINT ( 'NONE',  ( -8.537024980200822558E-17, -0.6872203660140405734, 0.09557912180100291977 ) ) ;
#1233 = CARTESIAN_POINT ( 'NONE',  ( 0.5951414857627569388, -1.550313246946717571, -0.4562001837530886839 ) ) ;
#1234 = FACE_OUTER_BOUND ( 'NONE', #16538, .T. ) ;
#1235 = CARTESIAN_POINT ( 'NONE',  ( 0.4954266169953891463, -1.646634881173000720, -0.6269490058875392124 ) ) ;
#1236 = CARTESIAN_POINT ( 'NONE',  ( -0.05137569054208568353, -0.2953118892970992282, 0.3683837247633758305 ) ) ;
#1237 = CIRCLE ( 'NONE', #21573, 0.01500000000000002894 ) ;
#1238 = ORIENTED_EDGE ( 'NONE', *, *, #7385, .F. ) ;
#1239 = VERTEX_POINT ( 'NONE', #13660 ) ;
#1240 = CARTESIAN_POINT ( 'NONE',  ( 0.1436225252650951412, -1.283668529478381393, 0.4687417262808780127 ) ) ;
#1241 = ORIENTED_EDGE ( 'NONE', *, *, #13651, .T. ) ;
#1242 = DIRECTION ( 'NONE',  ( 1.000000000000000000, -0.000000000000000000, -0.000000000000000000 ) ) ;
#1243 = SPHERICAL_SURFACE ( 'NONE', #1597, 0.01499999999999999944 ) ;
#1244 = CARTESIAN_POINT ( 'NONE',  ( 0.5446150423827782472, -1.368799154680095942, 0.7286756449045225237 ) ) ;
#1246 = VERTEX_POINT ( 'NONE', #13258 ) ;
#1245 = CARTESIAN_POINT ( 'NONE',  ( 0.3484677573834994435, -1.177852168535778565, 0.4182417262808778013 ) ) ;
#1247 = CARTESIAN_POINT ( 'NONE',  ( 0.4661750196922136991, -1.070732324447800421, 0.6917658376937553255 ) ) ;
#1248 = CARTESIAN_POINT ( 'NONE',  ( -1.502516396515344672E-15, -0.3899999999999999578, 5.463695987328526437E-16 ) ) ;
#1249 = VERTEX_POINT ( 'NONE', #962 ) ;
#1250 = CARTESIAN_POINT ( 'NONE',  ( 0.1499999999999994671, -0.5198120922912051745, -0.07362328916749329155 ) ) ;
#1251 = ORIENTED_EDGE ( 'NONE', *, *, #31298, .T. ) ;
#1252 = CARTESIAN_POINT ( 'NONE',  ( 0.02322307456033121872, -0.5318894034165193574, 0.1546977929980313804 ) ) ;
#1254 = DIRECTION ( 'NONE',  ( 1.060606950627616897E-16, 6.122684696619992497E-17, 1.000000000000000000 ) ) ;
#1253 = CARTESIAN_POINT ( 'NONE',  ( 0.6071598558232448317, -1.592990773492276357, 0.4345894283230820609 ) ) ;
#1255 = DIRECTION ( 'NONE',  ( 0.000000000000000000, -0.8090169943749496717, -0.5877852522924700285 ) ) ;
#1256 = ADVANCED_FACE ( 'NONE', ( #29312 ), #25828, .F. ) ;
#1257 = CARTESIAN_POINT ( 'NONE',  ( 0.06734526529546210061, -1.429207128842583163, -0.3669778653616447839 ) ) ;
#1258 = ORIENTED_EDGE ( 'NONE', *, *, #14188, .T. ) ;
#1259 = EDGE_CURVE ( 'NONE', #18158, #33923, #16312, .T. ) ;
#1260 = CARTESIAN_POINT ( 'NONE',  ( -0.01548846960707517956, -0.3772621329472692908, -0.3651003739303438911 ) ) ;
#1261 = CARTESIAN_POINT ( 'NONE',  ( 0.1872878105913098612, -0.8400613882515264308, 0.2180701053272094680 ) ) ;
#1262 = CARTESIAN_POINT ( 'NONE',  ( 0.1734397871105309574, -1.266755107815962678, 0.4263792231164484359 ) ) ;
#1263 = CARTESIAN_POINT ( 'NONE',  ( -0.2399999999999999079, -2.068584980338025847, -0.2731141320652225035 ) ) ;
#1264 = CARTESIAN_POINT ( 'NONE',  ( 0.1026041305702724421, -0.8285543066798866096, 0.1791339961852569385 ) ) ;
#1265 = CARTESIAN_POINT ( 'NONE',  ( -0.2746410161513779258, -1.730153431576819001, -0.08301574631829765349 ) ) ;
#1266 = CARTESIAN_POINT ( 'NONE',  ( 0.4864384408240609581, -1.181579935974320650, 0.4182417262808778013 ) ) ;
#1267 = CARTESIAN_POINT ( 'NONE',  ( -0.1529745177444690185, 0.4738847129974373962, 0.3606502365071603822 ) ) ;
#1268 = FACE_OUTER_BOUND ( 'NONE', #19998, .T. ) ;
#1269 = CARTESIAN_POINT ( 'NONE',  ( 0.05082303569918617675, 0.4631054925596486127, 0.09932635337952074039 ) ) ;
#1270 = PLANE ( 'NONE',  #22723 ) ;
#1271 = FACE_OUTER_BOUND ( 'NONE', #28939, .T. ) ;
#1272 = EDGE_CURVE ( 'NONE', #7197, #29556, #1237, .T. ) ;
#1273 = CARTESIAN_POINT ( 'NONE',  ( 0.3504057387187117234, -1.153664717295437070, 0.4422128889498894710 ) ) ;
#1274 = DIRECTION ( 'NONE',  ( 1.000000000000000000, -0.000000000000000000, -0.000000000000000000 ) ) ;
#1275 = DIRECTION ( 'NONE',  ( -1.000000000000000000, 0.000000000000000000, -5.691349986800505477E-16 ) ) ;
#1276 = CARTESIAN_POINT ( 'NONE',  ( -0.1743922129835729085, -0.5166151207188712791, 0.3750000000000001110 ) ) ;
#1277 = CARTESIAN_POINT ( 'NONE',  ( 0.3663377407856179269, -1.767777433818015220, -0.5763279985969705921 ) ) ;
#1278 = CARTESIAN_POINT ( 'NONE',  ( 0.3204139389452037023, -1.755336229099433654, 0.4849083929475442867 ) ) ;
#1279 = CARTESIAN_POINT ( 'NONE',  ( 0.7053080889764471451, -1.513942001867420339, 0.5667347313869608438 ) ) ;
#1280 = ORIENTED_EDGE ( 'NONE', *, *, #19499, .F. ) ;
#1281 = CARTESIAN_POINT ( 'NONE',  ( 0.5429359209136535025, -1.169310040315109545, 0.5682417262808779901 ) ) ;
#1282 = EDGE_LOOP ( 'NONE', ( #31892, #34657, #27826, #15822 ) ) ;
#1283 = CARTESIAN_POINT ( 'NONE',  ( 0.2679398507666006513, -1.673757272405929752, 0.5655069686649734084 ) ) ;
#1284 = CARTESIAN_POINT ( 'NONE',  ( 0.6018252865098940863, -1.483102701789519973, 0.5702406811564502132 ) ) ;
#1286 = ORIENTED_EDGE ( 'NONE', *, *, #27088, .T. ) ;
#1285 = DIRECTION ( 'NONE',  ( -1.000000000000000000, -1.450080480853946466E-15, 8.188689774234050758E-16 ) ) ;
#1288 = VERTEX_POINT ( 'NONE', #22542 ) ;
#1287 = ORIENTED_EDGE ( 'NONE', *, *, #9712, .T. ) ;
#1289 = CARTESIAN_POINT ( 'NONE',  ( 0.2400030092520472336, -0.7789576557571062931, 0.7291493276161450376 ) ) ;
#1290 = ORIENTED_EDGE ( 'NONE', *, *, #492, .F. ) ;
#1291 = ORIENTED_EDGE ( 'NONE', *, *, #15550, .T. ) ;
#1292 = CARTESIAN_POINT ( 'NONE',  ( -0.01256779751711274359, -0.5607309962333324460, 0.2869151978856656626 ) ) ;
#1294 = CARTESIAN_POINT ( 'NONE',  ( 0.1915833156076485189, -1.371527921740720135, 0.5547766577986595893 ) ) ;
#1293 = CARTESIAN_POINT ( 'NONE',  ( 0.05187277790672186611, 0.4419080096627359122, 0.1624279055868750321 ) ) ;
#1295 = CARTESIAN_POINT ( 'NONE',  ( 0.3740960844805631957, -1.108072201694596526, 0.5182417262812423209 ) ) ;
#1296 = DATE_AND_TIME ( #4348, #13576 ) ;
#1297 = EDGE_CURVE ( 'NONE', #19690, #11981, #3809, .T. ) ;
#1298 = CARTESIAN_POINT ( 'NONE',  ( 0.0006246259811798426324, -0.9534082139883233165, 0.04185307883324813905 ) ) ;
#1300 = ORIENTED_EDGE ( 'NONE', *, *, #21493, .T. ) ;
#1299 = ORIENTED_EDGE ( 'NONE', *, *, #9495, .T. ) ;
#1301 = B_SPLINE_CURVE_WITH_KNOTS ( 'NONE', 3,
 ( #24995, #18845, #33861, #21712 ),
 .UNSPECIFIED., .F., .F.,
 ( 4, 4 ),
 ( 0.000000000000000000, 0.0002458494465879629775 ),
 .UNSPECIFIED. ) ;
#1302 = CARTESIAN_POINT ( 'NONE',  ( 0.1576472890307486219, -0.8786603732910064357, 0.5360059036955113765 ) ) ;
#1303 = CARTESIAN_POINT ( 'NONE',  ( 0.1291963080521598140, -0.7094397666660188229, 0.4795944692163690570 ) ) ;
#1304 = CARTESIAN_POINT ( 'NONE',  ( 0.1108305878322193849, -0.5649205625374638107, 0.2321049223534430439 ) ) ;
#1305 = CARTESIAN_POINT ( 'NONE',  ( 0.03052449867241842710, -1.064021556079522535, 0.6116746401987742665 ) ) ;
#1306 = CARTESIAN_POINT ( 'NONE',  ( 0.4243666725459964151, -1.591076223527387423, -0.4156371400837810537 ) ) ;
#1307 = DIRECTION ( 'NONE',  ( -1.000000000000000000, -0.000000000000000000, -0.000000000000000000 ) ) ;
#1308 = LINE ( 'NONE', #35428, #6856 ) ;
#1309 = FACE_OUTER_BOUND ( 'NONE', #32759, .T. ) ;
#1310 = CARTESIAN_POINT ( 'NONE',  ( -0.01548846960707524721, 0.09061086148575919763, -0.5171215251571033011 ) ) ;
#1311 = CARTESIAN_POINT ( 'NONE',  ( -0.02000000000000000042, -1.944084441611813707, -0.4562887203618206655 ) ) ;
#1312 = DIRECTION ( 'NONE',  ( -1.000000000000000000, -0.000000000000000000, -0.000000000000000000 ) ) ;
#1313 = CARTESIAN_POINT ( 'NONE',  ( 0.01148915324952597475, -0.8840235622257791581, -0.02343339859393702568 ) ) ;
#1314 = CARTESIAN_POINT ( 'NONE',  ( 0.06942125022148733227, -0.5427962089461003670, 0.1770506202226188042 ) ) ;
#1315 = DIRECTION ( 'NONE',  ( 0.000000000000000000, -0.5127411190260188212, -0.8585432690668224343 ) ) ;
#1316 = CARTESIAN_POINT ( 'NONE',  ( -0.06980746140711623082, 5.828670879282072084E-17, 0.1749999999999999889 ) ) ;
#1317 = CARTESIAN_POINT ( 'NONE',  ( 0.1849096901904442591, -1.549205955729530793, 0.5682417262808778791 ) ) ;
#1318 = CARTESIAN_POINT ( 'NONE',  ( 0.3318484986314376162, -0.9704704429389122700, 0.6048456486855374736 ) ) ;
#1319 = APPROVAL_DATE_TIME ( #29475, #7104 ) ;
#1320 = CARTESIAN_POINT ( 'NONE',  ( 0.7255563027409094312, -1.477976514587821422, 0.7347025679090390948 ) ) ;
#1321 = EDGE_CURVE ( 'NONE', #10838, #32882, #34705, .T. ) ;
#1322 = CARTESIAN_POINT ( 'NONE',  ( -0.01548846960721190873, 0.4730347584884290191, -0.2341461249027944058 ) ) ;
#1323 = CARTESIAN_POINT ( 'NONE',  ( 0.3061892459480512474, -1.759162422899352318, 0.5694323708298315578 ) ) ;
#1324 = ORIENTED_EDGE ( 'NONE', *, *, #38545, .T. ) ;
#1325 = DIRECTION ( 'NONE',  ( 0.000000000000000000, 0.000000000000000000, -1.000000000000000000 ) ) ;
#1326 = CARTESIAN_POINT ( 'NONE',  ( -0.2399999999999999079, -1.804235510932644004, -0.1501860188971498311 ) ) ;
#1327 = PLANE ( 'NONE',  #30508 ) ;
#1328 = ORIENTED_EDGE ( 'NONE', *, *, #40432, .F. ) ;
#1329 = CARTESIAN_POINT ( 'NONE',  ( -0.3000000000000000999, -2.289343986263487896, -0.7686455968847020204 ) ) ;
#1330 = CARTESIAN_POINT ( 'NONE',  ( 0.4381829047093346863, -1.020301330954181518, 0.7847444992166355826 ) ) ;
#1332 = ORIENTED_EDGE ( 'NONE', *, *, #18204, .T. ) ;
#1331 = ORIENTED_EDGE ( 'NONE', *, *, #35960, .T. ) ;
#1333 = CARTESIAN_POINT ( 'NONE',  ( 0.1315192713089369247, -1.308544259391007492, -0.6883081435772964163 ) ) ;
#1334 = VERTEX_POINT ( 'NONE', #37958 ) ;
#1335 = CARTESIAN_POINT ( 'NONE',  ( 0.3351195522891313172, -1.762354232558481337, 0.5631496603913015431 ) ) ;
#1336 = FACE_OUTER_BOUND ( 'NONE', #15794, .T. ) ;
#1337 = CARTESIAN_POINT ( 'NONE',  ( -0.04230258372739850031, 0.4443637212174484930, -0.1488268768076315418 ) ) ;
#1338 = ORIENTED_EDGE ( 'NONE', *, *, #13424, .F. ) ;
#1339 = CARTESIAN_POINT ( 'NONE',  ( 0.7541811597904449771, -1.515850492646690473, 0.8047797755351335791 ) ) ;
#1340 = CARTESIAN_POINT ( 'NONE',  ( 0.08947262244426219813, -0.6461490780200273010, 0.1933266256753762846 ) ) ;
#1341 = CARTESIAN_POINT ( 'NONE',  ( 0.0004750029074822290955, -0.4386152177297633070, 0.1882660082133467416 ) ) ;
#1342 = VECTOR ( 'NONE', #22126, 39.37007874015748854 ) ;
#1343 = CARTESIAN_POINT ( 'NONE',  ( 0.3025071352787032652, -1.151881836541575721, 0.8404721679195121808 ) ) ;
#1345 = CARTESIAN_POINT ( 'NONE',  ( 0.3163996966746501771, -1.646713064435177731, 0.5991727703659502913 ) ) ;
#1344 = CARTESIAN_POINT ( 'NONE',  ( 0.2172267109180897882, -1.451647963948341058, 0.9382086856453861756 ) ) ;
#1346 = CARTESIAN_POINT ( 'NONE',  ( 0.1020516685261761286, -0.9421306251871297555, 0.3381412032200973861 ) ) ;
#1347 = ORIENTED_EDGE ( 'NONE', *, *, #21802, .T. ) ;
#1348 = DIRECTION ( 'NONE',  ( -1.000000000000000000, -6.779273404243070203E-32, -4.314083075427408311E-32 ) ) ;
#1349 = CARTESIAN_POINT ( 'NONE',  ( 0.2248552728485077867, -0.5917194789810457101, 0.4907616766386495022 ) ) ;
#1350 = DIRECTION ( 'NONE',  ( -1.000000000000000000, -6.779273404243070203E-32, -4.314083075427408311E-32 ) ) ;
#1351 = CARTESIAN_POINT ( 'NONE',  ( -0.05464101615137761936, -1.845925619402022155, -0.2644148183989317724 ) ) ;
#1352 = SPHERICAL_SURFACE ( 'NONE', #37169, 0.01499999999999999944 ) ;
#1353 = CARTESIAN_POINT ( 'NONE',  ( 0.1180487212903242045, -1.414513468998023660, 0.5470211090928080999 ) ) ;
#1354 = CARTESIAN_POINT ( 'NONE',  ( 0.6117231882494743589, -1.284912631992666254, 0.6460020013211499323 ) ) ;
#1355 = CARTESIAN_POINT ( 'NONE',  ( 0.07216878364870298046, 0.08000000000000023759, -0.1249999999999999029 ) ) ;
#1356 = CARTESIAN_POINT ( 'NONE',  ( 0.01797837544738539739, -0.9279355173420600345, 0.5914959875658215571 ) ) ;
#1357 = CARTESIAN_POINT ( 'NONE',  ( 0.03070601528493977633, -1.915553355962458459, -0.3085447803061387995 ) ) ;
#1358 = CARTESIAN_POINT ( 'NONE',  ( 0.5325603410779075064, -1.633963683135810641, -0.5997096917800632809 ) ) ;
#1359 = ORIENTED_EDGE ( 'NONE', *, *, #22868, .F. ) ;
#1360 = ADVANCED_FACE ( 'NONE', ( #3388 ), #19225, .T. ) ;
#1361 = CARTESIAN_POINT ( 'NONE',  ( 0.4171940613675130805, -1.169327234610036292, 0.7033695205199608225 ) ) ;
#1362 = CARTESIAN_POINT ( 'NONE',  ( -0.05464101615137762630, -1.910390638264138685, -0.8220407338378623585 ) ) ;
#1363 = CARTESIAN_POINT ( 'NONE',  ( -0.05615703521555034244, -0.2616264896058714262, -0.3776298641847865012 ) ) ;
#1364 = EDGE_CURVE ( 'NONE', #36154, #36726, #4129, .T. ) ;
#1365 = AXIS2_PLACEMENT_3D ( 'NONE', #21193, #33953, #37234 ) ;
#1366 = ORIENTED_EDGE ( 'NONE', *, *, #1156, .T. ) ;
#1367 = CARTESIAN_POINT ( 'NONE',  ( 0.5241818771854670489, -1.140424305731243981, 0.6527584601043535661 ) ) ;
#1368 = CARTESIAN_POINT ( 'NONE',  ( 0.09129909826610711765, -0.5802035170451905755, 0.2220056307398889928 ) ) ;
#1369 = ADVANCED_FACE ( 'NONE', ( #23561 ), #26823, .T. ) ;
#1370 = DIRECTION ( 'NONE',  ( 0.000000000000000000, 0.000000000000000000, 1.000000000000000000 ) ) ;
#1371 = LINE ( 'NONE', #39392, #38362 ) ;
#1372 = EDGE_CURVE ( 'NONE', #16786, #1527, #17823, .T. ) ;
#1373 = CARTESIAN_POINT ( 'NONE',  ( 0.07923844099270259400, -0.8780064891624800305, 0.4970579955510663339 ) ) ;
#1374 = ORIENTED_EDGE ( 'NONE', *, *, #23575, .F. ) ;
#1375 = CARTESIAN_POINT ( 'NONE',  ( -0.1638575715552559042, 0.5090525736530187029, 0.3414257732885224161 ) ) ;
#1376 = DIRECTION ( 'NONE',  ( 0.000000000000000000, 0.000000000000000000, 1.000000000000000000 ) ) ;
#1377 = CARTESIAN_POINT ( 'NONE',  ( -0.06980746140711623082, 0.000000000000000000, 0.000000000000000000 ) ) ;
#1378 = DIRECTION ( 'NONE',  ( 4.930380657631319405E-32, 0.4913225862583635584, 0.8709776783778060416 ) ) ;
#1379 = CARTESIAN_POINT ( 'NONE',  ( 0.4799067833796559768, -1.259349870180440867, 0.5814271704687581366 ) ) ;
#1381 = CARTESIAN_POINT ( 'NONE',  ( 0.5303494909463689622, -1.149217331578959334, 0.5682610892518529244 ) ) ;
#1380 = CARTESIAN_POINT ( 'NONE',  ( -0.2399999999999999079, -2.511040369707300268, -0.6548468226404909887 ) ) ;
#1382 = CARTESIAN_POINT ( 'NONE',  ( 0.1897171943901793389, -0.9163440338727294465, 0.2193954077252403545 ) ) ;
#1383 = ORIENTED_EDGE ( 'NONE', *, *, #23535, .T. ) ;
#1384 = CARTESIAN_POINT ( 'NONE',  ( -0.05464101615137773038, -2.585754275622221154, -0.2040099479399058724 ) ) ;
#1385 = ORIENTED_EDGE ( 'NONE', *, *, #29103, .F. ) ;
#1386 = CARTESIAN_POINT ( 'NONE',  ( 0.4137368557930669044, -1.589575952096031308, 0.5753881675367246151 ) ) ;
#1387 = ADVANCED_FACE ( 'NONE', ( #36491 ), #26647, .F. ) ;
#1389 = CYLINDRICAL_SURFACE ( 'NONE', #5778, 0.2149999999999999967 ) ;
#1388 = CARTESIAN_POINT ( 'NONE',  ( 0.08870872266905797943, -0.5912816985501267997, 0.03819782855198166488 ) ) ;
#1390 = CARTESIAN_POINT ( 'NONE',  ( 0.2047062219756962675, -1.651037923760164228, -0.3589593011634661934 ) ) ;
#1391 = APPLIED_PERSON_AND_ORGANIZATION_ASSIGNMENT ( #39682, #11520, ( #1177 ) ) ;
#1392 = VERTEX_POINT ( 'NONE', #36270 ) ;
#1393 = AXIS2_PLACEMENT_3D ( 'NONE', #8528, #18400, #17788 ) ;
#1394 = VERTEX_POINT ( 'NONE', #39178 ) ;
#1395 = CARTESIAN_POINT ( 'NONE',  ( -0.2399999999999999079, -2.458279774191353351, -0.8760505995903041798 ) ) ;
#1396 = CARTESIAN_POINT ( 'NONE',  ( 0.1208409751158145834, -0.5758948413296848257, 0.2589058236990056661 ) ) ;
#1397 = ORIENTED_EDGE ( 'NONE', *, *, #18213, .T. ) ;
#1398 = CARTESIAN_POINT ( 'NONE',  ( 0.2914323826288400809, -1.233685883474753497, -0.5166151207188711680 ) ) ;
#1399 = CARTESIAN_POINT ( 'NONE',  ( 0.01548846960707197032, -0.4730347584886857581, 0.2341461249029804237 ) ) ;
#1400 = TOROIDAL_SURFACE ( 'NONE', #35517, 0.07749999999977555398, 0.01000000000000000021 ) ;
#1401 = CARTESIAN_POINT ( 'NONE',  ( 0.6059136413949802735, -1.592571915802247329, 0.4262670158568807044 ) ) ;
#1402 = CIRCLE ( 'NONE', #24374, 0.1400000000000008182 ) ;
#1403 = CARTESIAN_POINT ( 'NONE',  ( 0.2311145781227797180, -1.233632278668805649, 0.4896568257691081283 ) ) ;
#1404 = AXIS2_PLACEMENT_3D ( 'NONE', #9105, #17757, #21271 ) ;
#1405 = DIRECTION ( 'NONE',  ( 0.000000000000000000, 0.000000000000000000, 1.000000000000000000 ) ) ;
#1406 = CARTESIAN_POINT ( 'NONE',  ( -0.01548846960707531660, -0.2372406987223574237, 0.4850946823762633531 ) ) ;
#1407 = B_SPLINE_CURVE_WITH_KNOTS ( 'NONE', 3,
 ( #22209, #21787, #3859, #15614 ),
 .UNSPECIFIED., .F., .F.,
 ( 4, 4 ),
 ( 0.000000000000000000, 0.0005595226744648492193 ),
 .UNSPECIFIED. ) ;
#1408 = CARTESIAN_POINT ( 'NONE',  ( 0.3390826044135689665, -0.8321809361840178942, 0.7462327844847882474 ) ) ;
#1409 = FACE_OUTER_BOUND ( 'NONE', #21743, .T. ) ;
#1410 = CARTESIAN_POINT ( 'NONE',  ( -1.019575837292303166, -0.04310840302197994911, 0.3749999999999990008 ) ) ;
#1411 = PERSON_AND_ORGANIZATION_ROLE ( 'creator' ) ;
#1412 = PLANE ( 'NONE',  #6759 ) ;
#1413 = CARTESIAN_POINT ( 'NONE',  ( 0.05268932808080566133, 0.2828369400135311573, 0.3737413977152168609 ) ) ;
#1414 = DIRECTION ( 'NONE',  ( 0.000000000000000000, 0.000000000000000000, -1.000000000000000000 ) ) ;
#1415 = CARTESIAN_POINT ( 'NONE',  ( 0.4591673992659657810, -1.217701019417315456, 0.4854672771262538711 ) ) ;
#1416 = CARTESIAN_POINT ( 'NONE',  ( 0.09075966053248608889, -1.322849613925215939, 0.4537811506657316030 ) ) ;
#1417 = EDGE_CURVE ( 'NONE', #20049, #23858, #4477, .T. ) ;
#1418 = CARTESIAN_POINT ( 'NONE',  ( 0.008416785622808892545, -0.6338120178247520498, 0.4051738709354697487 ) ) ;
#1419 = CARTESIAN_POINT ( 'NONE',  ( 0.5834653944837133732, -1.511631883459902514, -0.5858460414140914674 ) ) ;
#1420 = EDGE_CURVE ( 'NONE', #23564, #13401, #8503, .T. ) ;
#1421 = DIRECTION ( 'NONE',  ( -1.000000000000000000, 0.000000000000000000, 0.000000000000000000 ) ) ;
#1422 = CIRCLE ( 'NONE', #6633, 2.001674066779347783 ) ;
#1423 = CARTESIAN_POINT ( 'NONE',  ( 0.5860257985473380504, -1.592810714289444762, 0.4182417262808776903 ) ) ;
#1424 = CARTESIAN_POINT ( 'NONE',  ( -0.04762200653274045736, -0.2475542241873569527, 0.4137947767341018102 ) ) ;
#1425 = AXIS2_PLACEMENT_3D ( 'NONE', #15329, #2990, #3751 ) ;
#1426 = ADVANCED_FACE ( 'NONE', ( #7879 ), #20945, .T. ) ;
#1427 = VERTEX_POINT ( 'NONE', #20669 ) ;
#1428 = ORIENTED_EDGE ( 'NONE', *, *, #23324, .T. ) ;
#1429 = CARTESIAN_POINT ( 'NONE',  ( 0.3650258023173150734, -1.764296560404615466, -0.5885076244517606359 ) ) ;
#1430 = ORIENTED_EDGE ( 'NONE', *, *, #17759, .T. ) ;
#1431 = CARTESIAN_POINT ( 'NONE',  ( 0.01548846960707292615, -0.2306506793133126232, -0.4716198300880852790 ) ) ;
#1432 = DIRECTION ( 'NONE',  ( 1.000000000000000000, 0.000000000000000000, 0.000000000000000000 ) ) ;
#1433 = AXIS2_PLACEMENT_3D ( 'NONE', #28038, #88, #40362 ) ;
#1434 = CARTESIAN_POINT ( 'NONE',  ( 0.5120527146466833379, -1.317106629872495160, 0.7639365440521486139 ) ) ;
#1436 = ORIENTED_EDGE ( 'NONE', *, *, #36419, .T. ) ;
#1435 = CARTESIAN_POINT ( 'NONE',  ( -0.1617555154933660866, 0.4683069300263329460, 0.1178658435716244679 ) ) ;
#1437 = CARTESIAN_POINT ( 'NONE',  ( 0.2182827306251404198, -0.8246641648518335810, 0.4150641157079975052 ) ) ;
#1438 = LINE ( 'NONE', #17051, #25037 ) ;
#1439 = EDGE_LOOP ( 'NONE', ( #38172, #28947, #24871, #22597 ) ) ;
#1440 = CARTESIAN_POINT ( 'NONE',  ( -0.01548846960688914087, 0.3772621329476823493, -0.3651003739306282747 ) ) ;
#1441 = CARTESIAN_POINT ( 'NONE',  ( 0.2654007536097648390, -1.440376723817250237, 0.9058617339288995707 ) ) ;
#1442 = EDGE_CURVE ( 'NONE', #32978, #17370, #29921, .T. ) ;
#1444 = CARTESIAN_POINT ( 'NONE',  ( 0.2009277952559025970, -1.274385821372987060, -0.3194728440340255382 ) ) ;
#1443 = CARTESIAN_POINT ( 'NONE',  ( 0.6929203575076985366, -1.501108135639614094, 0.4708622924348231931 ) ) ;
#1445 = CARTESIAN_POINT ( 'NONE',  ( 0.4092450614235220163, -1.131740385117829817, 0.4687417262808780127 ) ) ;
#1446 = EDGE_CURVE ( 'NONE', #36014, #16165, #31483, .T. ) ;
#1447 = CARTESIAN_POINT ( 'NONE',  ( 0.004899539180344515861, -1.812954824892113237, -0.3559391749954987083 ) ) ;
#1448 = ORIENTED_EDGE ( 'NONE', *, *, #33089, .F. ) ;
#1449 = CARTESIAN_POINT ( 'NONE',  ( -0.2399999999999999079, -1.681985126431739364, -0.3495993037578392637 ) ) ;
#1450 = CARTESIAN_POINT ( 'NONE',  ( 0.1679539120650488104, -1.280520828024429125, 0.4182417262808778013 ) ) ;
#1451 = DIRECTION ( 'NONE',  ( 0.000000000000000000, 0.000000000000000000, -1.000000000000000000 ) ) ;
#1452 = CARTESIAN_POINT ( 'NONE',  ( 0.3364536680357681497, -1.190071269297861889, 0.7177689078920298504 ) ) ;
#1453 = CARTESIAN_POINT ( 'NONE',  ( 0.3204139389452037023, -1.755336229099433654, 0.4849083929475442867 ) ) ;
#1454 = CIRCLE ( 'NONE', #27041, 0.02999999999999998848 ) ;
#1455 = CARTESIAN_POINT ( 'NONE',  ( -0.1553124468364784072, 0.4816356660588179128, 0.3589899338161260944 ) ) ;
#1456 = CARTESIAN_POINT ( 'NONE',  ( 0.2484857473122377980, -1.339293634572156000, -0.5155029497116575543 ) ) ;
#1457 = VECTOR ( 'NONE', #15230, 39.37007874015748854 ) ;
#1458 = CARTESIAN_POINT ( 'NONE',  ( 0.6568730927750874304, -1.460570608776338597, 0.4224083929475443977 ) ) ;
#1459 =( BOUNDED_SURFACE ( )  B_SPLINE_SURFACE ( 3, 2, ( 
 ( #10089, #35198, #16668 ),
 ( #6999, #4506, #1267 ),
 ( #32284, #7600, #19567 ),
 ( #3907, #23263, #16462 ),
 ( #29005, #35581, #20173 ),
 ( #869, #4103, #10308 ),
 ( #29220, #13376, #22874 ),
 ( #35389, #38670, #13771 ),
 ( #7381, #19957, #26334 ),
 ( #33710, #30639, #30213 ),
 ( #23476, #5521, #17271 ),
 ( #39082, #21173, #17866 ) ),
 .UNSPECIFIED., .F., .F., .F. ) 
 B_SPLINE_SURFACE_WITH_KNOTS ( ( 4, 2, 2, 2, 2, 4 ),
 ( 3, 3 ),
 ( 0.001713391272003884783, 0.002288612648294801721, 0.002863834024585718441, 0.003151444712731176802, 0.003439055400876635596, 0.004014276777167552317 ),
 ( 0.000000000000000000, 1.000000000000000000 ),
 .UNSPECIFIED. ) 
 GEOMETRIC_REPRESENTATION_ITEM ( )  RATIONAL_B_SPLINE_SURFACE ( (
 ( 1.000000000000000000, 0.9128709291752516997, 1.000000000000000000),
 ( 1.000000000000000000, 0.9128719127420300561, 1.000000000000000000),
 ( 1.000000000000000000, 0.9128123349199704917, 1.000000000000000000),
 ( 1.000000000000000000, 0.9126095266099195635, 1.000000000000000000),
 ( 1.000000000000000000, 0.9124632789542336253, 1.000000000000000000),
 ( 1.000000000000000000, 0.9122369551432389922, 1.000000000000000000),
 ( 1.000000000000000000, 0.9121592698944432920, 1.000000000000000000),
 ( 1.000000000000000000, 0.9120159902104399974, 1.000000000000000000),
 ( 1.000000000000000000, 0.9119497308967260407, 1.000000000000000000),
 ( 1.000000000000000000, 0.9117802546610581649, 1.000000000000000000),
 ( 1.000000000000000000, 0.9117114107492867436, 1.000000000000000000),
 ( 1.000000000000000000, 0.9117127123830562896, 1.000000000000000000) ) ) 
 REPRESENTATION_ITEM ( '' )  SURFACE ( )  );
#1460 = CIRCLE ( 'NONE', #9981, 0.08749999999977554899 ) ;
#1461 = CARTESIAN_POINT ( 'NONE',  ( 0.000000000000000000, 0.000000000000000000, 0.000000000000000000 ) ) ;
#1462 = FACE_OUTER_BOUND ( 'NONE', #19936, .T. ) ;
#1463 = CARTESIAN_POINT ( 'NONE',  ( -0.2746410161513776482, -2.809880844172510272, -0.2480969101616946892 ) ) ;
#1464 = TOROIDAL_SURFACE ( 'NONE', #25736, 0.5250000000000000222, 0.01499999999999999944 ) ;
#1465 = CARTESIAN_POINT ( 'NONE',  ( 0.06486042810549992599, -1.341249661891149803, 0.5682417262808776570 ) ) ;
#1466 = CYLINDRICAL_SURFACE ( 'NONE', #40215, 0.1000000000000000194 ) ;
#1467 = DIRECTION ( 'NONE',  ( 0.7956551220374296074, 0.4593167559955304569, 0.3949190352937488879 ) ) ;
#1468 = ADVANCED_FACE ( 'NONE', ( #11188 ), #5007, .T. ) ;
#1469 = DIRECTION ( 'NONE',  ( -1.000000000000000000, 0.000000000000000000, -1.138269997360105631E-15 ) ) ;
#1470 = CARTESIAN_POINT ( 'NONE',  ( 0.3996493990393679696, -2.075761934976077860, -0.5159267940723109014 ) ) ;
#1471 = EDGE_CURVE ( 'NONE', #27541, #10276, #3949, .T. ) ;
#1472 = LINE ( 'NONE', #36411, #11914 ) ;
#1473 = EDGE_LOOP ( 'NONE', ( #19177, #35271, #27486, #31971 ) ) ;
#1474 = ORIENTED_EDGE ( 'NONE', *, *, #36700, .F. ) ;
#1475 = CARTESIAN_POINT ( 'NONE',  ( 0.1725857835740884083, -0.5195664690050083578, 0.1686779206399890985 ) ) ;
#1476 = EDGE_LOOP ( 'NONE', ( #31834, #27847, #31710, #25511 ) ) ;
#1477 = EDGE_CURVE ( 'NONE', #26774, #34185, #17752, .T. ) ;
#1478 = CARTESIAN_POINT ( 'NONE',  ( 0.4359176154167935247, -1.577352042444816416, -0.5155029497116575543 ) ) ;
#1479 = CARTESIAN_POINT ( 'NONE',  ( 0.2518471669880268937, -0.8867173105660602905, 0.6889547098528300273 ) ) ;
#1481 = ORIENTED_EDGE ( 'NONE', *, *, #14908, .F. ) ;
#1480 = CARTESIAN_POINT ( 'NONE',  ( -0.002007161383423167276, -0.8507966130668344062, 0.1047852373880929638 ) ) ;
#1482 = ORIENTED_EDGE ( 'NONE', *, *, #38374, .T. ) ;
#1483 = CARTESIAN_POINT ( 'NONE',  ( 0.3565602430104690135, -0.9764240072966976491, 0.8491718633188657384 ) ) ;
#1484 = AXIS2_PLACEMENT_3D ( 'NONE', #17317, #35426, #26381 ) ;
#1485 = ORIENTED_EDGE ( 'NONE', *, *, #25566, .T. ) ;
#1486 = VECTOR ( 'NONE', #8415, 39.37007874015748143 ) ;
#1487 = CARTESIAN_POINT ( 'NONE',  ( 0.1626312629268945875, -1.287482680162472359, 0.9420587295005244943 ) ) ;
#1489 = CARTESIAN_POINT ( 'NONE',  ( 0.4380553862277722921, -1.229819722584721164, 0.5856983068965045947 ) ) ;
#1488 = DIRECTION ( 'NONE',  ( 0.000000000000000000, 0.000000000000000000, 1.000000000000000000 ) ) ;
#1490 = DIRECTION ( 'NONE',  ( 0.8660512985181126888, 0.4999551463232384529, 0.000000000000000000 ) ) ;
#1491 = EDGE_CURVE ( 'NONE', #26219, #3309, #29109, .T. ) ;
#1492 = PERSON_AND_ORGANIZATION_ROLE ( 'classification_officer' ) ;
#1493 = AXIS2_PLACEMENT_3D ( 'NONE', #29081, #19224, #29489 ) ;
#1494 = APPROVAL ( #14613, 'UNKNOWN' ) ;
#1495 = CARTESIAN_POINT ( 'NONE',  ( -0.0006767624898369264692, -0.7404579356088998310, -0.1178596299512801177 ) ) ;
#1497 = ORIENTED_EDGE ( 'NONE', *, *, #8121, .T. ) ;
#1496 = VERTEX_POINT ( 'NONE', #30310 ) ;
#1498 = EDGE_CURVE ( 'NONE', #19084, #27272, #2137, .T. ) ;
#1499 = CARTESIAN_POINT ( 'NONE',  ( 0.1025463942476791679, -0.8285650497785959079, 0.3528706793080363946 ) ) ;
#1500 = DIRECTION ( 'NONE',  ( 1.000000000000000000, 9.860761315262660705E-32, 5.551115123125790098E-17 ) ) ;
#1501 = CARTESIAN_POINT ( 'NONE',  ( 0.09522050325736274023, -0.5826464688574188866, 0.2907231271288692187 ) ) ;
#1502 = CARTESIAN_POINT ( 'NONE',  ( 0.5304122745878165901, -1.471811735070700511, 0.7419010974003765746 ) ) ;
#1503 = DIRECTION ( 'NONE',  ( -0.4999999999999988343, -3.389636702121527438E-32, 0.8660254037844391517 ) ) ;
#1504 = CARTESIAN_POINT ( 'NONE',  ( 0.5919322900404796473, -1.484735096275495048, 0.6354748705596902081 ) ) ;
#1505 = CARTESIAN_POINT ( 'NONE',  ( 0.6114488815859958626, -1.589096688252098266, 0.4246483893745142679 ) ) ;
#1506 = CARTESIAN_POINT ( 'NONE',  ( 1.171686751963009499E-18, 0.2900000000000004796, 0.01749999999999952288 ) ) ;
#1507 = CARTESIAN_POINT ( 'NONE',  ( 0.7427087848590744334, -1.516420150208810380, 0.5553993000885846243 ) ) ;
#1508 = CARTESIAN_POINT ( 'NONE',  ( 0.06805528675573245534, -1.337523170998923927, 0.5185299294045161433 ) ) ;
#1509 = LINE ( 'NONE', #32744, #23175 ) ;
#1510 = DIRECTION ( 'NONE',  ( 0.000000000000000000, 0.9510565162951574170, 0.3090169943749355719 ) ) ;
#1511 = CARTESIAN_POINT ( 'NONE',  ( -3.183539100166564637E-08, -0.6701325942983367145, -0.1152599293596888730 ) ) ;
#1512 = CARTESIAN_POINT ( 'NONE',  ( 0.4584717390208091770, -1.703043547193807017, -0.5155029497116575543 ) ) ;
#1513 = AXIS2_PLACEMENT_3D ( 'NONE', #20014, #1121, #12878 ) ;
#1514 = CARTESIAN_POINT ( 'NONE',  ( 0.4972671625857253974, -1.080199071502573771, 0.5707417262808780478 ) ) ;
#1515 = CARTESIAN_POINT ( 'NONE',  ( 0.07216878364870311924, 0.000000000000000000, 0.1249999999999999029 ) ) ;
#1516 = CARTESIAN_POINT ( 'NONE',  ( 0.09565263806948612335, -1.148840486724431953, 0.8358535653919648700 ) ) ;
#1517 = CARTESIAN_POINT ( 'NONE',  ( 0.4302506758624459748, -1.041368148273517313, 0.6535113357015974733 ) ) ;
#1518 = APPROVAL_DATE_TIME ( #26611, #408 ) ;
#1519 = CARTESIAN_POINT ( 'NONE',  ( 0.6872158423035881203, -1.414036026188038031, 0.8114895833460221697 ) ) ;
#1520 = AXIS2_PLACEMENT_3D ( 'NONE', #4415, #26851, #10804 ) ;
#1521 = CONICAL_SURFACE ( 'NONE', #24503, 0.2000000000000000111, 1.047197551196598964 ) ;
#1522 = EDGE_CURVE ( 'NONE', #36854, #21617, #12209, .T. ) ;
#1523 = DIRECTION ( 'NONE',  ( 0.000000000000000000, 0.000000000000000000, 1.000000000000000000 ) ) ;
#1524 = EDGE_CURVE ( 'NONE', #4497, #13794, #9031, .T. ) ;
#1525 = CARTESIAN_POINT ( 'NONE',  ( 0.3164773456298530796, -1.761773283766707499, 0.5681507431435155464 ) ) ;
#1526 = AXIS2_PLACEMENT_3D ( 'NONE', #1117, #26386, #29051 ) ;
#1527 = VERTEX_POINT ( 'NONE', #11997 ) ;
#1528 = CARTESIAN_POINT ( 'NONE',  ( 0.3187641638634987618, -1.760284878867080183, 0.5597302103697527897 ) ) ;
#1529 = CARTESIAN_POINT ( 'NONE',  ( 0.6413879784614744395, -1.405912376546664122, -0.6250000000000000000 ) ) ;
#1531 = ORIENTED_EDGE ( 'NONE', *, *, #28760, .T. ) ;
#1530 = PLANE ( 'NONE',  #2057 ) ;
#1532 = CARTESIAN_POINT ( 'NONE',  ( 0.3247324306351094814, -1.759421949583082956, 0.4854534786567449300 ) ) ;
#1533 = CARTESIAN_POINT ( 'NONE',  ( 0.3740232550247291066, -0.9210422728154799010, 0.7367171417286558777 ) ) ;
#1535 = VERTEX_POINT ( 'NONE', #33809 ) ;
#1534 = ORIENTED_EDGE ( 'NONE', *, *, #8982, .T. ) ;
#1536 = CARTESIAN_POINT ( 'NONE',  ( 0.04118663679044942683, -1.516485496198475946, -0.6452587487763896679 ) ) ;
#1537 = ORIENTED_EDGE ( 'NONE', *, *, #10931, .T. ) ;
#1538 = ORIENTED_EDGE ( 'NONE', *, *, #36074, .F. ) ;
#1539 = CARTESIAN_POINT ( 'NONE',  ( 0.3545963309600190794, -1.820992936139588458, -0.5160179355990298644 ) ) ;
#1540 = CARTESIAN_POINT ( 'NONE',  ( 0.4471227077962564578, -1.226789242222319443, 0.5945616820347162657 ) ) ;
#1541 = CIRCLE ( 'NONE', #35666, 0.07999999999999996003 ) ;
#1542 = CARTESIAN_POINT ( 'NONE',  ( -0.04945776359515308140, 0.4635931069071607125, -0.1136454792236678418 ) ) ;
#1543 = EDGE_LOOP ( 'NONE', ( #19547, #20953, #31883, #36639 ) ) ;
#1544 = CARTESIAN_POINT ( 'NONE',  ( 0.6089330441038812713, -1.477473485466218150, -0.6250000000000000000 ) ) ;
#1545 = CARTESIAN_POINT ( 'NONE',  ( 0.1008403764883030462, -0.6728090870223089048, 0.3368761478404066478 ) ) ;
#1546 = CIRCLE ( 'NONE', #6765, 0.06000000000000038636 ) ;
#1547 = CARTESIAN_POINT ( 'NONE',  ( 0.2596705996059036070, -1.501196151453698668, 1.012645528602832856 ) ) ;
#1548 = CIRCLE ( 'NONE', #38959, 0.5302738246768106123 ) ;
#1549 = CARTESIAN_POINT ( 'NONE',  ( 0.4477263009981874986, -1.446915290368048224, 0.8103176498262139038 ) ) ;
#1551 = CARTESIAN_POINT ( 'NONE',  ( 0.3845608912840868254, -1.768804211478402166, -0.5723197561600831262 ) ) ;
#1550 = CARTESIAN_POINT ( 'NONE',  ( 0.2327167355993654541, -1.504842320349070173, 0.9206877750890873902 ) ) ;
#1552 = CARTESIAN_POINT ( 'NONE',  ( 0.06016085808641227078, -0.9698831199938917624, 0.4410261798063859207 ) ) ;
#1553 = ORIENTED_EDGE ( 'NONE', *, *, #33349, .F. ) ;
#1554 = EDGE_CURVE ( 'NONE', #32680, #3626, #26230, .T. ) ;
#1555 = CARTESIAN_POINT ( 'NONE',  ( 0.3702380742285729109, -1.615333040638610385, 0.5482224031604636671 ) ) ;
#1556 = CARTESIAN_POINT ( 'NONE',  ( 0.1894921497020525258, -0.4689065141878340226, 0.2178402233697973867 ) ) ;
#1557 = CARTESIAN_POINT ( 'NONE',  ( -0.03171102739523626313, 0.2433685106468593262, -0.4273977451499059166 ) ) ;
#1558 = CARTESIAN_POINT ( 'NONE',  ( -0.04087116408466984208, -0.4547130927580663173, -0.1255914340181775168 ) ) ;
#1559 = CARTESIAN_POINT ( 'NONE',  ( -0.2399999999999999079, -3.286568920421631290, -0.5766864829451954222 ) ) ;
#1560 = CARTESIAN_POINT ( 'NONE',  ( -0.2267371898560517907, -0.4872893062166330780, 0.3599999999999990430 ) ) ;
#1561 = CARTESIAN_POINT ( 'NONE',  ( 0.4444209036527600465, -1.039833579653637319, 0.7404771872114588316 ) ) ;
#1562 = CARTESIAN_POINT ( 'NONE',  ( -0.02000000000000000042, -1.910390638264138685, -0.7420407338378623985 ) ) ;
#1563 = AXIS2_PLACEMENT_3D ( 'NONE', #2879, #40310, #12140 ) ;
#1564 = CARTESIAN_POINT ( 'NONE',  ( 0.03025752215418233901, -1.950362531980313285, -0.3012757290405999044 ) ) ;
#1565 = CARTESIAN_POINT ( 'NONE',  ( 0.5454473090585744144, -1.628634442125448167, -0.5828508516191583944 ) ) ;
#1566 = ORIENTED_EDGE ( 'NONE', *, *, #14670, .F. ) ;
#1567 = CARTESIAN_POINT ( 'NONE',  ( 0.4358230120647305084, -1.191225622903871351, 0.6736421652573473251 ) ) ;
#1568 = CARTESIAN_POINT ( 'NONE',  ( -0.2399999999999999079, -3.941790907013290823, -0.4709369376873030477 ) ) ;
#1569 = CARTESIAN_POINT ( 'NONE',  ( -0.04140212552917830330, -0.2901315858634276323, -0.3705031754532651656 ) ) ;
#1570 = VECTOR ( 'NONE', #27657, 39.37007874015748143 ) ;
#1571 = AXIS2_PLACEMENT_3D ( 'NONE', #639, #13130, #37 ) ;
#1572 = ORIENTED_EDGE ( 'NONE', *, *, #32786, .F. ) ;
#1573 = CARTESIAN_POINT ( 'NONE',  ( 0.4856540751714051862, -1.094772563176381830, 0.7053893588296803463 ) ) ;
#1574 = CARTESIAN_POINT ( 'NONE',  ( -0.04293694706340299427, 0.07181688488226835310, -0.4893579783149998308 ) ) ;
#1575 = CARTESIAN_POINT ( 'NONE',  ( -0.1399999999999997358, 7.160938508832261116E-17, 0.2149999999999999967 ) ) ;
#1576 = VECTOR ( 'NONE', #24035, 39.37007874015748143 ) ;
#1577 = CARTESIAN_POINT ( 'NONE',  ( 0.04904889558162006669, -0.8792800190827789741, 0.4846422760073311187 ) ) ;
#1578 = ORIENTED_EDGE ( 'NONE', *, *, #32895, .F. ) ;
#1579 = CARTESIAN_POINT ( 'NONE',  ( 0.4334739817046469601, -1.659740982267900566, -0.5155029497116575543 ) ) ;
#1580 = VECTOR ( 'NONE', #3908, 39.37007874015748143 ) ;
#1581 = CARTESIAN_POINT ( 'NONE',  ( 0.04047170147976712068, 0.06272069502581248401, 0.4973236590858390316 ) ) ;
#1582 = CARTESIAN_POINT ( 'NONE',  ( -0.08000000000000000167, -2.367354784411275670, -0.3586747285825516718 ) ) ;
#1583 = FACE_OUTER_BOUND ( 'NONE', #20207, .T. ) ;
#1584 = CARTESIAN_POINT ( 'NONE',  ( 0.4366927577353089118, -1.195111805554035289, 0.6938221743858382640 ) ) ;
#1586 = FACE_BOUND ( 'NONE', #30002, .T. ) ;
#1585 = DIRECTION ( 'NONE',  ( -7.771561172376107616E-16, 7.170354002788761615E-17, -1.000000000000000000 ) ) ;
#1587 = CARTESIAN_POINT ( 'NONE',  ( 0.5839362087672538282, -1.507072137279306334, -0.5885553949852400102 ) ) ;
#1588 = VERTEX_POINT ( 'NONE', #2741 ) ;
#1589 = DIRECTION ( 'NONE',  ( -1.387778780781449225E-15, 6.590151126658375938E-16, -1.000000000000000000 ) ) ;
#1590 = ORIENTED_EDGE ( 'NONE', *, *, #28286, .F. ) ;
#1591 = CARTESIAN_POINT ( 'NONE',  ( 0.1879010291930788001, -0.5477411782657776174, -0.08446770797961487831 ) ) ;
#1592 = CARTESIAN_POINT ( 'NONE',  ( 0.3562885538576506250, -1.448602233765710956, 0.8591113950276315636 ) ) ;
#1594 = CARTESIAN_POINT ( 'NONE',  ( -0.02000000000000000042, -2.402843508890908808, -0.4070539641574215106 ) ) ;
#1593 = CARTESIAN_POINT ( 'NONE',  ( 0.08794147700442006554, -0.6552000505539613551, 0.02671434475884571294 ) ) ;
#1595 = CARTESIAN_POINT ( 'NONE',  ( 0.1338345669307856312, -1.289664158897918078, 0.4854672773588690204 ) ) ;
#1596 = ORIENTED_EDGE ( 'NONE', *, *, #30272, .F. ) ;
#1597 = AXIS2_PLACEMENT_3D ( 'NONE', #16856, #4483, #25702 ) ;
#1598 = EDGE_LOOP ( 'NONE', ( #11770, #35184, #34446, #21254 ) ) ;
#1599 = FACE_OUTER_BOUND ( 'NONE', #24496, .T. ) ;
#1600 = CARTESIAN_POINT ( 'NONE',  ( 0.1211351843104187254, -0.5779263820291693499, 0.2644342070444274939 ) ) ;
#1601 = ORIENTED_EDGE ( 'NONE', *, *, #39876, .T. ) ;
#1602 = CARTESIAN_POINT ( 'NONE',  ( 0.3900356592778671527, -1.754097070625186605, -0.4603106969345188149 ) ) ;
#1603 = CARTESIAN_POINT ( 'NONE',  ( 0.04157078424165398800, -0.4522175634759056373, 0.1290209392672012623 ) ) ;
#1604 = VECTOR ( 'NONE', #18659, 39.37007874015748143 ) ;
#1605 = AXIS2_PLACEMENT_3D ( 'NONE', #26518, #23239, #32679 ) ;
#1606 = CARTESIAN_POINT ( 'NONE',  ( 0.6257246952511709148, -1.577931829754174009, 0.4224971546942883904 ) ) ;
#1607 = PRODUCT_DEFINITION_SHAPE ( 'NONE', 'NONE',  #40666 ) ;
#1608 = CARTESIAN_POINT ( 'NONE',  ( 0.1322978751951766341, -1.279211731145868169, 0.4318426636282766129 ) ) ;
#1609 = CARTESIAN_POINT ( 'NONE',  ( 0.1889603646001475068, -0.5843802352234823694, 0.2966845687057266812 ) ) ;
#1610 = ADVANCED_FACE ( 'NONE', ( #37094 ), #21785, .T. ) ;
#1611 = CARTESIAN_POINT ( 'NONE',  ( 0.05634304521267755744, 1.092739197465705287E-15, 0.4588823192046724841 ) ) ;
#1612 = EDGE_CURVE ( 'NONE', #8537, #36494, #9278, .T. ) ;
#1613 = CARTESIAN_POINT ( 'NONE',  ( 0.6712941330769894854, -1.387165532388958678, 0.7909734157804186871 ) ) ;
#1614 = TOROIDAL_SURFACE ( 'NONE', #8160, 0.04999999999999998196, 0.1700000000000000400 ) ;
#1615 = CARTESIAN_POINT ( 'NONE',  ( 0.3992403239432529283, -1.683235622436187073, -0.6263438071736542323 ) ) ;
#1616 = CARTESIAN_POINT ( 'NONE',  ( 0.01548846960721238578, -0.2450655194478977839, -0.4674710490746283864 ) ) ;
#1617 = CARTESIAN_POINT ( 'NONE',  ( 0.6009539617556340918, -1.596610001391108868, -0.5128529812280162581 ) ) ;
#1618 = CARTESIAN_POINT ( 'NONE',  ( 0.03875523708677762469, 0.3062771359410750294, 0.3649060648845446897 ) ) ;
#1619 = CARTESIAN_POINT ( 'NONE',  ( 0.1840595033465176056, -0.8547675690073376353, 0.1457166466292989515 ) ) ;
#1620 = CARTESIAN_POINT ( 'NONE',  ( 0.6839214307796153136, -1.445693534907656508, 0.4790777032679445213 ) ) ;
#1621 = CARTESIAN_POINT ( 'NONE',  ( -0.05283102792148821475, 0.4560693389104576445, -0.1064538768721981082 ) ) ;
#1622 = ADVANCED_FACE ( 'NONE', ( #22196, #34912, #19684 ), #34711, .T. ) ;
#1623 = APPLIED_PERSON_AND_ORGANIZATION_ASSIGNMENT ( #9489, #38268, ( #35397 ) ) ;
#1624 = CARTESIAN_POINT ( 'NONE',  ( -0.01548846960707517956, -0.4638115001430989648, -0.2459753896937853235 ) ) ;
#1625 = CARTESIAN_POINT ( 'NONE',  ( 0.5750311553790389274, -1.568077294875266814, -0.4484120973757802497 ) ) ;
#1626 = VECTOR ( 'NONE', #16951, 39.37007874015748854 ) ;
#1627 = DIRECTION ( 'NONE',  ( -7.771561172376107616E-16, 7.170354002788761615E-17, -1.000000000000000000 ) ) ;
#1628 = PLANE ( 'NONE',  #7464 ) ;
#1629 = CARTESIAN_POINT ( 'NONE',  ( -0.04087116408466998779, -0.2599586249408754601, 0.3936479624527436383 ) ) ;
#1630 = AXIS2_PLACEMENT_3D ( 'NONE', #12113, #9417, #27354 ) ;
#1631 = ORIENTED_EDGE ( 'NONE', *, *, #33062, .F. ) ;
#1632 = AXIS2_PLACEMENT_3D ( 'NONE', #32854, #17232, #37557 ) ;
#1633 = EDGE_LOOP ( 'NONE', ( #22929, #38455, #14161, #25594 ) ) ;
#1634 = CARTESIAN_POINT ( 'NONE',  ( 0.4670822870386998060, -1.088164015307882648, -0.6212900150988791559 ) ) ;
#1635 = AXIS2_PLACEMENT_3D ( 'NONE', #14109, #1980, #14502 ) ;
#1636 = CARTESIAN_POINT ( 'NONE',  ( 0.4697228370620195048, -1.442521976758482261, -0.5166151207188711680 ) ) ;
#1637 = ORIENTED_EDGE ( 'NONE', *, *, #23407, .T. ) ;
#1638 = PLANE ( 'NONE',  #9915 ) ;
#1639 = CARTESIAN_POINT ( 'NONE',  ( 0.02953079040095519733, 0.2329676531120528360, -0.4763574306556333515 ) ) ;
#1640 = CARTESIAN_POINT ( 'NONE',  ( 0.3828956050899013919, -1.120133131850320263, 0.7911315793847942812 ) ) ;
#1642 = ORIENTED_EDGE ( 'NONE', *, *, #21732, .F. ) ;
#1641 = CARTESIAN_POINT ( 'NONE',  ( -0.02953079040095639429, 0.4684706630666118365, 0.2484463060367366194 ) ) ;
#1643 = CARTESIAN_POINT ( 'NONE',  ( 0.4820398931871337500, -1.088803207145679242, 0.6894399345265510570 ) ) ;
#1644 = CIRCLE ( 'NONE', #37731, 0.04500000000000022038 ) ;
#1645 = CYLINDRICAL_SURFACE ( 'NONE', #34216, 0.2500000000000000000 ) ;
#1646 = VERTEX_POINT ( 'NONE', #9408 ) ;
#1647 = CARTESIAN_POINT ( 'NONE',  ( 0.1734973056165642902, -1.209394307038482497, -0.5155029497116575543 ) ) ;
#1648 = B_SPLINE_CURVE_WITH_KNOTS ( 'NONE', 3,
 ( #2160, #36510, #8321, #14086, #39194, #4417, #23574, #36093 ),
 .UNSPECIFIED., .F., .F.,
 ( 4, 2, 2, 4 ),
 ( 0.0005881714484888330569, 0.001255587419990853576, 0.001589295405741864486, 0.001923003391492875396 ),
 .UNSPECIFIED. ) ;
#1649 = CARTESIAN_POINT ( 'NONE',  ( 0.05844364294462878889, -0.7327107322325441263, 0.5805734399641627741 ) ) ;
#1651 = CARTESIAN_POINT ( 'NONE',  ( 0.1153571302060458353, -0.4466443244026027659, 0.1507141667401463714 ) ) ;
#1650 = CARTESIAN_POINT ( 'NONE',  ( 0.7040907193196406233, -1.491292208824496424, 0.5118938265934908083 ) ) ;
#1652 = CARTESIAN_POINT ( 'NONE',  ( 0.2469141422421070875, -1.581573626495411444, -0.3511777555542848206 ) ) ;
#1653 = FACE_OUTER_BOUND ( 'NONE', #6648, .T. ) ;
#1654 = ORIENTED_EDGE ( 'NONE', *, *, #30058, .T. ) ;
#1655 = DIRECTION ( 'NONE',  ( 0.000000000000000000, 0.000000000000000000, -1.000000000000000000 ) ) ;
#1656 = CARTESIAN_POINT ( 'NONE',  ( 0.1581650021276241880, -1.285700486175305857, 0.4182417262808778013 ) ) ;
#1657 = EDGE_CURVE ( 'NONE', #16708, #39344, #7950, .T. ) ;
#1658 = CARTESIAN_POINT ( 'NONE',  ( 0.3696433394773024350, -2.076155315806792245, -0.5157937231490886676 ) ) ;
#1659 = CARTESIAN_POINT ( 'NONE',  ( 0.4375190507963158115, -1.228364410370137660, 0.5956955845658383764 ) ) ;
#1660 = CARTESIAN_POINT ( 'NONE',  ( 0.1364676818254310919, -1.302864912412562193, -0.3444472864111620125 ) ) ;
#1661 = AXIS2_PLACEMENT_3D ( 'NONE', #1295, #17698, #1893 ) ;
#1662 = EDGE_CURVE ( 'NONE', #12973, #30547, #29671, .T. ) ;
#1663 = CARTESIAN_POINT ( 'NONE',  ( 0.5201389011762601600, -1.665685209299224923, -0.5911274130876347233 ) ) ;
#1664 = EDGE_CURVE ( 'NONE', #32520, #27730, #38877, .T. ) ;
#1665 = AXIS2_PLACEMENT_3D ( 'NONE', #15901, #31142, #34625 ) ;
#1666 = EDGE_CURVE ( 'NONE', #15505, #9243, #3654, .T. ) ;
#1667 = CARTESIAN_POINT ( 'NONE',  ( 0.2876584704904820433, -1.030801853274127655, 0.6172218215535044683 ) ) ;
#1668 = CARTESIAN_POINT ( 'NONE',  ( 0.01548846960707524721, 0.000000000000000000, 0.000000000000000000 ) ) ;
#1669 = CARTESIAN_POINT ( 'NONE',  ( 0.3484900513549475942, -1.166308394724161479, 0.4314524459101332643 ) ) ;
#1670 = DIRECTION ( 'NONE',  ( 0.000000000000000000, 0.000000000000000000, -1.000000000000000000 ) ) ;
#1671 = CARTESIAN_POINT ( 'NONE',  ( 0.01548846960707524721, 0.000000000000000000, 0.000000000000000000 ) ) ;
#1672 = PERSON_AND_ORGANIZATION_ROLE ( 'design_owner' ) ;
#1673 = APPROVAL_PERSON_ORGANIZATION ( #5738, #30299, #39475 ) ;
#1674 = CARTESIAN_POINT ( 'NONE',  ( 0.06449607379900242077, -1.337176272736496419, 0.5902663767274672901 ) ) ;
#1675 = CARTESIAN_POINT ( 'NONE',  ( 0.3125627377754333081, -1.533273879788720429, -0.7004264455586597382 ) ) ;
#1676 = CIRCLE ( 'NONE', #32502, 0.02999999999999998848 ) ;
#1677 = DIRECTION ( 'NONE',  ( -0.4999551463232385085, 0.8660512985181127998, 0.000000000000000000 ) ) ;
#1678 = EDGE_CURVE ( 'NONE', #14515, #30753, #28548, .T. ) ;
#1679 = CARTESIAN_POINT ( 'NONE',  ( 0.01204616690667267322, -0.4657357789976088180, 0.01148779890123117695 ) ) ;
#1680 = CARTESIAN_POINT ( 'NONE',  ( 0.4051926429175483624, -1.104840550354867279, 0.6011831493249744085 ) ) ;
#1681 = CARTESIAN_POINT ( 'NONE',  ( 0.3112618463733268781, -1.738655945234965916, 0.7427334498521994677 ) ) ;
#1682 = CARTESIAN_POINT ( 'NONE',  ( 0.03868264068766629621, -0.03360988006411996798, -0.4753775160315163451 ) ) ;
#1683 = ORIENTED_EDGE ( 'NONE', *, *, #13917, .F. ) ;
#1684 = ORIENTED_EDGE ( 'NONE', *, *, #33671, .F. ) ;
#1685 = CARTESIAN_POINT ( 'NONE',  ( 0.1764830872386634331, -0.4886048756821292915, 0.1725546913697795504 ) ) ;
#1686 = ORIENTED_EDGE ( 'NONE', *, *, #35073, .T. ) ;
#1687 = CARTESIAN_POINT ( 'NONE',  ( 0.4710977142973246656, -1.661186711027922813, -0.4170720528719246700 ) ) ;
#1688 = AXIS2_PLACEMENT_3D ( 'NONE', #11790, #24347, #12399 ) ;
#1689 = CARTESIAN_POINT ( 'NONE',  ( 0.1347597814052855225, -0.5521900656507784388, 0.1611950669615822840 ) ) ;
#1691 = EDGE_LOOP ( 'NONE', ( #7815, #26358, #7067, #6159 ) ) ;
#1690 = CARTESIAN_POINT ( 'NONE',  ( -0.001169249310984843589, -0.7938970875308333230, 0.02649849479796821672 ) ) ;
#1692 = CIRCLE ( 'NONE', #24682, 0.2149999999999999967 ) ;
#1693 = EDGE_LOOP ( 'NONE', ( #37648, #3502, #33966, #10993 ) ) ;
#1694 = CARTESIAN_POINT ( 'NONE',  ( 0.1787515287242018858, -0.6558014035218070470, 0.6057541867068507724 ) ) ;
#1695 = EDGE_LOOP ( 'NONE', ( #23782, #30098, #37718, #33340 ) ) ;
#1696 = DIRECTION ( 'NONE',  ( 0.3468893892380782717, 0.9373665302208757932, 0.03180785525163551397 ) ) ;
#1698 = CARTESIAN_POINT ( 'NONE',  ( 0.1897596718690655326, -1.237814093943444993, 0.5863089767353449888 ) ) ;
#1697 = DIRECTION ( 'NONE',  ( 0.8660512985181135770, 0.4999551463232371207, 0.000000000000000000 ) ) ;
#1699 = LOCAL_TIME ( 0, 53, 7.000000000000000000, #931 ) ;
#1700 = CARTESIAN_POINT ( 'NONE',  ( 0.4409062655693438137, -1.690090444797295977, -0.2869361388274795921 ) ) ;
#1701 = APPROVAL_STATUS ( 'not_yet_approved' ) ;
#1702 = CARTESIAN_POINT ( 'NONE',  ( 0.1934290844966307377, -1.261396119720670894, -0.7137149802747378979 ) ) ;
#1704 = EDGE_LOOP ( 'NONE', ( #564, #37325, #6115, #12602 ) ) ;
#1703 = VERTEX_POINT ( 'NONE', #12916 ) ;
#1705 = CARTESIAN_POINT ( 'NONE',  ( 0.1744008153849919973, -0.8797694432983949042, 0.5730610230391658400 ) ) ;
#1706 = CARTESIAN_POINT ( 'NONE',  ( 0.3984114568195520345, -1.599003643269838904, -0.5155029497116575543 ) ) ;
#1707 = EDGE_CURVE ( 'NONE', #755, #34098, #23755, .T. ) ;
#1708 = CARTESIAN_POINT ( 'NONE',  ( 0.1350056248402534687, -0.6996330933666771168, 0.5045168804572850441 ) ) ;
#1709 =( BOUNDED_SURFACE ( )  B_SPLINE_SURFACE ( 3, 2, ( 
 ( #33947, #12337, #5747 ),
 ( #18305, #30845, #2667 ),
 ( #15210, #27765, #12132 ),
 ( #6148, #24894, #18712 ) ),
 .UNSPECIFIED., .F., .F., .F. ) 
 B_SPLINE_SURFACE_WITH_KNOTS ( ( 4, 4 ),
 ( 3, 3 ),
 ( -1.734723475976807094E-18, 0.0003263618124877773626 ),
 ( 0.000000000000000000, 1.000000000000000000 ),
 .UNSPECIFIED. ) 
 GEOMETRIC_REPRESENTATION_ITEM ( )  RATIONAL_B_SPLINE_SURFACE ( (
 ( 1.000000000000000000, 0.7071496063340664273, 1.000000000000000000),
 ( 1.000000000000000000, 0.7071209263092794739, 1.000000000000000000),
 ( 1.000000000000000000, 0.7071067771900807486, 1.000000000000000000),
 ( 1.000000000000000000, 0.7071067811865479058, 1.000000000000000000) ) ) 
 REPRESENTATION_ITEM ( '' )  SURFACE ( )  );
#1710 = CARTESIAN_POINT ( 'NONE',  ( 0.5529922410844849701, -1.511190678568866241, 0.5733929733483635882 ) ) ;
#1711 = CARTESIAN_POINT ( 'NONE',  ( 0.05177553688007868748, -1.201125113761218666, 0.6644015224960638788 ) ) ;
#1712 = CARTESIAN_POINT ( 'NONE',  ( 0.6068955179909718556, -1.480486077813617962, 0.5781976481189164963 ) ) ;
#1713 = FACE_OUTER_BOUND ( 'NONE', #20602, .T. ) ;
#1714 = EDGE_CURVE ( 'NONE', #30709, #1646, #24190, .T. ) ;
#1715 = CARTESIAN_POINT ( 'NONE',  ( 0.3927316539789887928, -1.706278926685924180, -0.4292189291772694482 ) ) ;
#1716 = DIRECTION ( 'NONE',  ( 0.000000000000000000, 0.000000000000000000, -1.000000000000000000 ) ) ;
#1717 = EDGE_CURVE ( 'NONE', #15843, #7929, #5984, .T. ) ;
#1718 = CARTESIAN_POINT ( 'NONE',  ( -0.2300000000000000655, 0.5182417262804733804, 0.3749999999999999445 ) ) ;
#1719 = CARTESIAN_POINT ( 'NONE',  ( 0.3699999999999788458, -2.097675824466504135, -0.4688691127277798687 ) ) ;
#1720 = CARTESIAN_POINT ( 'NONE',  ( -0.02000000000000000042, -1.845925619402022155, -0.3444148183989317880 ) ) ;
#1721 = CARTESIAN_POINT ( 'NONE',  ( -0.0003523642967645715515, -0.9220156720689431928, 0.06121834490154719893 ) ) ;
#1722 = CARTESIAN_POINT ( 'NONE',  ( -0.3000000000000000999, -3.672249662662566472, -0.1880352225538197142 ) ) ;
#1723 = EDGE_CURVE ( 'NONE', #28841, #5281, #13390, .T. ) ;
#1724 = DIRECTION ( 'NONE',  ( -0.4999551463232377313, 0.8660512985181132439, -0.000000000000000000 ) ) ;
#1725 = CLOSED_SHELL ( 'NONE', ( #33113, #19688, #19693, #4680, #14913, #20218, #17239, #25799, #22608, #34827, #37384, #3758, #25606 ) ) ;
#1726 = AXIS2_PLACEMENT_3D ( 'NONE', #29057, #3157, #25789 ) ;
#1727 = DIRECTION ( 'NONE',  ( 0.000000000000000000, 3.414809992080317289E-15, -1.000000000000000000 ) ) ;
#1728 = CARTESIAN_POINT ( 'NONE',  ( 0.02199361096923483153, -0.8343928545013460374, 0.5934276300867008525 ) ) ;
#1729 = CARTESIAN_POINT ( 'NONE',  ( 0.4556897805969272741, -1.061013212638954206, 0.6517789979982376858 ) ) ;
#1730 = PERSON_AND_ORGANIZATION ( #28500, #32463 ) ;
#1731 = CARTESIAN_POINT ( 'NONE',  ( 0.6221473432577675489, -1.308691071842436493, 0.8644659521288400317 ) ) ;
#1732 = ADVANCED_FACE ( 'NONE', ( #23607 ), #35570, .T. ) ;
#1733 = LOCAL_TIME ( 0, 53, 7.000000000000000000, #28823 ) ;
#1734 = EDGE_CURVE ( 'NONE', #38697, #13940, #14122, .T. ) ;
#1735 = EDGE_CURVE ( 'NONE', #36909, #24607, #37427, .T. ) ;
#1736 = CARTESIAN_POINT ( 'NONE',  ( 0.4112193008908943126, -1.591609915475965975, -0.6177460231409253044 ) ) ;
#1737 = AXIS2_PLACEMENT_3D ( 'NONE', #2008, #13918, #35950 ) ;
#1738 = CARTESIAN_POINT ( 'NONE',  ( 0.3110797536664995366, -1.761551355401022700, 0.5692323052624194135 ) ) ;
#1739 = EDGE_CURVE ( 'NONE', #13108, #10835, #35506, .T. ) ;
#1740 = VERTEX_POINT ( 'NONE', #4250 ) ;
#1741 = CARTESIAN_POINT ( 'NONE',  ( 0.2999999999999791167, -2.097675824466505023, -0.7286991843995648255 ) ) ;
#1742 = CARTESIAN_POINT ( 'NONE',  ( 0.1259012050209226963, -1.123654620964547934, 0.8919649897266007654 ) ) ;
#1743 = CARTESIAN_POINT ( 'NONE',  ( -2.112273405726188513E-14, -2.107936428766274073, -0.2870436526301869962 ) ) ;
#1745 = EDGE_LOOP ( 'NONE', ( #12346, #3380, #15937, #13795 ) ) ;
#1744 = CARTESIAN_POINT ( 'NONE',  ( -0.3000000000000000999, -4.134278792318540674, -0.4999285807449073693 ) ) ;
#1746 = CARTESIAN_POINT ( 'NONE',  ( 0.06450940144326640369, -1.331203771656425561, 0.5682439549991663563 ) ) ;
#1747 = B_SPLINE_CURVE_WITH_KNOTS ( 'NONE', 3,
 ( #30685, #33971, #27192, #26977, #39513, #20618 ),
 .UNSPECIFIED., .F., .F.,
 ( 4, 2, 4 ),
 ( 0.000000000000000000, 0.5000000000000000000, 1.000000000000000000 ),
 .UNSPECIFIED. ) ;
#1748 = CARTESIAN_POINT ( 'NONE',  ( 0.6179353394495007423, -1.299228382567916285, 0.5682417262808777680 ) ) ;
#1750 = EDGE_LOOP ( 'NONE', ( #8435, #16528, #28992, #34357 ) ) ;
#1749 = VERTEX_POINT ( 'NONE', #29551 ) ;
#1751 = CARTESIAN_POINT ( 'NONE',  ( 0.06561571374232599840, -1.525176766320938793, -0.6748652540125912314 ) ) ;
#1752 = VERTEX_POINT ( 'NONE', #23419 ) ;
#1753 = FACE_BOUND ( 'NONE', #18113, .T. ) ;
#1754 = CARTESIAN_POINT ( 'NONE',  ( 0.5660458073529762713, -1.502436908615445210, 0.5399521221014897954 ) ) ;
#1755 = DATE_TIME_ROLE ( 'classification_date' ) ;
#1756 = CARTESIAN_POINT ( 'NONE',  ( -0.03874953289575077536, 0.4622846869243777967, -0.1151793484519217925 ) ) ;
#1757 = ORIENTED_EDGE ( 'NONE', *, *, #5929, .T. ) ;
#1758 = CARTESIAN_POINT ( 'NONE',  ( 0.1831772843670138040, -1.238081160791867585, 0.5906532873403225192 ) ) ;
#1759 = CARTESIAN_POINT ( 'NONE',  ( 0.1200222707058349603, -0.7080646023026895275, 0.4423028072555330592 ) ) ;
#1760 = CARTESIAN_POINT ( 'NONE',  ( 0.1261966868762690042, -0.9842092163644554637, 0.9331960565778399941 ) ) ;
#1761 = CARTESIAN_POINT ( 'NONE',  ( 0.09811070749329325880, -0.5560036527972357367, 0.2112130360183118449 ) ) ;
#1763 = CARTESIAN_POINT ( 'NONE',  ( 0.1614670899430008522, -0.7569536277469717245, 0.1022936816274460647 ) ) ;
#1762 = CARTESIAN_POINT ( 'NONE',  ( 0.2276870189180398851, -1.487426405742815261, 0.9274550246884837312 ) ) ;
#1764 = CARTESIAN_POINT ( 'NONE',  ( 0.09375000000000006939, -0.9316581899787153009, 0.1457185332388701571 ) ) ;
#1765 = LOCAL_TIME ( 0, 53, 7.000000000000000000, #18162 ) ;
#1766 = VERTEX_POINT ( 'NONE', #8142 ) ;
#1767 = ORIENTED_EDGE ( 'NONE', *, *, #6638, .T. ) ;
#1768 = ADVANCED_FACE ( 'NONE', ( #7314 ), #37523, .T. ) ;
#1769 = LINE ( 'NONE', #39976, #14748 ) ;
#1770 = CARTESIAN_POINT ( 'NONE',  ( 0.1207008425007928681, -0.4921100478383975685, 0.3258471659695452161 ) ) ;
#1771 = EDGE_CURVE ( 'NONE', #6171, #3151, #4037, .T. ) ;
#1772 = AXIS2_PLACEMENT_3D ( 'NONE', #6632, #19208, #37715 ) ;
#1773 = CARTESIAN_POINT ( 'NONE',  ( 0.3690965330173307524, -1.099411688709415413, 0.5182417262812423209 ) ) ;
#1774 = CARTESIAN_POINT ( 'NONE',  ( -0.05616044724337262289, -0.4399661196824186660, -0.1321902923858476464 ) ) ;
#1775 = DIRECTION ( 'NONE',  ( 0.000000000000000000, 0.000000000000000000, -1.000000000000000000 ) ) ;
#1776 = CARTESIAN_POINT ( 'NONE',  ( 0.3911589123679613533, -1.952241739367067019, -0.4946140563714283567 ) ) ;
#1777 = CARTESIAN_POINT ( 'NONE',  ( -0.2399999999999999079, -2.853330612949663170, -0.6088139570729240724 ) ) ;
#1778 = CARTESIAN_POINT ( 'NONE',  ( 0.5633629393321837320, -1.208205391268785567, 0.7270432621192387534 ) ) ;
#1779 = DIRECTION ( 'NONE',  ( 1.000000000000000000, 0.000000000000000000, 7.702990362679453920E-16 ) ) ;
#1780 = DIRECTION ( 'NONE',  ( 1.000000000000000000, 0.000000000000000000, 0.000000000000000000 ) ) ;
#1781 = AXIS2_PLACEMENT_3D ( 'NONE', #3964, #35439, #38321 ) ;
#1782 = CARTESIAN_POINT ( 'NONE',  ( 0.05999999999999990757, 0.000000000000000000, 0.06250000000000000000 ) ) ;
#1783 = DIRECTION ( 'NONE',  ( 1.000000000000000000, 0.000000000000000000, 0.000000000000000000 ) ) ;
#1784 = CARTESIAN_POINT ( 'NONE',  ( -0.04087116408467055678, -0.2940498268759209055, -0.3688792544161150766 ) ) ;
#1785 = APPLIED_APPROVAL_ASSIGNMENT ( #40187, ( #31348 ) ) ;
#1786 = VERTEX_POINT ( 'NONE', #32826 ) ;
#1787 = CARTESIAN_POINT ( 'NONE',  ( 0.3880044884704604846, -0.9770951376028897961, 0.6894504840255317735 ) ) ;
#1788 = CARTESIAN_POINT ( 'NONE',  ( 0.2629665421248923995, -1.157745397434066126, -0.5155029497116575543 ) ) ;
#1789 = AXIS2_PLACEMENT_3D ( 'NONE', #39012, #32830, #4255 ) ;
#1790 = CARTESIAN_POINT ( 'NONE',  ( 0.1759864516496214559, -1.107502683655886555, 0.7499173190827560509 ) ) ;
#1791 = ORIENTED_EDGE ( 'NONE', *, *, #14862, .F. ) ;
#1792 = DIRECTION ( 'NONE',  ( 1.702140497302368477E-12, 0.9510565162951575280, 0.3090169943749354053 ) ) ;
#1793 = LINE ( 'NONE', #29534, #34193 ) ;
#1794 = CARTESIAN_POINT ( 'NONE',  ( 0.1949582633045185420, -1.370042541011457837, 0.4186407401730019018 ) ) ;
#1795 = DIRECTION ( 'NONE',  ( 0.000000000000000000, 0.000000000000000000, 1.000000000000000000 ) ) ;
#1796 = CARTESIAN_POINT ( 'NONE',  ( 0.4667596051884817521, -1.235694863872689897, 0.6085114794545928296 ) ) ;
#1798 = FACE_OUTER_BOUND ( 'NONE', #5960, .T. ) ;
#1797 = CARTESIAN_POINT ( 'NONE',  ( 0.01548846960707524721, -0.09319974324249266640, -0.5318964258758781538 ) ) ;
#1799 = CARTESIAN_POINT ( 'NONE',  ( -0.04582713223189553015, -0.2312054150958152143, -0.4285473768184985821 ) ) ;
#1800 = ORIENTED_EDGE ( 'NONE', *, *, #35811, .F. ) ;
#1801 = DIRECTION ( 'NONE',  ( 0.000000000000000000, 1.000000000000000000, -3.330669073875470607E-16 ) ) ;
#1802 = VERTEX_POINT ( 'NONE', #11047 ) ;
#1803 = CARTESIAN_POINT ( 'NONE',  ( -0.3000000000000000999, -2.183180860297908144, -0.4937760292030871079 ) ) ;
#1804 = CARTESIAN_POINT ( 'NONE',  ( 0.06137814430738681298, -0.5595901097020826720, 0.2438590846621483677 ) ) ;
#1806 = CARTESIAN_POINT ( 'NONE',  ( 0.4644259937802360239, -1.101352082929256682, -0.6430948353041650023 ) ) ;
#1805 = CARTESIAN_POINT ( 'NONE',  ( 0.08985841505820577058, -0.5644647999051150000, 0.1403608567123640904 ) ) ;
#1807 = CARTESIAN_POINT ( 'NONE',  ( 0.1499999999999996614, -0.07651041855118867474, 0.5222379212568208917 ) ) ;
#1808 = ORIENTED_EDGE ( 'NONE', *, *, #14754, .F. ) ;
#1809 = AXIS2_PLACEMENT_3D ( 'NONE', #3737, #19972, #22678 ) ;
#1810 = DIRECTION ( 'NONE',  ( 1.000000000000000000, 1.443840457432242888E-15, -8.336459783983783483E-16 ) ) ;
#1811 = CARTESIAN_POINT ( 'NONE',  ( 0.5739652476806176296, -1.499266104267773736, 0.5740897328662426524 ) ) ;
#1812 = ORIENTED_EDGE ( 'NONE', *, *, #32828, .T. ) ;
#1813 = CYLINDRICAL_SURFACE ( 'NONE', #34915, 0.06250000000000000000 ) ;
#1814 = FACE_OUTER_BOUND ( 'NONE', #20604, .T. ) ;
#1815 = CARTESIAN_POINT ( 'NONE',  ( 0.4023438766660552557, -1.746991767930276884, -0.4399290715031914933 ) ) ;
#1816 = CARTESIAN_POINT ( 'NONE',  ( 0.1931523484426772019, -1.244006994361245511, 0.4502174690324191042 ) ) ;
#1817 = CARTESIAN_POINT ( 'NONE',  ( 0.07550925375975386933, -1.312278240014781661, 0.4838115075940697118 ) ) ;
#1818 = CARTESIAN_POINT ( 'NONE',  ( -0.3000000000000000999, -2.595429044015121534, -0.5484989581857646623 ) ) ;
#1819 = CARTESIAN_POINT ( 'NONE',  ( 0.2114022633412600827, -0.5658596150412534831, 0.4491712673773823883 ) ) ;
#1820 = CARTESIAN_POINT ( 'NONE',  ( -0.02872242845530502062, 0.2464193076120121673, 0.4721747535844850741 ) ) ;
#1821 = CARTESIAN_POINT ( 'NONE',  ( 0.01548846960707524721, -0.3772621329472692908, -0.3651003739303438911 ) ) ;
#1822 = CARTESIAN_POINT ( 'NONE',  ( 0.5793421593297778394, -1.608008675138359100, -0.4698213068957341476 ) ) ;
#1823 = CARTESIAN_POINT ( 'NONE',  ( 0.04760578872586636312, 0.3171112559587664914, 0.3633058139840091849 ) ) ;
#1824 = DIRECTION ( 'NONE',  ( -1.000000000000000000, 0.000000000000000000, 0.000000000000000000 ) ) ;
#1825 = FACE_OUTER_BOUND ( 'NONE', #35829, .T. ) ;
#1826 = CARTESIAN_POINT ( 'NONE',  ( -0.05083665881509060597, 0.4330284998000940577, -0.1917934360576658004 ) ) ;
#1827 = CARTESIAN_POINT ( 'NONE',  ( 0.3053298862878815467, -1.679825167650452089, 0.8905181393053133165 ) ) ;
#1828 = CARTESIAN_POINT ( 'NONE',  ( 0.5616945454376203184, -1.585497279018332373, -0.5227682507658810707 ) ) ;
#1829 = FACE_OUTER_BOUND ( 'NONE', #8432, .T. ) ;
#1830 = CARTESIAN_POINT ( 'NONE',  ( 0.4677164644732115795, -1.686000531315665407, 0.5767158751130112559 ) ) ;
#1831 = CARTESIAN_POINT ( 'NONE',  ( -0.05138886601528206560, -0.2591656398409012962, 0.3946081992295803476 ) ) ;
#1832 = ORIENTED_EDGE ( 'NONE', *, *, #38175, .F. ) ;
#1833 = ORIENTED_EDGE ( 'NONE', *, *, #32015, .F. ) ;
#1834 = DIRECTION ( 'NONE',  ( 0.000000000000000000, -1.000000000000000000, 3.330669073875470607E-16 ) ) ;
#1835 = CARTESIAN_POINT ( 'NONE',  ( 0.05579155178881651383, -1.335540925555324332, 0.3667417262808778111 ) ) ;
#1836 = EDGE_LOOP ( 'NONE', ( #37686, #13941, #13062, #14876, #26572, #22028 ) ) ;
#1837 = DIRECTION ( 'NONE',  ( 7.771561172376107616E-16, -7.170354002788761615E-17, 1.000000000000000000 ) ) ;
#1838 = CARTESIAN_POINT ( 'NONE',  ( 0.5092908111800726889, -1.308897765795846713, 0.6930370963245210403 ) ) ;
#1840 = VERTEX_POINT ( 'NONE', #1013 ) ;
#1839 = CARTESIAN_POINT ( 'NONE',  ( -0.03650581953630665372, 0.4542932396444838705, 0.2355374485430446752 ) ) ;
#1841 = CARTESIAN_POINT ( 'NONE',  ( 0.4299297405268334149, -1.031605064505895619, 0.6882246241152528698 ) ) ;
#1842 = CARTESIAN_POINT ( 'NONE',  ( 0.0006049580205936592146, -1.952245379408770187, -0.3315140204742151320 ) ) ;
#1843 = ORIENTED_EDGE ( 'NONE', *, *, #4125, .T. ) ;
#1844 = CARTESIAN_POINT ( 'NONE',  ( 0.3224042817241155601, -1.181557111677860705, 0.5668948776571440806 ) ) ;
#1845 = ORIENTED_EDGE ( 'NONE', *, *, #8517, .F. ) ;
#1846 = CARTESIAN_POINT ( 'NONE',  ( 0.3083011426979856973, -1.561450148453558118, 0.8343410752513801265 ) ) ;
#1848 = CARTESIAN_POINT ( 'NONE',  ( -0.02231181081520722254, -0.3551561381230117775, 0.3696296485972567769 ) ) ;
#1847 = CARTESIAN_POINT ( 'NONE',  ( 0.6949609426117219213, -1.492559866762042331, 0.4793319850971706209 ) ) ;
#1849 = CARTESIAN_POINT ( 'NONE',  ( 0.3208715077212234701, -1.182672892261233732, 0.4687417262808780127 ) ) ;
#1850 = CARTESIAN_POINT ( 'NONE',  ( 0.3699999999999786793, -2.107936428766273185, -0.7005084057759870531 ) ) ;
#1851 = ORIENTED_EDGE ( 'NONE', *, *, #15422, .F. ) ;
#1852 = ORIENTED_EDGE ( 'NONE', *, *, #676, .F. ) ;
#1853 = CARTESIAN_POINT ( 'NONE',  ( 0.02934857795850940448, -1.577273124788314052, -0.6407384231926183116 ) ) ;
#1854 = CARTESIAN_POINT ( 'NONE',  ( 0.04155248107635919896, 0.4416604393009538887, 0.1616214326753678820 ) ) ;
#1855 = CARTESIAN_POINT ( 'NONE',  ( 0.1552519097254527192, -0.9561661948719739623, 0.6628835997166871996 ) ) ;
#1856 = CARTESIAN_POINT ( 'NONE',  ( -2.112273405726188513E-14, -2.104526171302527171, -0.6992671735679987233 ) ) ;
#1857 = APPLIED_DATE_AND_TIME_ASSIGNMENT ( #26080, #22379, ( #28638 ) ) ;
#1858 = DIRECTION ( 'NONE',  ( -1.000000000000000000, -1.450080480853946466E-15, 8.188689774234050758E-16 ) ) ;
#1859 = DIRECTION ( 'NONE',  ( -1.000000000000000000, 0.000000000000000000, 0.000000000000000000 ) ) ;
#1860 = CARTESIAN_POINT ( 'NONE',  ( 0.01548846960706677829, 0.2306506793134169842, 0.4716198300880505845 ) ) ;
#1861 = CARTESIAN_POINT ( 'NONE',  ( 0.04293701532779498065, 0.2295363440003037880, -0.4381116105132950023 ) ) ;
#1862 = CARTESIAN_POINT ( 'NONE',  ( 0.4199258674957010995, -1.127834923126881606, 0.4949619196504369545 ) ) ;
#1863 = LINE ( 'NONE', #17486, #5565 ) ;
#1864 = APPROVAL_DATE_TIME ( #8604, #32073 ) ;
#1865 = CARTESIAN_POINT ( 'NONE',  ( 0.002683297570301478637, -0.9564051229508913066, 0.3926252623119886875 ) ) ;
#1866 = CARTESIAN_POINT ( 'NONE',  ( 0.4475625759263253678, -1.247751609582666843, 0.6057417262809817737 ) ) ;
#1867 = VECTOR ( 'NONE', #4494, 39.37007874015748854 ) ;
#1868 = DIRECTION ( 'NONE',  ( -7.000205099780314469E-17, -1.000000000000000000, 6.590151126658399604E-16 ) ) ;
#1869 = ADVANCED_FACE ( 'NONE', ( #4632 ), #17208, .F. ) ;
#1870 = CARTESIAN_POINT ( 'NONE',  ( 0.4278413765848551042, -1.120299553241070001, -0.3830631589809550541 ) ) ;
#1871 = CARTESIAN_POINT ( 'NONE',  ( 0.4095694756667743186, -1.742820565356182794, -0.5801262846953157970 ) ) ;
#1872 = CARTESIAN_POINT ( 'NONE',  ( 0.0004750074233420679450, -0.4386152179651120475, 0.1512205247030782573 ) ) ;
#1873 = DIRECTION ( 'NONE',  ( 0.000000000000000000, 0.000000000000000000, -1.000000000000000000 ) ) ;
#1874 = VERTEX_POINT ( 'NONE', #4841 ) ;
#1875 = EDGE_CURVE ( 'NONE', #24616, #4342, #9961, .T. ) ;
#1876 = VERTEX_POINT ( 'NONE', #17413 ) ;
#1877 = CARTESIAN_POINT ( 'NONE',  ( 0.1903419785339184878, -0.5326379394093359032, 0.2481619417568516339 ) ) ;
#1878 = EDGE_LOOP ( 'NONE', ( #12193, #13404, #40416, #34916 ) ) ;
#1879 = CARTESIAN_POINT ( 'NONE',  ( -0.08000000000000000167, -1.682484669133182953, -0.03683853088544705029 ) ) ;
#1880 = EDGE_CURVE ( 'NONE', #2643, #40111, #16828, .T. ) ;
#1881 = CARTESIAN_POINT ( 'NONE',  ( 0.3434118854289890943, -1.064821506014568708, 0.7872763406766211114 ) ) ;
#1882 = EDGE_CURVE ( 'NONE', #13458, #18110, #25067, .T. ) ;
#1883 = B_SPLINE_CURVE_WITH_KNOTS ( 'NONE', 3,
 ( #33216, #14474, #4211, #24362, #5630, #27650 ),
 .UNSPECIFIED., .F., .F.,
 ( 4, 2, 4 ),
 ( 0.000000000000000000, 0.0001845344150746688959, 0.0003690688301493377918 ),
 .UNSPECIFIED. ) ;
#1885 = VERTEX_POINT ( 'NONE', #40016 ) ;
#1884 = CARTESIAN_POINT ( 'NONE',  ( 0.007864899693521575086, -0.7290558150142686378, -0.007045877879649726193 ) ) ;
#1886 = EDGE_CURVE ( 'NONE', #38792, #40536, #8353, .T. ) ;
#1887 = VERTEX_POINT ( 'NONE', #5453 ) ;
#1888 = CARTESIAN_POINT ( 'NONE',  ( 0.3175383896200173472, -1.184309477189361415, 0.5626414999152751228 ) ) ;
#1889 = ORIENTED_EDGE ( 'NONE', *, *, #34629, .F. ) ;
#1890 = CARTESIAN_POINT ( 'NONE',  ( 0.2711658269972071489, -1.669704017044846278, 0.6768845942166327179 ) ) ;
#1892 = CARTESIAN_POINT ( 'NONE',  ( 0.1507440847924569616, -1.242487625469949952, 0.6036539243957432799 ) ) ;
#1891 = DIRECTION ( 'NONE',  ( 0.4999999999999973910, -0.6123724356957970238, 0.6123724356957940262 ) ) ;
#1893 = DIRECTION ( 'NONE',  ( 0.8660512985181134660, 0.4999551463232372872, 0.000000000000000000 ) ) ;
#1894 = APPROVAL_STATUS ( 'not_yet_approved' ) ;
#1895 = DIRECTION ( 'NONE',  ( 0.4999999999999973910, 0.000000000000000000, -0.8660254037844402619 ) ) ;
#1897 = ORIENTED_EDGE ( 'NONE', *, *, #31877, .F. ) ;
#1896 = ORIENTED_EDGE ( 'NONE', *, *, #23810, .F. ) ;
#1898 = CARTESIAN_POINT ( 'NONE',  ( 0.01147012505024846800, -0.8931644348827614266, -0.01216302941885656977 ) ) ;
#1899 = CARTESIAN_POINT ( 'NONE',  ( 0.1186103394390872201, -1.414144848331978510, 0.5683298932114988489 ) ) ;
#1900 = CARTESIAN_POINT ( 'NONE',  ( 0.07548269292739374914, -0.5857035475933982660, 0.3081389644222882196 ) ) ;
#1901 = CARTESIAN_POINT ( 'NONE',  ( 0.000000000000000000, 0.000000000000000000, 0.000000000000000000 ) ) ;
#1902 = EDGE_CURVE ( 'NONE', #26889, #39656, #5328, .T. ) ;
#1903 = CARTESIAN_POINT ( 'NONE',  ( -2.119743302583864240E-14, -2.104521498059988449, -0.6992654726654029540 ) ) ;
#1904 = CARTESIAN_POINT ( 'NONE',  ( 0.05990572404004890911, -1.332677842034995397, 0.5606126620464084720 ) ) ;
#1905 = APPLIED_DATE_AND_TIME_ASSIGNMENT ( #3566, #9935, ( #27300 ) ) ;
#1906 = LINE ( 'NONE', #32944, #29878 ) ;
#1907 = PLANE ( 'NONE',  #16629 ) ;
#1908 = FACE_OUTER_BOUND ( 'NONE', #14660, .T. ) ;
#1909 = CARTESIAN_POINT ( 'NONE',  ( -0.1795773455677913688, 0.4580325878418424757, 0.3606502365332823201 ) ) ;
#1910 = SPHERICAL_SURFACE ( 'NONE', #38995, 0.01499999999999999944 ) ;
#1911 = CARTESIAN_POINT ( 'NONE',  ( 0.4183850207828535006, -1.104805702410075030, 0.5963159008084065738 ) ) ;
#1912 = CARTESIAN_POINT ( 'NONE',  ( 0.3445219659096331322, -1.630113034086819290, -0.4330379103484555126 ) ) ;
#1913 = CARTESIAN_POINT ( 'NONE',  ( -0.2399999999999999079, -2.183180860297908144, -0.4937760292030871079 ) ) ;
#1914 = CARTESIAN_POINT ( 'NONE',  ( 0.1180550382625277506, -1.031362315377588157, 0.9291368297579983837 ) ) ;
#1915 = CARTESIAN_POINT ( 'NONE',  ( 0.3170172301852910435, -0.9601440561661597206, 0.5902234374070133294 ) ) ;
#1916 = PERSON_AND_ORGANIZATION_ROLE ( 'creator' ) ;
#1917 = CARTESIAN_POINT ( 'NONE',  ( 0.4045891740076953402, -0.9484829520717948936, 0.8148132024759134895 ) ) ;
#1918 = CARTESIAN_POINT ( 'NONE',  ( 0.3950057241659845064, -1.613548743562832843, -0.6688636923212416541 ) ) ;
#1919 = CARTESIAN_POINT ( 'NONE',  ( 0.04760578872586464921, -0.04300259564631973147, -0.4803138972568000153 ) ) ;
#1920 = EDGE_CURVE ( 'NONE', #38229, #35870, #10603, .T. ) ;
#1921 = ORIENTED_EDGE ( 'NONE', *, *, #21052, .T. ) ;
#1922 = CARTESIAN_POINT ( 'NONE',  ( 0.3540349203463854511, -1.725807860701394691, -0.5334517722040031940 ) ) ;
#1923 = CARTESIAN_POINT ( 'NONE',  ( 0.05974118262646924138, -0.8876447553630215648, 0.7647173577216134222 ) ) ;
#1924 = EDGE_CURVE ( 'NONE', #18554, #15872, #4049, .T. ) ;
#1925 = CARTESIAN_POINT ( 'NONE',  ( 0.2006210498355077976, -1.239694361563377534, 0.4577691556116682547 ) ) ;
#1927 = ORIENTED_EDGE ( 'NONE', *, *, #27088, .F. ) ;
#1926 = CARTESIAN_POINT ( 'NONE',  ( 0.3853296036239867162, -1.884128910060018702, -0.4867200447654468354 ) ) ;
#1928 = FACE_OUTER_BOUND ( 'NONE', #12187, .T. ) ;
#1929 = EDGE_CURVE ( 'NONE', #20340, #5616, #30164, .T. ) ;
#1930 =( REPRESENTATION_RELATIONSHIP ('NONE','NONE', #27514, #7794 ) REPRESENTATION_RELATIONSHIP_WITH_TRANSFORMATION ( #35418 )SHAPE_REPRESENTATION_RELATIONSHIP( ) );
#1931 = CARTESIAN_POINT ( 'NONE',  ( 0.5718426945711908571, -1.221126421150759755, 0.7198242229513793777 ) ) ;
#1933 = ORIENTED_EDGE ( 'NONE', *, *, #14710, .F. ) ;
#1932 = VERTEX_POINT ( 'NONE', #17804 ) ;
#1934 = CARTESIAN_POINT ( 'NONE',  ( 0.09888984647273572903, -1.356722515137474439, -0.6730291679367702562 ) ) ;
#1935 =( BOUNDED_SURFACE ( )  B_SPLINE_SURFACE ( 2, 3, ( 
 ( #1866, #24474, #30441, #21183, #20794, #21407, #36613, #40293, #26946, #30220, #2268, #14809, #27372, #33942, #33315 ),
 ( #5121, #39478, #30838, #5742, #14588, #27156, #11523, #11718, #24275, #15201, #27760, #36798, #8608, #23668, #5531 ),
 ( #25292, #31653, #28775, #6745, #24691, #3078, #18492, #25077, #12125, #37222, #28574, #37832, #21795, #40509, #37611 ),
 ( #34329, #18919, #6140, #2865, #15413, #28169, #27970, #34940, #19115, #3474, #15621, #9648, #9435, #6347, #28365 ),
 ( #9040, #31861, #21602, #12332, #16029, #31263, #5927, #33, #22013, #6539, #19323, #34125, #24889, #451, #34538 ) ),
 .UNSPECIFIED., .F., .F., .F. ) 
 B_SPLINE_SURFACE_WITH_KNOTS ( ( 3, 2, 3 ),
 ( 4, 3, 2, 2, 2, 2, 4 ),
 ( -0.01000000000000000021, 0.000000000000000000, 1.000000000000000000 ),
 ( -0.2248845959520953119, -0.1024158528858618994, -0.002066484013594062884, 0.001425941394020094344, 0.9981093185551406233, 1.001427204709084418, 1.101776573581352281 ),
 .UNSPECIFIED. ) 
 GEOMETRIC_REPRESENTATION_ITEM ( )  RATIONAL_B_SPLINE_SURFACE ( (
 ( 1.000000000000000000, 1.000000000000000000, 1.000000000000000000, 1.000000000000000000, 1.000000000000000000, 1.000000000000000000, 1.000000000000000000, 1.000000000000000000, 1.000000000000000000, 1.000000000000000000, 1.000000000000000000, 1.000000000000000000, 1.000000000000000000, 1.000000000000000000, 1.000000000000000000),
 ( 1.000000000000000000, 1.000000000000000000, 1.000000000000000000, 1.000000000000000000, 1.000000000000000000, 1.000000000000000000, 1.000000000000000000, 1.000000000000000000, 1.000000000000000000, 1.000000000000000000, 1.000000000000000000, 1.000000000000000000, 1.000000000000000000, 1.000000000000000000, 1.000000000000000000),
 ( 1.000000000000000000, 1.000000000000000000, 1.000000000000000000, 1.000000000000000000, 1.000000000000000000, 1.000000000000000000, 1.000000000000000000, 1.000000000000000000, 1.000000000000000000, 1.000000000000000000, 1.000000000000000000, 1.000000000000000000, 1.000000000000000000, 1.000000000000000000, 1.000000000000000000),
 ( 0.7063388106193552174, 0.7063388106193552174, 0.7063388106193552174, 0.7063388106193552174, 0.7063388106193552174, 0.7063388106193546623, 0.7063388106193546623, 0.7063388106193546623, 0.7063388106193546623, 0.7063388106193546623, 0.7063388106193546623, 0.7063388106193552174, 0.7063388106193552174, 0.7063388106193552174, 0.7063388106193552174),
 ( 1.000000000000000000, 1.000000000000000000, 1.000000000000000000, 1.000000000000000000, 1.000000000000000000, 1.000000000000000000, 1.000000000000000000, 1.000000000000000000, 1.000000000000000000, 1.000000000000000000, 1.000000000000000000, 1.000000000000000000, 1.000000000000000000, 1.000000000000000000, 1.000000000000000000) ) ) 
 REPRESENTATION_ITEM ( '' )  SURFACE ( )  );
#1936 = EDGE_LOOP ( 'NONE', ( #36678, #33675, #17468, #17857 ) ) ;
#1937 = CARTESIAN_POINT ( 'NONE',  ( -0.2399999999999999079, -3.701811653776600597, -0.3192834175180689904 ) ) ;
#1938 = CARTESIAN_POINT ( 'NONE',  ( 0.5640895105453352931, -1.503407492374277510, 0.5358556994421860287 ) ) ;
#1939 = SECURITY_CLASSIFICATION_LEVEL ( 'unclassified' ) ;
#1940 = CARTESIAN_POINT ( 'NONE',  ( -0.01548846960707442842, 0.4730347584886794854, -0.2341461249029804237 ) ) ;
#1941 = ORIENTED_EDGE ( 'NONE', *, *, #6752, .F. ) ;
#1942 = CARTESIAN_POINT ( 'NONE',  ( 0.1091017126209868487, -1.269603009439766339, 0.6006954958647061638 ) ) ;
#1943 = CARTESIAN_POINT ( 'NONE',  ( 0.1981269588659515801, -0.8717101755341865044, 0.6257585543226611424 ) ) ;
#1944 = CARTESIAN_POINT ( 'NONE',  ( 0.3109746253762922796, -1.659824283146108748, 0.9017776097172691685 ) ) ;
#1945 = CARTESIAN_POINT ( 'NONE',  ( 0.1509521914015893862, -0.7534614311450832380, 0.5756042479487297747 ) ) ;
#1947 = DIRECTION ( 'NONE',  ( -1.000000000000000000, -1.138269997360102279E-15, 1.138269997360102279E-15 ) ) ;
#1946 = CARTESIAN_POINT ( 'NONE',  ( 0.5923833459584677552, -1.600710257484702970, 0.4291951338990673825 ) ) ;
#1948 = ADVANCED_FACE ( 'NONE', ( #40219 ), #24210, .T. ) ;
#1949 = CARTESIAN_POINT ( 'NONE',  ( 0.06950777349364366253, -1.183310629122789503, 0.6632153050984169740 ) ) ;
#1950 = EDGE_LOOP ( 'NONE', ( #15524, #18844, #37509, #37294, #24907, #13662, #26137, #12030, #33143, #33196, #16859 ) ) ;
#1951 = ORIENTED_EDGE ( 'NONE', *, *, #22792, .F. ) ;
#1952 = CARTESIAN_POINT ( 'NONE',  ( 0.02953079040095687308, -0.4684706630666107263, -0.2484463060367401721 ) ) ;
#1953 = CARTESIAN_POINT ( 'NONE',  ( 0.3545037818611191383, -0.8523828408883230567, 0.7589984277719855621 ) ) ;
#1954 = DIRECTION ( 'NONE',  ( 0.8660512985181134660, 0.4999551463232372317, 0.000000000000000000 ) ) ;
#1955 = CARTESIAN_POINT ( 'NONE',  ( 0.3699999999999786793, -2.080203412138651231, -0.4693458302813933170 ) ) ;
#1956 = DIRECTION ( 'NONE',  ( 0.8660512985181142431, 0.4999551463232357884, 0.000000000000000000 ) ) ;
#1957 = CARTESIAN_POINT ( 'NONE',  ( 0.08352889633857743523, -1.314305457479380879, 0.4727645997108643749 ) ) ;
#1958 = B_SPLINE_CURVE_WITH_KNOTS ( 'NONE', 3,
 ( #24339, #9293, #9509, #15073, #6000, #27438, #8900, #36868, #21662, #30713, #21258, #12587, #34608, #24946, #40155, #18782, #27830, #6411, #33996, #2729, #31335, #34400, #6214, #5801, #8683, #21872, #33795, #37688, #30906, #34189, #30507, #18359, #3139, #18567, #5602, #2338, #15680, #15276, #14877, #39962, #31121, #2535, #15492, #25149, #2935, #12198, #28043, #11985 ),
 .UNSPECIFIED., .F., .F.,
 ( 4, 2, 2, 2, 2, 2, 2, 2, 2, 2, 2, 2, 2, 2, 2, 2, 2, 2, 2, 2, 2, 2, 2, 4 ),
 ( 0.004590105785999735490, 0.006718271026485181721, 0.008846436266970628820, 0.01097460150745607765, 0.01310276674794152649, 0.01523093198842697185, 0.01735909722891242069, 0.01948726246939787299, 0.02161542770988332182, 0.02374359295036877066, 0.02587175819085422296, 0.02693584081109693870, 0.02799992343133965791, 0.03012808867182510675, 0.03119217129206782249, 0.03225625391231053823, 0.03332033653255325745, 0.03385237784267460665, 0.03438441915279595584, 0.03544850177303865424, 0.03651258439328135263, 0.03757666701352405797, 0.03810870832364541411, 0.03864074963376676330 ),
 .UNSPECIFIED. ) ;
#1959 = CARTESIAN_POINT ( 'NONE',  ( 0.1816520550910808995, -1.697676133517970420, -0.6833403372426165578 ) ) ;
#1960 = CARTESIAN_POINT ( 'NONE',  ( 0.1087663190456345796, -1.420020949109092934, 0.5260726173889570534 ) ) ;
#1961 = CARTESIAN_POINT ( 'NONE',  ( 0.2980752164830456907, -0.8471807121723260448, 0.6106271213134966125 ) ) ;
#1962 = CARTESIAN_POINT ( 'NONE',  ( 0.03113248654051816583, 0.000000000000000000, 0.000000000000000000 ) ) ;
#1963 = CARTESIAN_POINT ( 'NONE',  ( 0.05360578929985907598, -1.598838039970692737, -0.3436840987125299174 ) ) ;
#1964 = LINE ( 'NONE', #23773, #14684 ) ;
#1965 = ORIENTED_EDGE ( 'NONE', *, *, #30859, .T. ) ;
#1966 = CARTESIAN_POINT ( 'NONE',  ( 0.4257416900749242394, -1.216787901257387228, 0.6459620410871801388 ) ) ;
#1967 = DIRECTION ( 'NONE',  ( -7.000205099780314469E-17, -1.000000000000000000, 6.590151126658399604E-16 ) ) ;
#1968 = CARTESIAN_POINT ( 'NONE',  ( -0.04047161733259861671, -0.3430572239576335503, -0.3654812350069442939 ) ) ;
#1969 = ORIENTED_EDGE ( 'NONE', *, *, #14539, .F. ) ;
#1970 = CARTESIAN_POINT ( 'NONE',  ( 0.3826582672041143329, -0.9717923329141301414, 0.6844662983072338225 ) ) ;
#1971 = EDGE_CURVE ( 'NONE', #17060, #35941, #170, .T. ) ;
#1972 = CYLINDRICAL_SURFACE ( 'NONE', #35085, 0.03000000000000003358 ) ;
#1973 = CARTESIAN_POINT ( 'NONE',  ( 0.2085758075447457227, -1.314883828705479152, 0.6759879400794416293 ) ) ;
#1974 = ORIENTED_EDGE ( 'NONE', *, *, #31902, .F. ) ;
#1975 = CARTESIAN_POINT ( 'NONE',  ( 0.1904911882605962448, -1.371587248428298045, 0.5682417262808803216 ) ) ;
#1976 = DIRECTION ( 'NONE',  ( 0.000000000000000000, 2.986499936241660365E-14, -1.000000000000000000 ) ) ;
#1977 = DIRECTION ( 'NONE',  ( -1.000000000000000000, -0.000000000000000000, -0.000000000000000000 ) ) ;
#1978 = CARTESIAN_POINT ( 'NONE',  ( 0.1799149647795341422, -1.765837058809831106, -0.3253848170194846845 ) ) ;
#1979 = CARTESIAN_POINT ( 'NONE',  ( 0.4441119490203502829, -1.203454984316005616, 0.6735005572665853091 ) ) ;
#1981 = CARTESIAN_POINT ( 'NONE',  ( 0.6540709664215760277, -1.593060928864740156, 0.5182417262812423209 ) ) ;
#1980 = DIRECTION ( 'NONE',  ( 1.000000000000000000, 6.779273404243070203E-32, 4.314083075427408311E-32 ) ) ;
#1982 = CARTESIAN_POINT ( 'NONE',  ( -0.05562144613422698863, -0.2870684680408737144, -0.3605846877396493011 ) ) ;
#1983 = ORIENTED_EDGE ( 'NONE', *, *, #3168, .T. ) ;
#1984 = DIRECTION ( 'NONE',  ( 7.771561172376107616E-16, -7.170354002788761615E-17, 1.000000000000000000 ) ) ;
#1985 = EDGE_LOOP ( 'NONE', ( #6775, #427, #21387, #33252 ) ) ;
#1986 = PERSON ( 'NAUO-PER13', 'UNSPECIFIED', 'UNSPECIFIED', ('UNSPECIFIED'), ('UNSPECIFIED'), ('UNSPECIFIED') ) ;
#1987 = DIRECTION ( 'NONE',  ( 1.000000000000000000, -0.000000000000000000, -0.000000000000000000 ) ) ;
#1988 = CARTESIAN_POINT ( 'NONE',  ( 0.2106021162434502936, -1.038359553320539419, 0.8169558973072331698 ) ) ;
#1990 = CARTESIAN_POINT ( 'NONE',  ( 0.4700898499424847055, -1.130550283242669485, -0.6581804127022372608 ) ) ;
#1989 = CARTESIAN_POINT ( 'NONE',  ( 0.7011468811679719693, -1.538227936001232088, 0.5810316690295218578 ) ) ;
#1991 = CARTESIAN_POINT ( 'NONE',  ( 0.5667833376006989887, -1.501841640556043744, 0.4952036213288417144 ) ) ;
#1992 = ADVANCED_FACE ( 'NONE', ( #20718 ), #173, .T. ) ;
#1993 = ORIENTED_EDGE ( 'NONE', *, *, #40360, .F. ) ;
#1994 = ORIENTED_EDGE ( 'NONE', *, *, #1707, .F. ) ;
#1995 = EDGE_CURVE ( 'NONE', #21929, #1211, #18798, .T. ) ;
#1996 = CARTESIAN_POINT ( 'NONE',  ( 0.03113248654051816583, 0.6410130462957083219, -0.4300623794142590661 ) ) ;
#1997 = CARTESIAN_POINT ( 'NONE',  ( 0.1230184117381799835, -0.5703923235244722223, 0.2416267668379052103 ) ) ;
#1998 = ORIENTED_EDGE ( 'NONE', *, *, #30675, .F. ) ;
#1999 = CARTESIAN_POINT ( 'NONE',  ( 0.3304338600317479613, -1.765066422999553186, 0.5534862069867115819 ) ) ;
#2000 = CARTESIAN_POINT ( 'NONE',  ( 0.04762035657658240939, -0.4700462218748481802, 0.1075639008183879169 ) ) ;
#2001 = CARTESIAN_POINT ( 'NONE',  ( 0.6008383320827431762, -1.595119844626816885, 0.4182417262808776903 ) ) ;
#2002 = CARTESIAN_POINT ( 'NONE',  ( 0.09068171474054860515, -1.314855571806884615, 0.4630352297835350073 ) ) ;
#2003 = AXIS2_PLACEMENT_3D ( 'NONE', #6309, #19071, #16200 ) ;
#2004 = CARTESIAN_POINT ( 'NONE',  ( 0.07070506769835151195, -1.314942671243113814, 0.5018317509599571347 ) ) ;
#2005 = LINE ( 'NONE', #29983, #10863 ) ;
#2006 = CARTESIAN_POINT ( 'NONE',  ( 0.1927581100858387075, -0.5042345029781482024, 0.3213135115051561908 ) ) ;
#2007 = AXIS2_PLACEMENT_3D ( 'NONE', #25307, #15827, #37845 ) ;
#2008 = CARTESIAN_POINT ( 'NONE',  ( 0.01548846960707524721, -0.3772621329472692908, -0.3651003739303438911 ) ) ;
#2009 = CARTESIAN_POINT ( 'NONE',  ( 0.01128729522873549510, -0.9461985897320858152, 0.1457185332388702959 ) ) ;
#2010 = CARTESIAN_POINT ( 'NONE',  ( 0.5751363246278207164, -1.612441950723962458, -0.5313468545301665014 ) ) ;
#2011 = CARTESIAN_POINT ( 'NONE',  ( 0.1456664551191460266, -1.333113330760314907, -0.7163645201341654056 ) ) ;
#2012 = FACE_OUTER_BOUND ( 'NONE', #1439, .T. ) ;
#2013 = CARTESIAN_POINT ( 'NONE',  ( -0.08408070219616067820, -0.09959325338431374020, 0.3749999999999987232 ) ) ;
#2014 = CARTESIAN_POINT ( 'NONE',  ( 0.1536596445529301580, -1.277574755431481135, 0.4245438548657214928 ) ) ;
#2015 = CARTESIAN_POINT ( 'NONE',  ( -3.414809992080329023E-17, -0.4300901116921415634, 0.2008512132480425316 ) ) ;
#2016 = CARTESIAN_POINT ( 'NONE',  ( 0.5733332956384830092, -1.543075624777708210, -0.4912759999829157675 ) ) ;
#2017 = DIRECTION ( 'NONE',  ( 0.000000000000000000, 0.000000000000000000, 1.000000000000000000 ) ) ;
#2018 = EDGE_CURVE ( 'NONE', #5177, #14867, #34667, .T. ) ;
#2019 = ORIENTED_EDGE ( 'NONE', *, *, #27363, .F. ) ;
#2020 = DIRECTION ( 'NONE',  ( -1.000000000000000000, -2.341930812374887555E-31, 1.664003471950578127E-31 ) ) ;
#2021 = CARTESIAN_POINT ( 'NONE',  ( 0.4089992519647981384, -1.131314579718122992, 0.3157417262808777658 ) ) ;
#2022 = CARTESIAN_POINT ( 'NONE',  ( 0.1316017208954911588, -1.248059642665102942, 0.5182417262812423209 ) ) ;
#2023 = CARTESIAN_POINT ( 'NONE',  ( -0.03309060444528695577, 0.3730661130945406301, -0.3633899800202425312 ) ) ;
#2024 = CARTESIAN_POINT ( 'NONE',  ( 0.5185792659196485355, -1.323880597841234241, 0.6352211934613883892 ) ) ;
#2025 = CIRCLE ( 'NONE', #13833, 0.1033070866141734268 ) ;
#2027 = VERTEX_POINT ( 'NONE', #13066 ) ;
#2026 = CARTESIAN_POINT ( 'NONE',  ( -0.1631308187679525179, 0.4729065765976191993, 0.1187908002253880019 ) ) ;
#2028 = CARTESIAN_POINT ( 'NONE',  ( 0.4978751173634345939, -1.107738205778658669, 0.6841874689585324409 ) ) ;
#2029 = ORIENTED_EDGE ( 'NONE', *, *, #20334, .T. ) ;
#2030 = EDGE_LOOP ( 'NONE', ( #22026, #38650, #7429 ) ) ;
#2031 = CARTESIAN_POINT ( 'NONE',  ( 0.01041333297898627656, -0.5306758790526455716, 0.1248763267698726892 ) ) ;
#2032 = AXIS2_PLACEMENT_3D ( 'NONE', #7969, #14551, #4482 ) ;
#2033 = CARTESIAN_POINT ( 'NONE',  ( 0.3500362837767272972, -1.585416944253276172, 0.7709133781444270639 ) ) ;
#2035 = CARTESIAN_POINT ( 'NONE',  ( 0.1870390274204316861, -0.5985361199501452178, 0.003541061305677496631 ) ) ;
#2034 = CARTESIAN_POINT ( 'NONE',  ( 0.7066443439621657996, -1.495287734631166598, 0.5281105036456856805 ) ) ;
#2036 = CARTESIAN_POINT ( 'NONE',  ( 0.01548846960712810944, 0.4730347584885798429, -0.2341461249029115899 ) ) ;
#2037 = VECTOR ( 'NONE', #2838, 39.37007874015748854 ) ;
#2038 = EDGE_LOOP ( 'NONE', ( #2765, #36816, #4537, #27383 ) ) ;
#2039 = DIRECTION ( 'NONE',  ( 0.8660512985181130219, 0.4999551463232378978, -6.610988856618928922E-16 ) ) ;
#2040 = CARTESIAN_POINT ( 'NONE',  ( 0.01548846960721296691, 0.4730347584884322942, 0.2341461249027875779 ) ) ;
#2041 = CARTESIAN_POINT ( 'NONE',  ( 0.1142242363313231979, -0.8822466011666808550, 0.5261702761697892861 ) ) ;
#2042 = CARTESIAN_POINT ( 'NONE',  ( 0.1250267426322058117, -1.317120597453650621, -0.3493847494023202271 ) ) ;
#2043 = EDGE_CURVE ( 'NONE', #2067, #2801, #34860, .T. ) ;
#2044 = LINE ( 'NONE', #39277, #16115 ) ;
#2045 = CARTESIAN_POINT ( 'NONE',  ( 0.3865105166509632539, -1.105244162432096999, 0.6295132537179397580 ) ) ;
#2046 = CARTESIAN_POINT ( 'NONE',  ( 0.3067120372624415614, -1.770199942203851240, 0.4177417262808785781 ) ) ;
#2047 = CARTESIAN_POINT ( 'NONE',  ( 0.3433891623868345344, -1.169237029733195543, 0.4282016284639145742 ) ) ;
#2048 = DIRECTION ( 'NONE',  ( 1.000000000000000000, -0.000000000000000000, -0.000000000000000000 ) ) ;
#2049 = COORDINATED_UNIVERSAL_TIME_OFFSET ( 0, 0, .AHEAD. ) ;
#2050 = AXIS2_PLACEMENT_3D ( 'NONE', #40055, #11879, #5712 ) ;
#2051 = CARTESIAN_POINT ( 'NONE',  ( 0.05360726000536972929, -1.265335673192477639, 0.6608739414109141563 ) ) ;
#2052 = CARTESIAN_POINT ( 'NONE',  ( 0.04155248107635842181, -0.4523094957185427312, 0.1288470070525104538 ) ) ;
#2053 = CARTESIAN_POINT ( 'NONE',  ( 2.048885995248197414E-16, 0.2900000000000004796, -5.122214988120493288E-16 ) ) ;
#2054 = AXIS2_PLACEMENT_3D ( 'NONE', #1377, #26869, #7914 ) ;
#2055 = VECTOR ( 'NONE', #31921, 39.37007874015748143 ) ;
#2056 = CARTESIAN_POINT ( 'NONE',  ( 0.3999999739562093981, -2.086702397455008295, -0.5179432086380986178 ) ) ;
#2057 = AXIS2_PLACEMENT_3D ( 'NONE', #31116, #11980, #2530 ) ;
#2058 = CARTESIAN_POINT ( 'NONE',  ( -0.2746410161513779258, -2.511040369707300268, -0.5948468226404902692 ) ) ;
#2059 = CARTESIAN_POINT ( 'NONE',  ( 0.01895494625228225788, 0.07381100255646896868, -0.5147985126481140483 ) ) ;
#2060 = VERTEX_POINT ( 'NONE', #22151 ) ;
#2061 = EDGE_LOOP ( 'NONE', ( #35113, #17797 ) ) ;
#2062 = CARTESIAN_POINT ( 'NONE',  ( 0.1499999999999993561, 0.000000000000000000, 0.000000000000000000 ) ) ;
#2063 = VERTEX_POINT ( 'NONE', #34250 ) ;
#2064 = CARTESIAN_POINT ( 'NONE',  ( 0.4139756487772989768, -1.674437384244100713, -0.3990444774096185143 ) ) ;
#2065 = VERTEX_POINT ( 'NONE', #37959 ) ;
#2067 = VERTEX_POINT ( 'NONE', #18849 ) ;
#2066 = CARTESIAN_POINT ( 'NONE',  ( 0.009065448934498832739, -0.6074849142585841966, 0.009116045154335344555 ) ) ;
#2068 = VERTEX_POINT ( 'NONE', #6669 ) ;
#2069 = DIRECTION ( 'NONE',  ( 1.000000000000000000, 2.341930812374887555E-31, -1.664003471950578127E-31 ) ) ;
#2070 = EDGE_LOOP ( 'NONE', ( #34144, #33477, #18552, #6853, #4350, #3277, #10660 ) ) ;
#2071 = CARTESIAN_POINT ( 'NONE',  ( -0.001578457898017553238, -0.5340257668161403348, 0.1971401768889480544 ) ) ;
#2073 = CARTESIAN_POINT ( 'NONE',  ( 0.1470252489180754740, -1.243555166057507932, 0.6044257298140193191 ) ) ;
#2072 = CARTESIAN_POINT ( 'NONE',  ( 0.5908512823694407334, -1.601569576941602957, 0.4282615004916613399 ) ) ;
#2074 = DIRECTION ( 'NONE',  ( 1.702140497302367467E-12, 0.9510565162951502005, -0.3090169943749580539 ) ) ;
#2075 = SECURITY_CLASSIFICATION_LEVEL ( 'unclassified' ) ;
#2076 = VECTOR ( 'NONE', #25527, 39.37007874015748854 ) ;
#2077 = DIRECTION ( 'NONE',  ( 0.000000000000000000, 0.000000000000000000, 1.000000000000000000 ) ) ;
#2079 = ORIENTED_EDGE ( 'NONE', *, *, #4175, .T. ) ;
#2078 = ORIENTED_EDGE ( 'NONE', *, *, #26556, .T. ) ;
#2080 = CARTESIAN_POINT ( 'NONE',  ( 0.3431906593882065315, -1.156341550885930491, 0.6074911006494660981 ) ) ;
#2081 = CARTESIAN_POINT ( 'NONE',  ( 0.2137282995058389923, -1.231963470009917128, 0.5563255107610510786 ) ) ;
#2082 = CARTESIAN_POINT ( 'NONE',  ( 0.1924812274689710334, -0.8175909794505628048, 0.6368276176361362673 ) ) ;
#2083 = CIRCLE ( 'NONE', #25048, 0.1620173459747806799 ) ;
#2084 = CIRCLE ( 'NONE', #12589, 0.06434668806854085266 ) ;
#2085 = CARTESIAN_POINT ( 'NONE',  ( 0.1871597835675367083, -0.7100598730055870389, 0.03076398055866989140 ) ) ;
#2086 = DIRECTION ( 'NONE',  ( 0.000000000000000000, 0.000000000000000000, -1.000000000000000000 ) ) ;
#2087 = CARTESIAN_POINT ( 'NONE',  ( 0.3211374802916291959, -1.297362887257381026, 0.4402873239467990918 ) ) ;
#2088 = AXIS2_PLACEMENT_3D ( 'NONE', #2924, #2524, #21652 ) ;
#2089 = CARTESIAN_POINT ( 'NONE',  ( 0.3951517471592372877, -1.686279057714856311, -0.4060406207988965788 ) ) ;
#2090 = CARTESIAN_POINT ( 'NONE',  ( 0.3837046737290842335, -1.723330870051356767, 0.4227126563901177358 ) ) ;
#2091 = EDGE_CURVE ( 'NONE', #1239, #34108, #365, .T. ) ;
#2092 = CARTESIAN_POINT ( 'NONE',  ( 0.3699999999999797895, -2.107936428766272741, -0.2870436526301863300 ) ) ;
#2093 = CARTESIAN_POINT ( 'NONE',  ( -0.2746410161513782033, -2.003129936916423048, -0.4197911229995844873 ) ) ;
#2094 = CARTESIAN_POINT ( 'NONE',  ( 0.4314229567236929630, -1.111443131039648868, 0.6061934567595625989 ) ) ;
#2095 = LINE ( 'NONE', #1722, #38440 ) ;
#2096 = EDGE_CURVE ( 'NONE', #33486, #31970, #31672, .T. ) ;
#2097 = DIRECTION ( 'NONE',  ( -1.000000000000000000, 0.000000000000000000, 0.000000000000000000 ) ) ;
#2098 = EDGE_CURVE ( 'NONE', #433, #19840, #12446, .T. ) ;
#2099 = CARTESIAN_POINT ( 'NONE',  ( 0.2190338188766751681, -1.487106827364948147, 0.9008211596871106286 ) ) ;
#2100 = CARTESIAN_POINT ( 'NONE',  ( 0.4790383449168201802, -1.075084602395082634, 0.6124719440393814329 ) ) ;
#2101 = CARTESIAN_POINT ( 'NONE',  ( 0.02769007923577383040, -0.9640067030880757892, 0.6504839076559877364 ) ) ;
#2102 = PERSON_AND_ORGANIZATION ( #28500, #32463 ) ;
#2103 = CARTESIAN_POINT ( 'NONE',  ( 0.4504805333218593333, -1.026900667268108469, 0.8467065612799143937 ) ) ;
#2104 = B_SPLINE_CURVE_WITH_KNOTS ( 'NONE', 3,
 ( #29595, #13952, #30011, #1842, #14358, #11279, #23846, #17652, #14560, #27127, #39657, #39871, #36769, #11691, #30409, #25045, #24245, #40264, #2240, #27533, #27729, #18271, #27342, #15385, #33478, #12097 ),
 .UNSPECIFIED., .F., .F.,
 ( 4, 2, 2, 2, 2, 2, 2, 2, 2, 2, 2, 2, 4 ),
 ( -5.999999999672944161E-08, 0.002879311815431165582, 0.005758683630862327339, 0.008638055446293490397, 0.01151742726172465259, 0.01439679907715581304, 0.01727617089258697697, 0.01871585680030255633, 0.02015554270801813916, 0.02159522861573372199, 0.02231507156959151167, 0.02267499304652039957, 0.02303491452344929094 ),
 .UNSPECIFIED. ) ;
#2105 = AXIS2_PLACEMENT_3D ( 'NONE', #10033, #22605, #6526 ) ;
#2106 = DIRECTION ( 'NONE',  ( 0.000000000000000000, 0.000000000000000000, -1.000000000000000000 ) ) ;
#2107 = CARTESIAN_POINT ( 'NONE',  ( 0.05634206451479396166, -0.01034894336415755935, -0.4588844674656199496 ) ) ;
#2108 = CIRCLE ( 'NONE', #29680, 2.001671648589471442 ) ;
#2109 = AXIS2_PLACEMENT_3D ( 'NONE', #5302, #24081, #30642 ) ;
#2110 = EDGE_CURVE ( 'NONE', #36587, #2842, #34956, .T. ) ;
#2111 = CARTESIAN_POINT ( 'NONE',  ( 0.02999864137222190211, -2.091146312649429628, -0.7263531585133695678 ) ) ;
#2112 = ORIENTED_EDGE ( 'NONE', *, *, #38643, .F. ) ;
#2113 = CARTESIAN_POINT ( 'NONE',  ( 0.03333333333331318926, -1.848796465755284668, -0.6381145059054189606 ) ) ;
#2114 = APPROVAL ( #29283, 'UNSPECIFIED' ) ;
#2115 = CARTESIAN_POINT ( 'NONE',  ( 0.004217272053185415481, -0.5691354127735893664, 0.3239988763902699742 ) ) ;
#2116 = CIRCLE ( 'NONE', #20532, 0.6115209409081865388 ) ;
#2117 = CARTESIAN_POINT ( 'NONE',  ( 0.5553811761775682143, -1.443364489385942306, 0.7462368593144907969 ) ) ;
#2118 = CARTESIAN_POINT ( 'NONE',  ( 0.3853411735685215445, -1.756807109041784054, -0.4499573014714178809 ) ) ;
#2120 = ORIENTED_EDGE ( 'NONE', *, *, #23131, .T. ) ;
#2119 = CARTESIAN_POINT ( 'NONE',  ( 0.3204479958614548929, -1.182666560659948907, 0.5682417262808776570 ) ) ;
#2121 = CARTESIAN_POINT ( 'NONE',  ( 0.04154009738085473469, 0.2902754972779525988, 0.3700679770908117394 ) ) ;
#2122 = CARTESIAN_POINT ( 'NONE',  ( 0.1963745812722482442, -0.6060194383687296238, 0.2878283022669332891 ) ) ;
#2124 = EDGE_LOOP ( 'NONE', ( #13708, #37503, #35908, #38126 ) ) ;
#2123 = VERTEX_POINT ( 'NONE', #19245 ) ;
#2125 = CARTESIAN_POINT ( 'NONE',  ( 0.08989322008881010795, -1.439897079492934440, -0.6871119803270818727 ) ) ;
#2126 = ORIENTED_EDGE ( 'NONE', *, *, #15191, .T. ) ;
#2127 = CARTESIAN_POINT ( 'NONE',  ( 0.01548846960721296691, 0.4730347584884322942, 0.2341461249027875779 ) ) ;
#2128 = CARTESIAN_POINT ( 'NONE',  ( 0.01548846960707511190, 0.09319974324249648279, 0.5318964258758775987 ) ) ;
#2129 = PERSON_AND_ORGANIZATION ( #12765, #26710 ) ;
#2130 = DIRECTION ( 'NONE',  ( 0.000000000000000000, 0.5365213554527465956, -0.8438867430782092116 ) ) ;
#2131 = ORIENTED_EDGE ( 'NONE', *, *, #6660, .T. ) ;
#2132 = DIRECTION ( 'NONE',  ( 0.4999551463232373427, -0.8660512985181134660, 0.000000000000000000 ) ) ;
#2133 = CARTESIAN_POINT ( 'NONE',  ( 0.1125212918553140234, -0.7619884966536627502, 0.4061142703594107228 ) ) ;
#2134 = CARTESIAN_POINT ( 'NONE',  ( 0.2800970862558492813, -1.537244030595081856, 0.9925064799805612958 ) ) ;
#2135 = CARTESIAN_POINT ( 'NONE',  ( 0.4968737439736803374, -1.542313245617131345, 0.5635433591466190162 ) ) ;
#2137 = LINE ( 'NONE', #13852, #9903 ) ;
#2136 = DIRECTION ( 'NONE',  ( -0.4999551463232373427, 0.8660512985181134660, -0.000000000000000000 ) ) ;
#2138 = CARTESIAN_POINT ( 'NONE',  ( 0.01879405481382893928, -0.9579227845311485412, 0.3482156429045401569 ) ) ;
#2139 = ORIENTED_EDGE ( 'NONE', *, *, #18885, .F. ) ;
#2140 = EDGE_LOOP ( 'NONE', ( #29079, #6459, #6924 ) ) ;
#2141 = AXIS2_PLACEMENT_3D ( 'NONE', #5354, #17917, #17532 ) ;
#2142 = B_SPLINE_CURVE_WITH_KNOTS ( 'NONE', 3,
 ( #25681, #221, #436, #16227 ),
 .UNSPECIFIED., .F., .F.,
 ( 4, 4 ),
 ( 4.336808689942155440E-19, 0.0002303018524726754336 ),
 .UNSPECIFIED. ) ;
#2143 = CARTESIAN_POINT ( 'NONE',  ( 0.04293317454820588797, -0.4432234940308283355, -0.2195257349118454882 ) ) ;
#2144 = CARTESIAN_POINT ( 'NONE',  ( 0.3038869664936152959, -0.7554869697991318800, 0.6839101067327857386 ) ) ;
#2145 = EDGE_CURVE ( 'NONE', #25611, #22283, #25747, .T. ) ;
#2146 = DIRECTION ( 'NONE',  ( 1.000000000000000000, -0.000000000000000000, -0.000000000000000000 ) ) ;
#2147 = EDGE_CURVE ( 'NONE', #21815, #23348, #6629, .T. ) ;
#2148 = VECTOR ( 'NONE', #18130, 39.37007874015748143 ) ;
#2149 = CONICAL_SURFACE ( 'NONE', #31709, 0.2000000000000000111, 1.047197551196598964 ) ;
#2150 = CARTESIAN_POINT ( 'NONE',  ( 0.04293701532779389124, -0.4432143466407630350, 0.2195216604697207696 ) ) ;
#2151 = CIRCLE ( 'NONE', #27110, 0.1700000000000001232 ) ;
#2152 = ADVANCED_FACE ( 'NONE', ( #31571 ), #150, .T. ) ;
#2153 = FACE_OUTER_BOUND ( 'NONE', #21960, .T. ) ;
#2154 = CARTESIAN_POINT ( 'NONE',  ( 0.1761599653103556595, -1.266290592972142193, -0.7065742620306031396 ) ) ;
#2155 = EDGE_CURVE ( 'NONE', #39497, #33041, #35155, .T. ) ;
#2156 = CARTESIAN_POINT ( 'NONE',  ( 0.3085271267949294960, -1.189394089994698867, 0.5261560657346352476 ) ) ;
#2157 = CARTESIAN_POINT ( 'NONE',  ( 0.5231597928089396499, -1.148848539795074508, 0.7464108937515090414 ) ) ;
#2158 = PRODUCT_DEFINITION_SHAPE ( 'NONE', 'NONE',  #1177 ) ;
#2159 = PERSON_AND_ORGANIZATION ( #28500, #32463 ) ;
#2160 = CARTESIAN_POINT ( 'NONE',  ( -0.1088121136105144049, -0.4964308608213456875, 0.1000000000000000194 ) ) ;
#2161 = VECTOR ( 'NONE', #163, 39.37007874015748143 ) ;
#2162 = DIRECTION ( 'NONE',  ( 0.000000000000000000, 3.330669073875470114E-16, 1.000000000000000000 ) ) ;
#2163 = ORIENTED_EDGE ( 'NONE', *, *, #12309, .T. ) ;
#2164 = DIRECTION ( 'NONE',  ( -1.000000000000000000, -0.000000000000000000, -0.000000000000000000 ) ) ;
#2165 = FACE_OUTER_BOUND ( 'NONE', #23989, .T. ) ;
#2166 = DIRECTION ( 'NONE',  ( 8.881784197001246407E-16, -2.361472542561082612E-16, 1.000000000000000000 ) ) ;
#2167 = EDGE_CURVE ( 'NONE', #27329, #16906, #31221, .T. ) ;
#2168 = ORIENTED_EDGE ( 'NONE', *, *, #35075, .T. ) ;
#2169 = CARTESIAN_POINT ( 'NONE',  ( 0.2080690969106096522, -0.8521148724087993509, 0.3830115466634239074 ) ) ;
#2170 = AXIS2_PLACEMENT_3D ( 'NONE', #14577, #11708, #27149 ) ;
#2171 = CARTESIAN_POINT ( 'NONE',  ( 0.08509462338391231284, -0.8106601328590971045, 0.1993838098214128496 ) ) ;
#2172 = CARTESIAN_POINT ( 'NONE',  ( 0.2220010284085898178, -1.342657189645787064, 0.6229336649678032245 ) ) ;
#2173 = ORIENTED_EDGE ( 'NONE', *, *, #1498, .T. ) ;
#2174 = CARTESIAN_POINT ( 'NONE',  ( -0.02000000000000000042, -1.723343441215260619, -0.2604803408413784993 ) ) ;
#2175 = CIRCLE ( 'NONE', #13965, 0.01499999999999999598 ) ;
#2176 = CIRCLE ( 'NONE', #3493, 0.4488493849861021068 ) ;
#2177 = CARTESIAN_POINT ( 'NONE',  ( 0.03672447062657722278, 0.04080285735492172883, 0.4790833464420496957 ) ) ;
#2178 = CARTESIAN_POINT ( 'NONE',  ( 0.03647060353175650416, -0.4543627241291142149, -0.2356060312622652864 ) ) ;
#2179 = CARTESIAN_POINT ( 'NONE',  ( 0.1838426283055374921, -1.725872612985020593, -0.3279395879214231924 ) ) ;
#2180 = AXIS2_PLACEMENT_3D ( 'NONE', #37451, #18535, #31091 ) ;
#2181 = CARTESIAN_POINT ( 'NONE',  ( 0.4436287470858775728, -1.200807317510819372, 0.6564808803850732399 ) ) ;
#2183 = CARTESIAN_POINT ( 'NONE',  ( -0.2299999999999999267, 0.5182417262804744906, 0.09999999999999989453 ) ) ;
#2182 = CARTESIAN_POINT ( 'NONE',  ( 0.02953079040095559285, 0.5250338024619285449, 0.07436286310882497808 ) ) ;
#2184 = FACE_OUTER_BOUND ( 'NONE', #27289, .T. ) ;
#2185 = EDGE_LOOP ( 'NONE', ( #16379, #10385, #22146, #8192 ) ) ;
#2186 = CARTESIAN_POINT ( 'NONE',  ( 0.07298619815556110779, -1.313484934506050417, 0.5462077094077502082 ) ) ;
#2187 = VERTEX_POINT ( 'NONE', #28102 ) ;
#2188 = AXIS2_PLACEMENT_3D ( 'NONE', #6580, #28820, #6393 ) ;
#2189 = DIRECTION ( 'NONE',  ( 0.000000000000000000, 0.8159412518334721032, 0.5781348229923762849 ) ) ;
#2190 = CARTESIAN_POINT ( 'NONE',  ( 0.06121954705759836968, -0.5575974508628280812, 0.2378852839864381008 ) ) ;
#2191 = TOROIDAL_SURFACE ( 'NONE', #4167, 0.04500000000000023426, 0.01499999999999999944 ) ;
#2193 = CARTESIAN_POINT ( 'NONE',  ( 5.487288226601811250E-16, -0.2899999999999993694, -0.04250000000000066225 ) ) ;
#2192 = CARTESIAN_POINT ( 'NONE',  ( -0.02953079040095700838, -0.4684706630666085614, 0.2484463060367459175 ) ) ;
#2194 = CARTESIAN_POINT ( 'NONE',  ( 0.5602799925893692246, -1.505597493397644149, 0.5182417262812344383 ) ) ;
#2195 = ORIENTED_EDGE ( 'NONE', *, *, #26046, .F. ) ;
#2196 = ORIENTED_EDGE ( 'NONE', *, *, #11512, .F. ) ;
#2197 = CARTESIAN_POINT ( 'NONE',  ( 0.1993854619498310055, -2.037305861891523850, -0.2781182464799481502 ) ) ;
#2198 = CARTESIAN_POINT ( 'NONE',  ( 0.2691130962247216263, -0.9494530259878606326, 0.7322442259066408443 ) ) ;
#2199 = CARTESIAN_POINT ( 'NONE',  ( 0.5779297624755960205, -1.623152544610868109, 0.5629341535590222101 ) ) ;
#2200 = CARTESIAN_POINT ( 'NONE',  ( 0.3999999999999787059, -2.143549940236731288, -0.4549916158381476228 ) ) ;
#2201 = EDGE_CURVE ( 'NONE', #35465, #5749, #6210, .T. ) ;
#2202 = CARTESIAN_POINT ( 'NONE',  ( -0.02235124290213187995, 0.5044963136724002206, 0.09030809412322121643 ) ) ;
#2203 = DIRECTION ( 'NONE',  ( 0.000000000000000000, 0.3268939817722816832, -0.9450610163799283425 ) ) ;
#2204 = VECTOR ( 'NONE', #7460, 39.37007874015748143 ) ;
#2205 = EDGE_CURVE ( 'NONE', #8583, #9507, #4541, .T. ) ;
#2206 = CARTESIAN_POINT ( 'NONE',  ( 0.3935416462523685932, -1.752073130202900897, -0.5293634714477323255 ) ) ;
#2207 = DIRECTION ( 'NONE',  ( -7.771561172376107616E-16, 7.170354002788761615E-17, -1.000000000000000000 ) ) ;
#2208 = ADVANCED_FACE ( 'NONE', ( #30251 ), #39318, .T. ) ;
#2209 = CARTESIAN_POINT ( 'NONE',  ( 0.3073438066573006555, -0.7730596496961650299, 0.7003458109913517360 ) ) ;
#2210 = AXIS2_PLACEMENT_3D ( 'NONE', #12468, #33663, #30793 ) ;
#2211 = VECTOR ( 'NONE', #12735, 39.37007874015748143 ) ;
#2212 = CARTESIAN_POINT ( 'NONE',  ( -0.2399999999999999079, -2.477126460671948749, -0.4732852368073287574 ) ) ;
#2213 = CARTESIAN_POINT ( 'NONE',  ( -2.194512287980899339E-05, -0.9481927139106636204, 0.1806018079512390906 ) ) ;
#2214 = ADVANCED_FACE ( 'NONE', ( #4741 ), #31310, .T. ) ;
#2215 = CARTESIAN_POINT ( 'NONE',  ( 0.6468257105432076992, -1.563888897256662469, -0.6077625487223605738 ) ) ;
#2216 = DIRECTION ( 'NONE',  ( -0.8593916653663324912, 0.5113178712883813537, 0.000000000000000000 ) ) ;
#2217 = CARTESIAN_POINT ( 'NONE',  ( 0.5775767250843619749, -1.612202439891691652, 0.5714792215281596643 ) ) ;
#2218 = CARTESIAN_POINT ( 'NONE',  ( 0.4100456123093286775, -1.725225710419908243, -0.4268450903248972028 ) ) ;
#2219 = AXIS2_PLACEMENT_3D ( 'NONE', #27051, #33220, #30136 ) ;
#2220 = DIRECTION ( 'NONE',  ( -1.000000000000000000, 0.000000000000000000, 0.000000000000000000 ) ) ;
#2221 = EDGE_CURVE ( 'NONE', #7743, #33803, #18827, .T. ) ;
#2222 = TOROIDAL_SURFACE ( 'NONE', #33740, 0.1699999999999999845, 0.01499999999999999944 ) ;
#2223 = CARTESIAN_POINT ( 'NONE',  ( 0.01054327228848483088, -0.5372198261166355460, 0.4758561573974433023 ) ) ;
#2224 = CARTESIAN_POINT ( 'NONE',  ( 0.4034443304043100476, -1.732073763044814196, -0.5980905150073216880 ) ) ;
#2225 = EDGE_CURVE ( 'NONE', #3536, #15736, #37612, .T. ) ;
#2226 = CARTESIAN_POINT ( 'NONE',  ( 0.1415875073431126230, -1.284922281152920398, 0.5547766581037201217 ) ) ;
#2227 = CARTESIAN_POINT ( 'NONE',  ( 0.6008383320827377361, -1.595119844626803562, 0.4182417262808777458 ) ) ;
#2228 = EDGE_CURVE ( 'NONE', #36405, #9596, #6331, .T. ) ;
#2229 = ORIENTED_EDGE ( 'NONE', *, *, #14727, .F. ) ;
#2230 = CARTESIAN_POINT ( 'NONE',  ( 0.4655516839591847256, -1.068397176280596161, -0.6095936865603254207 ) ) ;
#2231 = CARTESIAN_POINT ( 'NONE',  ( 0.3611552640280384363, -1.125445538258061928, 0.6035644152996554324 ) ) ;
#2232 = CARTESIAN_POINT ( 'NONE',  ( -2.070754768975505034, -0.09959325338431362917, 0.3602693341844379060 ) ) ;
#2233 = VECTOR ( 'NONE', #30402, 39.37007874015748143 ) ;
#2234 = CARTESIAN_POINT ( 'NONE',  ( 0.4557618173848551058, -1.227332695086565506, 0.7391538672619316630 ) ) ;
#2236 = VERTEX_POINT ( 'NONE', #12554 ) ;
#2235 = CARTESIAN_POINT ( 'NONE',  ( -0.2746410161513779258, -2.139295658456680904, -0.3024034539465678129 ) ) ;
#2237 = CARTESIAN_POINT ( 'NONE',  ( 0.4302506758624459748, -1.041368148273517313, 0.6535113357015974733 ) ) ;
#2238 = ORIENTED_EDGE ( 'NONE', *, *, #1554, .F. ) ;
#2239 = B_SPLINE_CURVE_WITH_KNOTS ( 'NONE', 3,
 ( #30247, #33529, #24504, #5339 ),
 .UNSPECIFIED., .F., .F.,
 ( 4, 4 ),
 ( 5.011996131622145663E-14, 7.281930351775003953E-08 ),
 .UNSPECIFIED. ) ;
#2240 = CARTESIAN_POINT ( 'NONE',  ( 0.1353039243655410340, -1.303414152582186736, -0.3416695301304896737 ) ) ;
#2241 = EDGE_LOOP ( 'NONE', ( #31181, #2131, #4288, #7036 ) ) ;
#2242 = DIRECTION ( 'NONE',  ( 0.8660512985181135770, 0.4999551463232369541, 0.000000000000000000 ) ) ;
#2243 = CIRCLE ( 'NONE', #35049, 0.5756329413417604624 ) ;
#2244 = CIRCLE ( 'NONE', #10779, 0.1000000000000000194 ) ;
#2245 = CARTESIAN_POINT ( 'NONE',  ( 0.03562778247724820296, -0.5379013666131609028, 0.1838651273310172585 ) ) ;
#2247 = DIRECTION ( 'NONE',  ( -1.000000000000000000, -0.000000000000000000, -0.000000000000000000 ) ) ;
#2246 = CARTESIAN_POINT ( 'NONE',  ( 0.6651013997919192899, -1.542812421080071550, 0.4323470902494797041 ) ) ;
#2248 = DIRECTION ( 'NONE',  ( -0.8660512985181132439, -0.4999551463232375093, 0.000000000000000000 ) ) ;
#2249 = EDGE_LOOP ( 'NONE', ( #29412, #7120, #1767, #19083 ) ) ;
#2250 = CARTESIAN_POINT ( 'NONE',  ( 0.4893086098151709362, -1.099159724303276020, 0.7026458958596925042 ) ) ;
#2251 = VERTEX_POINT ( 'NONE', #27589 ) ;
#2252 = CIRCLE ( 'NONE', #34417, 0.01500000000000006016 ) ;
#2253 = DIRECTION ( 'NONE',  ( 1.000000000000000000, 0.000000000000000000, 0.000000000000000000 ) ) ;
#2254 = AXIS2_PLACEMENT_3D ( 'NONE', #1860, #39471, #7601 ) ;
#2255 = CARTESIAN_POINT ( 'NONE',  ( 0.1107380495411959126, -0.8768048433569302080, 0.5086585179081277719 ) ) ;
#2256 = DIRECTION ( 'NONE',  ( 1.387778780781449620E-15, 0.000000000000000000, 1.000000000000000000 ) ) ;
#2257 = EDGE_CURVE ( 'NONE', #10465, #22886, #12955, .T. ) ;
#2258 = CARTESIAN_POINT ( 'NONE',  ( 0.03654368633476911404, 0.08356155710620580268, -0.5047517311408941110 ) ) ;
#2259 = EDGE_CURVE ( 'NONE', #29592, #5283, #14910, .T. ) ;
#2260 = CARTESIAN_POINT ( 'NONE',  ( 0.2467884284475332646, -1.005975727473770398, 0.5856700373633461076 ) ) ;
#2261 = CARTESIAN_POINT ( 'NONE',  ( 0.3077938761450154104, -1.772073966255670596, 0.3667417262808779777 ) ) ;
#2262 = CARTESIAN_POINT ( 'NONE',  ( 0.05634301242525762560, 0.2780425975185383813, -0.3652000572937701972 ) ) ;
#2263 = CARTESIAN_POINT ( 'NONE',  ( 0.1852697686925744991, -0.8388888312570772499, 0.1465813977937011903 ) ) ;
#2264 = CARTESIAN_POINT ( 'NONE',  ( 0.03259135683726806926, -1.157323147438684030, 0.6652026314908382476 ) ) ;
#2265 = PERSON_AND_ORGANIZATION ( #28500, #32463 ) ;
#2266 = VECTOR ( 'NONE', #8685, 39.37007874015748143 ) ;
#2267 = CARTESIAN_POINT ( 'NONE',  ( 0.4403554762574504733, -1.137327559350066242, 0.4417353236092321778 ) ) ;
#2268 = CARTESIAN_POINT ( 'NONE',  ( 0.5535797480692251638, -1.186549887580578444, 0.6057417262809811076 ) ) ;
#2269 = DIRECTION ( 'NONE',  ( -1.000000000000000000, 0.000000000000000000, 0.000000000000000000 ) ) ;
#2270 = AXIS2_PLACEMENT_3D ( 'NONE', #4986, #30096, #17553 ) ;
#2271 = AXIS2_PLACEMENT_3D ( 'NONE', #17921, #5580, #36454 ) ;
#2272 = CARTESIAN_POINT ( 'NONE',  ( 2.161549057781019548E-05, -0.4383321693235875394, 0.06536088093990558012 ) ) ;
#2273 = DIRECTION ( 'NONE',  ( 0.000000000000000000, 0.000000000000000000, 1.000000000000000000 ) ) ;
#2274 = LINE ( 'NONE', #33946, #25825 ) ;
#2275 = CARTESIAN_POINT ( 'NONE',  ( 0.3587298685345038929, -1.621939747702046297, 0.4817067625245350371 ) ) ;
#2276 = AXIS2_PLACEMENT_3D ( 'NONE', #17712, #30687, #30076 ) ;
#2277 = ORIENTED_EDGE ( 'NONE', *, *, #28847, .T. ) ;
#2278 = ORIENTED_EDGE ( 'NONE', *, *, #20859, .T. ) ;
#2279 = AXIS2_PLACEMENT_3D ( 'NONE', #37055, #15466, #2914 ) ;
#2280 = CARTESIAN_POINT ( 'NONE',  ( -0.1068489084554249124, -0.4866459697499495585, 0.09652185631082288442 ) ) ;
#2281 = VERTEX_POINT ( 'NONE', #37252 ) ;
#2282 = FACE_OUTER_BOUND ( 'NONE', #31562, .T. ) ;
#2284 = ORIENTED_EDGE ( 'NONE', *, *, #12181, .F. ) ;
#2283 = CARTESIAN_POINT ( 'NONE',  ( -0.1157351208611889781, -0.4799584063719138927, 0.1184929141221633259 ) ) ;
#2286 = ORIENTED_EDGE ( 'NONE', *, *, #37409, .T. ) ;
#2285 = CARTESIAN_POINT ( 'NONE',  ( 0.007248405253956994622, -0.7849820093401896903, 0.02096406129000137619 ) ) ;
#2287 = VERTEX_POINT ( 'NONE', #21215 ) ;
#2288 = CARTESIAN_POINT ( 'NONE',  ( 0.03664605387828134830, 0.4684681574363447343, -0.1090337349854987731 ) ) ;
#2289 = ORIENTED_EDGE ( 'NONE', *, *, #18541, .F. ) ;
#2290 = CARTESIAN_POINT ( 'NONE',  ( -0.001589221141236483482, -0.5299580663956803273, 0.1754197759787374244 ) ) ;
#2291 = DIRECTION ( 'NONE',  ( 1.000000000000000000, -0.000000000000000000, -0.000000000000000000 ) ) ;
#2292 = CARTESIAN_POINT ( 'NONE',  ( 0.1734973056165642902, -1.209394307038482497, -0.5155029497116575543 ) ) ;
#2293 = PERSON_AND_ORGANIZATION ( #12257, #5033 ) ;
#2294 = AXIS2_PLACEMENT_3D ( 'NONE', #4735, #23299, #32728 ) ;
#2295 = CARTESIAN_POINT ( 'NONE',  ( -0.1710642718812830643, 0.4986889572247755198, 0.3032895567580806695 ) ) ;
#2297 = EDGE_LOOP ( 'NONE', ( #19537, #21661, #39362, #36100 ) ) ;
#2296 = EDGE_LOOP ( 'NONE', ( #9337, #21762, #2564, #18314, #37181 ) ) ;
#2298 = AXIS2_PLACEMENT_3D ( 'NONE', #13113, #25674, #38209 ) ;
#2299 = CARTESIAN_POINT ( 'NONE',  ( 0.2469141422421070875, -1.581573626495411444, -0.3511777555542848206 ) ) ;
#2300 = CARTESIAN_POINT ( 'NONE',  ( 0.2209893336501091432, -1.227886349168061386, 0.5261107291778043260 ) ) ;
#2301 = AXIS2_PLACEMENT_3D ( 'NONE', #35795, #26548, #32703 ) ;
#2302 = CARTESIAN_POINT ( 'NONE',  ( 0.2002263348979474444, -0.8551021424006158833, 0.6387041187184567814 ) ) ;
#2303 = CARTESIAN_POINT ( 'NONE',  ( 0.1856764667174918837, -0.8115940886088498507, 0.08463465656060843723 ) ) ;
#2304 = FACE_OUTER_BOUND ( 'NONE', #14277, .T. ) ;
#2305 = APPLIED_APPROVAL_ASSIGNMENT ( #32073, ( #22018 ) ) ;
#2306 = CARTESIAN_POINT ( 'NONE',  ( 0.4002255668615350426, -1.695126185520418938, -0.4229178359567086765 ) ) ;
#2307 = CARTESIAN_POINT ( 'NONE',  ( -0.2399999999999999079, -3.941790907013290823, 0.08058400322088303536 ) ) ;
#2308 = AXIS2_PLACEMENT_3D ( 'NONE', #39626, #17628, #1405 ) ;
#2309 = CARTESIAN_POINT ( 'NONE',  ( 0.3544525855955990568, -1.628498139902175401, -0.6593841416021928303 ) ) ;
#2310 = CARTESIAN_POINT ( 'NONE',  ( 0.3699999999999788458, -2.120743408781763595, -0.4622665795123166999 ) ) ;
#2311 = CARTESIAN_POINT ( 'NONE',  ( 0.3077938761450154104, -1.772073966255670596, 0.3667417262808779777 ) ) ;
#2312 = CARTESIAN_POINT ( 'NONE',  ( -1.316612518408581027E-05, -0.9424504616873518037, 0.09060630441213164687 ) ) ;
#2313 = CARTESIAN_POINT ( 'NONE',  ( 0.4634712904840416203, -1.711704060178988129, -0.5155029497116575543 ) ) ;
#2314 = DIRECTION ( 'NONE',  ( 0.000000000000000000, 0.000000000000000000, 1.000000000000000000 ) ) ;
#2315 = CARTESIAN_POINT ( 'NONE',  ( 0.1999999999999789724, -2.166079853131637645, -0.5407606602423824516 ) ) ;
#2316 = CARTESIAN_POINT ( 'NONE',  ( 0.07933644511000853550, -0.9611106349790075054, 0.8249633512138372371 ) ) ;
#2317 = CARTESIAN_POINT ( 'NONE',  ( 0.03393842632515668700, -0.9998690014380283708, 0.6797094769501190736 ) ) ;
#2318 = APPROVAL_STATUS ( 'not_yet_approved' ) ;
#2319 = CARTESIAN_POINT ( 'NONE',  ( 0.5091714098097919194, -1.126742604313814677, 0.8493738626068785269 ) ) ;
#2320 = CONICAL_SURFACE ( 'NONE', #23332, 0.1400000000000013178, 1.047197551196602072 ) ;
#2321 = AXIS2_PLACEMENT_3D ( 'NONE', #22952, #17161, #29105 ) ;
#2322 = CARTESIAN_POINT ( 'NONE',  ( 0.4115766028365042128, -1.733048369835246794, 0.5182417262812423209 ) ) ;
#2323 = CARTESIAN_POINT ( 'NONE',  ( 0.02881408050861685236, -0.06014027758171745092, -0.4945500181289065322 ) ) ;
#2324 = AXIS2_PLACEMENT_3D ( 'NONE', #39345, #1325, #32964 ) ;
#2325 = CARTESIAN_POINT ( 'NONE',  ( 0.5264113014007820723, -1.640729993778254014, 0.5682417262808777680 ) ) ;
#2326 = ORIENTED_EDGE ( 'NONE', *, *, #26541, .T. ) ;
#2327 = PLANE ( 'NONE',  #19127 ) ;
#2328 = APPLIED_APPROVAL_ASSIGNMENT ( #39090, ( #25768 ) ) ;
#2329 = CARTESIAN_POINT ( 'NONE',  ( 0.07864456654739519770, -0.9658104792752110201, 0.8218898466748431053 ) ) ;
#2330 = CARTESIAN_POINT ( 'NONE',  ( 0.5385340078061969793, -1.420402263057676695, 0.7715738128166309551 ) ) ;
#2331 = CARTESIAN_POINT ( 'NONE',  ( -0.2399999999999999079, -2.375187403135927688, -0.6336237179921873075 ) ) ;
#2333 = ORIENTED_EDGE ( 'NONE', *, *, #3960, .F. ) ;
#2332 = DIRECTION ( 'NONE',  ( 1.000000000000000000, 3.624433060062967676E-13, -2.563064096159672774E-12 ) ) ;
#2334 = CONICAL_SURFACE ( 'NONE', #5598, 0.1600000000000000588, 1.047197551196602516 ) ;
#2335 = CARTESIAN_POINT ( 'NONE',  ( 0.2889710164712426255, -0.7847915145120791802, 0.6224945701162477585 ) ) ;
#2337 = EDGE_LOOP ( 'NONE', ( #29855, #26571 ) ) ;
#2336 = ORIENTED_EDGE ( 'NONE', *, *, #28866, .F. ) ;
#2338 = CARTESIAN_POINT ( 'NONE',  ( 0.6738503551975361106, -1.390429358051159081, 0.7373033579730302600 ) ) ;
#2339 = CARTESIAN_POINT ( 'NONE',  ( 0.4941573835580928553, -1.197472013777949540, -0.4122610257295771796 ) ) ;
#2340 = CARTESIAN_POINT ( 'NONE',  ( 0.1499999999999994671, 0.5230810839623357689, -0.1699593469062178064 ) ) ;
#2341 = DATE_TIME_ROLE ( 'classification_date' ) ;
#2342 = FACE_OUTER_BOUND ( 'NONE', #37522, .T. ) ;
#2343 = ORIENTED_EDGE ( 'NONE', *, *, #10360, .T. ) ;
#2344 = CARTESIAN_POINT ( 'NONE',  ( 0.2214974906291148626, -0.9030582019982653641, 0.6599196580771191645 ) ) ;
#2345 = CARTESIAN_POINT ( 'NONE',  ( 0.2211959769661343000, -1.309495541150525799, -0.5931747813493346566 ) ) ;
#2346 = CARTESIAN_POINT ( 'NONE',  ( 0.4988733860125649788, -1.542123411666028732, 0.6032420550392955105 ) ) ;
#2347 = CARTESIAN_POINT ( 'NONE',  ( -0.001106909109950914580, -0.7985540816996060665, 0.01933639101178150771 ) ) ;
#2348 = CARTESIAN_POINT ( 'NONE',  ( 0.0007702871825654963910, -0.9531316724789442585, 0.2767708779485607562 ) ) ;
#2349 = VERTEX_POINT ( 'NONE', #9469 ) ;
#2350 = ORIENTED_EDGE ( 'NONE', *, *, #29609, .T. ) ;
#2351 = DIRECTION ( 'NONE',  ( 1.000000000000000000, -0.000000000000000000, -0.000000000000000000 ) ) ;
#2352 = CARTESIAN_POINT ( 'NONE',  ( 0.3612790108085988106, -0.8653713489192644825, 0.7675946798073856048 ) ) ;
#2353 = CIRCLE ( 'NONE', #25350, 0.01500000000000005496 ) ;
#2354 = DIRECTION ( 'NONE',  ( 0.000000000000000000, 0.000000000000000000, 1.000000000000000000 ) ) ;
#2355 = EDGE_CURVE ( 'NONE', #31920, #15882, #33751, .T. ) ;
#2356 = LINE ( 'NONE', #17972, #33054 ) ;
#2357 = SECURITY_CLASSIFICATION ( '', '', #11765 ) ;
#2358 = APPROVAL ( #306, 'UNKNOWN' ) ;
#2359 = CARTESIAN_POINT ( 'NONE',  ( 0.1999999999999789724, -2.183180860297921466, -0.4937760292030871079 ) ) ;
#2360 = CARTESIAN_POINT ( 'NONE',  ( 2.696301922142129168E-33, 7.654042494670954463E-18, -0.06250000000000000000 ) ) ;
#2361 = AXIS2_PLACEMENT_3D ( 'NONE', #4215, #12883, #13077 ) ;
#2362 = CARTESIAN_POINT ( 'NONE',  ( 0.3119755472902833726, -1.175847033624922489, 0.5195546043588886720 ) ) ;
#2363 = CARTESIAN_POINT ( 'NONE',  ( 0.5544279432241370209, -1.187676084274785548, 0.5985052393047670671 ) ) ;
#2364 = PERSON_AND_ORGANIZATION_ROLE ( 'creator' ) ;
#2365 = CARTESIAN_POINT ( 'NONE',  ( 0.1889603646001475068, -0.5843802352234823694, 0.2966845687057266812 ) ) ;
#2366 = CARTESIAN_POINT ( 'NONE',  ( 0.3690696315487195789, -2.046121508319152849, -0.6829205282668205923 ) ) ;
#2367 = CARTESIAN_POINT ( 'NONE',  ( 0.6590705178848084156, -1.601721441849921268, 0.5182417262812423209 ) ) ;
#2368 = DIRECTION ( 'NONE',  ( -2.280301054154496008E-31, 1.000000000000000000, -2.106022274728121591E-16 ) ) ;
#2369 = ORIENTED_EDGE ( 'NONE', *, *, #23378, .F. ) ;
#2370 = CARTESIAN_POINT ( 'NONE',  ( 0.3759405909208060059, -1.611975652049966179, -0.3607904488862428982 ) ) ;
#2371 = DIRECTION ( 'NONE',  ( -0.4999551463232377313, 0.8660512985181132439, -0.000000000000000000 ) ) ;
#2372 = CIRCLE ( 'NONE', #15530, 0.1000000000000000194 ) ;
#2373 = CARTESIAN_POINT ( 'NONE',  ( -0.05634490452572842034, -0.005064009952712422366, -0.4588782462578062660 ) ) ;
#2374 = ADVANCED_FACE ( 'NONE', ( #31296 ), #40234, .T. ) ;
#2375 = CARTESIAN_POINT ( 'NONE',  ( 0.02141150205530418724, -0.8856259524795232485, 0.4902799836155304347 ) ) ;
#2376 = VERTEX_POINT ( 'NONE', #13582 ) ;
#2377 = EDGE_CURVE ( 'NONE', #31608, #30897, #36602, .T. ) ;
#2378 = CARTESIAN_POINT ( 'NONE',  ( -0.03868649100028188209, 0.3066017772948842479, 0.3648306000529296100 ) ) ;
#2379 = CARTESIAN_POINT ( 'NONE',  ( 0.03478489236950984415, -0.07228210831916198620, 0.5113624180529658947 ) ) ;
#2380 = LOCAL_TIME ( 0, 53, 7.000000000000000000, #9298 ) ;
#2381 = CARTESIAN_POINT ( 'NONE',  ( 0.04308611741968229603, -0.4494132222463866344, -0.2058373899768682624 ) ) ;
#2382 = CARTESIAN_POINT ( 'NONE',  ( 0.1867562162627207645, -1.721001719842840227, -0.3581518700804716127 ) ) ;
#2383 = EDGE_CURVE ( 'NONE', #12135, #36587, #7374, .T. ) ;
#2384 = CARTESIAN_POINT ( 'NONE',  ( 0.4203373861789014843, -1.172197600499562009, 0.6891193374043744768 ) ) ;
#2386 = CARTESIAN_POINT ( 'NONE',  ( 0.1909286924077255032, -1.257064795538239022, -0.4400554600884079015 ) ) ;
#2385 = CARTESIAN_POINT ( 'NONE',  ( 0.04139678531769570152, 0.4525211694413215358, 0.1291682248591994320 ) ) ;
#2387 = EDGE_CURVE ( 'NONE', #35372, #36916, #669, .T. ) ;
#2388 = FACE_BOUND ( 'NONE', #23456, .T. ) ;
#2389 = ORIENTED_EDGE ( 'NONE', *, *, #40640, .F. ) ;
#2390 = EDGE_LOOP ( 'NONE', ( #695, #2455 ) ) ;
#2391 = ADVANCED_FACE ( 'NONE', ( #38056 ), #9505, .F. ) ;
#2392 = AXIS2_PLACEMENT_3D ( 'NONE', #35692, #23383, #16975 ) ;
#2393 = CARTESIAN_POINT ( 'NONE',  ( 0.1568341744305939145, -0.7257825074155194178, 0.5774065548309712526 ) ) ;
#2394 = EDGE_LOOP ( 'NONE', ( #26405, #27725, #14929, #2495, #20764, #36435 ) ) ;
#2395 = DIRECTION ( 'NONE',  ( -1.000000000000000000, 0.000000000000000000, 0.000000000000000000 ) ) ;
#2396 = CARTESIAN_POINT ( 'NONE',  ( 0.4424104223302582906, -1.573875977550938110, 0.5848388507199695496 ) ) ;
#2398 = CARTESIAN_POINT ( 'NONE',  ( 0.6047538891612447287, -1.605163873594933843, 0.4396382108053983884 ) ) ;
#2397 = CARTESIAN_POINT ( 'NONE',  ( 0.3544525855956190963, -1.628498139902242681, -0.6593841416022943047 ) ) ;
#2399 = CARTESIAN_POINT ( 'NONE',  ( -0.1210148435730033917, -0.5061394519556894345, 0.1438724812234795092 ) ) ;
#2400 = VERTEX_POINT ( 'NONE', #32278 ) ;
#2401 = CARTESIAN_POINT ( 'NONE',  ( 0.4905912024403834559, -1.589136493782425719, -0.5753219298350721322 ) ) ;
#2402 = ORIENTED_EDGE ( 'NONE', *, *, #8817, .F. ) ;
#2403 = CARTESIAN_POINT ( 'NONE',  ( 0.3871031770338608791, -1.873715675035283024, -0.3077635280768467596 ) ) ;
#2404 = CARTESIAN_POINT ( 'NONE',  ( 0.4219977553732560116, -1.241953814191006256, 0.8304148750200471829 ) ) ;
#2405 = CARTESIAN_POINT ( 'NONE',  ( 0.4746252454845096280, -1.666917666310047119, 0.4878717617910002802 ) ) ;
#2406 = DIRECTION ( 'NONE',  ( 1.000000000000000000, 0.000000000000000000, 0.000000000000000000 ) ) ;
#2407 = EDGE_CURVE ( 'NONE', #22774, #2376, #19949, .T. ) ;
#2408 = CARTESIAN_POINT ( 'NONE',  ( 0.8248651029816849167, 0.000000000000000000, 0.000000000000000000 ) ) ;
#2409 = FACE_BOUND ( 'NONE', #23150, .T. ) ;
#2410 = CYLINDRICAL_SURFACE ( 'NONE', #29228, 0.5400000000000017009 ) ;
#2411 = DIRECTION ( 'NONE',  ( -1.000000000000000000, 0.000000000000000000, 0.000000000000000000 ) ) ;
#2412 = AXIS2_PLACEMENT_3D ( 'NONE', #17855, #33693, #24453 ) ;
#2413 = CARTESIAN_POINT ( 'NONE',  ( 0.3805742881279173817, -0.9147748976205605231, 0.7744170315737640697 ) ) ;
#2414 = CARTESIAN_POINT ( 'NONE',  ( -0.05281452789367933193, 0.3064952470002013651, 0.3541670097232195169 ) ) ;
#2415 = CARTESIAN_POINT ( 'NONE',  ( 0.006178162761485163183, -0.9774033419544895240, 0.4753174591059177168 ) ) ;
#2416 = ORGANIZATION ( 'NAUO-ORG12', 'UNSPECIFIED', 'UNSPECIFIED' ) ;
#2417 = CARTESIAN_POINT ( 'NONE',  ( 0.6202635901223110260, -1.561719534786903729, -0.5933892023552781447 ) ) ;
#2418 = CARTESIAN_POINT ( 'NONE',  ( 0.05257579864948812298, -1.595298430439333393, -0.6695260341086051170 ) ) ;
#2419 = CARTESIAN_POINT ( 'NONE',  ( 0.02999999999997891853, -2.097675824466501915, -0.2588528740066096678 ) ) ;
#2420 = CARTESIAN_POINT ( 'NONE',  ( 0.6011193747858227798, -1.595581932925101976, 0.4276689662439276396 ) ) ;
#2421 = TOROIDAL_SURFACE ( 'NONE', #38555, 0.04249999999999999611, 0.02499999999999995628 ) ;
#2422 = DIRECTION ( 'NONE',  ( 0.000000000000000000, 0.000000000000000000, -1.000000000000000000 ) ) ;
#2423 = B_SPLINE_CURVE_WITH_KNOTS ( 'NONE', 3,
 ( #12434, #24601, #6816, #34450, #38507, #905 ),
 .UNSPECIFIED., .F., .F.,
 ( 4, 2, 4 ),
 ( -4.995199405858393678E-06, 0.0003667636180932637305, 0.0007385224355923858657 ),
 .UNSPECIFIED. ) ;
#2424 = VERTEX_POINT ( 'NONE', #4093 ) ;
#2425 = DIRECTION ( 'NONE',  ( -0.3468893892380657262, 0.7396492646828742856, 0.5767033179097595941 ) ) ;
#2426 = DIRECTION ( 'NONE',  ( 0.000000000000000000, 0.000000000000000000, -1.000000000000000000 ) ) ;
#2427 = LINE ( 'NONE', #33670, #35050 ) ;
#2428 = CARTESIAN_POINT ( 'NONE',  ( 0.4751758298663431024, -1.652426242819088342, -0.6334442537810195395 ) ) ;
#2429 = ORIENTED_EDGE ( 'NONE', *, *, #25857, .T. ) ;
#2430 = EDGE_CURVE ( 'NONE', #35420, #12540, #11621, .T. ) ;
#2431 = FACE_OUTER_BOUND ( 'NONE', #12347, .T. ) ;
#2432 = FACE_OUTER_BOUND ( 'NONE', #29977, .T. ) ;
#2433 = DIRECTION ( 'NONE',  ( -1.000000000000000000, -7.857794173099924470E-32, -8.628166150854818811E-32 ) ) ;
#2434 = CARTESIAN_POINT ( 'NONE',  ( 0.05999999999999990757, 0.000000000000000000, 0.5614999999999926716 ) ) ;
#2435 = EDGE_CURVE ( 'NONE', #37335, #8583, #13370, .T. ) ;
#2436 = CARTESIAN_POINT ( 'NONE',  ( 0.4037390063638767734, -1.153315448710456881, 0.7518491778188490793 ) ) ;
#2438 = ORIENTED_EDGE ( 'NONE', *, *, #25908, .F. ) ;
#2437 = DIRECTION ( 'NONE',  ( -0.5000000000000002220, 0.000000000000000000, 0.8660254037844384856 ) ) ;
#2439 = CARTESIAN_POINT ( 'NONE',  ( 0.4975638555224211612, -1.097967759515461550, 0.6244301767862630026 ) ) ;
#2440 = CIRCLE ( 'NONE', #14904, 0.03000000000000000930 ) ;
#2441 = ORIENTED_EDGE ( 'NONE', *, *, #16789, .F. ) ;
#2442 = EDGE_CURVE ( 'NONE', #19638, #14679, #40364, .T. ) ;
#2443 = DIRECTION ( 'NONE',  ( 1.000000000000000000, 0.000000000000000000, 0.000000000000000000 ) ) ;
#2444 = ORIENTED_EDGE ( 'NONE', *, *, #15258, .T. ) ;
#2445 = CARTESIAN_POINT ( 'NONE',  ( -0.04155248107635957366, 0.2623121065566128007, -0.3903559784317159886 ) ) ;
#2446 = CARTESIAN_POINT ( 'NONE',  ( 0.2700198664771301660, -1.375350736655498229, 0.9052646506941134374 ) ) ;
#2448 = CARTESIAN_POINT ( 'NONE',  ( 0.1766268836841131673, -0.5128407814923380270, -0.004769247607836917847 ) ) ;
#2447 = CARTESIAN_POINT ( 'NONE',  ( -0.2399999999999999079, -4.098813193844367042, -0.6491724279539748954 ) ) ;
#2449 = FACE_OUTER_BOUND ( 'NONE', #32911, .T. ) ;
#2450 = ORIENTED_EDGE ( 'NONE', *, *, #39553, .F. ) ;
#2451 = EDGE_LOOP ( 'NONE', ( #36493, #3544, #24242, #1374 ) ) ;
#2452 = ADVANCED_FACE ( 'NONE', ( #23047 ), #7174, .T. ) ;
#2453 = CARTESIAN_POINT ( 'NONE',  ( 0.4110504371346864194, -1.121748555647557266, 0.6019148399695160023 ) ) ;
#2454 = CARTESIAN_POINT ( 'NONE',  ( 0.5526746308725590806, -1.505849688569114608, 0.6462697217425257268 ) ) ;
#2455 = ORIENTED_EDGE ( 'NONE', *, *, #995, .F. ) ;
#2456 = FACE_OUTER_BOUND ( 'NONE', #19343, .T. ) ;
#2457 = CARTESIAN_POINT ( 'NONE',  ( 0.3622253751127874066, -1.756884464425453984, -0.4902987826081479650 ) ) ;
#2458 = ADVANCED_FACE ( 'NONE', ( #17471 ), #3732, .T. ) ;
#2459 = CARTESIAN_POINT ( 'NONE',  ( 0.09153058604599668968, -0.8486693615597448170, 0.3862177764867652519 ) ) ;
#2460 = CARTESIAN_POINT ( 'NONE',  ( 0.5860390410503526493, -1.538367470261696957, -0.4143366047946381858 ) ) ;
#2461 = CARTESIAN_POINT ( 'NONE',  ( -0.1157351144566549916, -0.4800210170678197441, 0.3382895569178748785 ) ) ;
#2462 = EDGE_CURVE ( 'NONE', #1752, #51, #373, .T. ) ;
#2463 = CARTESIAN_POINT ( 'NONE',  ( 0.5053588047760252389, -1.583603243833816565, -0.5401600205605632254 ) ) ;
#2464 = CARTESIAN_POINT ( 'NONE',  ( 0.7472913949145145729, -1.513305546476923613, 0.4177417262808786336 ) ) ;
#2465 = EDGE_CURVE ( 'NONE', #21660, #30753, #22663, .T. ) ;
#2466 = DIRECTION ( 'NONE',  ( 1.000000000000000000, 6.779273404243070203E-32, 4.314083075427408311E-32 ) ) ;
#2467 = CARTESIAN_POINT ( 'NONE',  ( -0.2399999999999999079, -3.985676108854518507, -0.7623095129438225426 ) ) ;
#2468 = CARTESIAN_POINT ( 'NONE',  ( 0.01226155556033644428, -1.026869578359442370, 0.5617476425356938696 ) ) ;
#2469 = PERSON_AND_ORGANIZATION_ROLE ( 'creator' ) ;
#2470 = CARTESIAN_POINT ( 'NONE',  ( 0.4302259848396451369, -1.133463226324729733, 0.4383158576218293967 ) ) ;
#2471 = CARTESIAN_POINT ( 'NONE',  ( 0.01895494625228151542, -0.5124113341948460798, 0.08888305413160187129 ) ) ;
#2472 = CARTESIAN_POINT ( 'NONE',  ( 0.5943483229377598542, -1.499644859401920938, -0.6402273302934655685 ) ) ;
#2473 = CARTESIAN_POINT ( 'NONE',  ( 0.01186068252828692722, -0.5714573607336731476, -0.08599319573038584352 ) ) ;
#2474 = CARTESIAN_POINT ( 'NONE',  ( -0.01548846960707531660, -0.4638115001431011297, -0.2459753896937847684 ) ) ;
#2475 = DIRECTION ( 'NONE',  ( 1.000000000000000000, -0.000000000000000000, -0.000000000000000000 ) ) ;
#2476 = CARTESIAN_POINT ( 'NONE',  ( 0.3918164284306930312, -1.740509091685305876, -0.5895034584783541698 ) ) ;
#2477 = ORIENTED_EDGE ( 'NONE', *, *, #28253, .T. ) ;
#2478 = ORIENTED_EDGE ( 'NONE', *, *, #19314, .T. ) ;
#2479 = CARTESIAN_POINT ( 'NONE',  ( -0.1157923916714846541, -0.5295015842442638565, 0.1380392329925947958 ) ) ;
#2480 = ORIENTED_EDGE ( 'NONE', *, *, #2387, .T. ) ;
#2481 = CARTESIAN_POINT ( 'NONE',  ( -0.2399999999999999079, -3.156018320128275878, -0.4841849112664152743 ) ) ;
#2482 = EDGE_CURVE ( 'NONE', #23421, #22699, #33673, .T. ) ;
#2483 = CARTESIAN_POINT ( 'NONE',  ( -0.1062912471183645874, -0.4837944836747484212, 0.1097058945452955153 ) ) ;
#2485 = VERTEX_POINT ( 'NONE', #20775 ) ;
#2484 = CARTESIAN_POINT ( 'NONE',  ( 0.05999999999999990757, 0.5878163732725504298, -0.2704268771689488093 ) ) ;
#2486 = VERTEX_POINT ( 'NONE', #8399 ) ;
#2487 = CARTESIAN_POINT ( 'NONE',  ( 0.02235124290213165790, 0.5044963136723996655, -0.09030809412322095275 ) ) ;
#2488 = ORIENTED_EDGE ( 'NONE', *, *, #35188, .T. ) ;
#2489 = CARTESIAN_POINT ( 'NONE',  ( -0.0002190029760103817690, -0.5598929387007183234, 0.2782029251743489140 ) ) ;
#2491 = CARTESIAN_POINT ( 'NONE',  ( 0.2055039781776641650, -1.247779362046685714, 0.5783501873904609569 ) ) ;
#2490 = CARTESIAN_POINT ( 'NONE',  ( 0.1465179088820477704, -0.8893166351135021186, 0.5570520123011054592 ) ) ;
#2492 = CARTESIAN_POINT ( 'NONE',  ( 0.3605386037194296400, -1.159593875931560714, 0.5133706147585744839 ) ) ;
#2493 = CARTESIAN_POINT ( 'NONE',  ( 0.1984286359563034452, -1.270056632699685162, -0.7137153576319578141 ) ) ;
#2495 = ORIENTED_EDGE ( 'NONE', *, *, #4868, .T. ) ;
#2494 = ORIENTED_EDGE ( 'NONE', *, *, #9500, .F. ) ;
#2496 = CARTESIAN_POINT ( 'NONE',  ( -0.01548846960707517956, -0.09319974324249266640, -0.5318964258758781538 ) ) ;
#2497 = CARTESIAN_POINT ( 'NONE',  ( 0.3853411735687863326, -1.756807109041631509, -0.4499573014711771846 ) ) ;
#2498 = CARTESIAN_POINT ( 'NONE',  ( -0.05252049209742432057, -0.4488546425834899489, 0.1362647994370363713 ) ) ;
#2499 = B_SPLINE_SURFACE_WITH_KNOTS ( 'NONE', 3, 3, ( 
 ( #22822, #19517, #38213, #4051, #7132, #7327, #13721, #32232, #1218, #22401, #38020, #35739, #29377, #10038, #34930, #19904, #29165, #32442, #12937, #1027, #3671, #13538, #6736, #38620, #3460, #25484, #16833, #10440, #23001, #26287, #38810, #10640, #7549, #19312, #16229, #28768, #626, #7945, #5069, #27313, #8555, #10858, #20519, #11663, #32654, #8159, #5261, #39842, #17630, #1408, #13916, #30177, #2209, #20321, #26488, #33052, #29985, #27095, #4858, #24222, #35949, #33455, #1819, #8364, #39025, #14136, #23432, #2006, #29768, #17024, #30379, #20933, #36556, #32842, #17431, #7755, #14532, #4460 ),
 ( #24029, #26898, #14335, #17820, #20733, #4649, #33260, #14749, #36745, #29565, #26707, #39628, #39427, #36135, #39238, #11465, #11250, #17221, #1613, #11060, #23619, #23819, #36341, #3204, #21729, #8767, #2806, #34068, #37355, #15353, #21344, #33655, #12460, #21949, #167, #37547, #33882, #8978, #9168, #34478, #30589, #28297, #25220, #24834, #12657, #37766, #2413, #5684, #40451, #21548, #5466, #15749, #5868, #37164, #34265, #30983, #25014, #18427, #27913, #14951, #12276, #6074, #6289, #21128, #18643, #18240, #27503, #40029, #24419, #11852, #18033, #36950, #30784, #31204, #28113, #3021, #15566, #2603 ),
 ( #15140, #40644, #27702, #9369, #18861, #31402, #40233, #12069, #24634, #22352, #38361, #970, #4212, #26051, #31800, #32189, #31998, #13076, #3616, #10200, #35084, #4001, #13488, #25841, #38571, #9782, #35290, #32390, #22768, #37972, #3810, #22556, #7084, #16365, #34871, #22164, #10392, #22954, #29328, #35473, #6684, #38161, #19654, #7277, #19051, #16778, #13674, #13275, #1172, #26236, #31587, #19258, #28903, #9985, #34678, #9585, #19856, #6483, #767, #3405, #15961, #28506, #384, #12882, #16180, #25441, #28720, #16566, #583, #25630, #29110, #6891, #19464, #4416, #11016, #14693, #23162, #39574 ),
 ( #7705, #23572, #5023, #35898, #36092, #17380, #20274, #13863, #7892, #8319, #32794, #29717, #1354, #14475, #20465, #32998, #20073, #11407, #7492, #39192, #29939, #17770, #26440, #4804, #1778, #14290, #23382, #38975, #17168, #29517, #2157, #27046, #17588, #10805, #38757, #10587, #23975, #20889, #4595, #32601, #26852, #1561, #16974, #35691, #36508, #14083, #30323, #26660, #39379, #11202, #33217, #23766, #36286, #8104, #20682, #30133, #1961, #33411, #5220, #5631, #8512, #18381, #5821, #12017, #34426, #30929, #21077, #18595, #27460, #2755, #17979, #36704, #3160, #24576, #24179, #6241, #30538, #21286 ),
 ( #39790, #15093, #18814, #31357, #27261, #5413, #11622, #33602, #15304, #2363, #14901, #27651, #31150, #39984, #12415, #24965, #21899, #11805, #24363, #40180, #6025, #18186, #2558, #37496, #36900, #37110, #34213, #8710, #8927, #27860, #33828, #30736, #21501, #9318, #34019, #40398, #12224, #2968, #24787, #37305, #9118, #28068, #21683, #15517, #40597, #16328, #25587, #7049, #28671, #13035, #25175, #6839, #35030, #929, #10358, #19422, #12833, #9538, #22115, #19005, #34636, #12611, #7236, #6433, #22505, #22718, #22921, #31537, #9738, #31956, #329, #10145, #28250, #3565, #35436, #19805, #32343, #3349 ),
 ( #15908, #19617, #724, #32152, #114, #3773, #28454, #34820, #25396, #540, #15704, #37712, #16520, #6630, #38114, #3958, #35250, #38318, #26006, #37925, #22305, #19205, #31748, #16134, #28864, #9933, #13223, #25792, #29060, #13437, #38528, #20420, #17540, #39525, #17331, #13633, #26199, #1729, #14429, #32556, #38723, #20232, #1517, #39335, #32752, #11357, #7449, #4974, #14036, #20634, #10544, #26395, #23119, #14245, #1318, #29282, #1915, #33169, #8055, #4375, #29675, #35642, #26808, #4165, #39146, #16931, #32954, #36241, #10973, #4556, #30087, #4758, #29474, #29889, #26997, #23927, #36457, #38926 ),
 ( #20022, #8269, #20842, #17125, #16731, #1131, #7848, #26610, #11157, #10757, #23530, #13825, #36049, #23329, #23714, #35852, #7665, #12330, #14637, #25075, #12520, #18701, #448, #37609, #27208, #25288, #34123, #9432, #24137, #2100, #9836, #31261, #30270, #33362, #11575, #9221, #12943, #5170, #22010, #6537, #28571, #6345, #39741, #36659, #31453, #3471, #21029, #8465, #21793, #3076, #28362, #34326, #25492, #5925, #34732, #15619, #9646, #18489, #15410, #31044, #3261, #2863, #17722, #31651, #22214, #37830, #27968, #28167, #40507, #15811, #24887, #31, #37410, #34536, #19112, #18917, #6137, #16027 ) ),
 .UNSPECIFIED., .F., .F., .F.,
 ( 4, 1, 1, 1, 4 ),
 ( 4, 3, 1, 1, 1, 1, 1, 1, 1, 1, 1, 1, 1, 1, 1, 1, 1, 1, 1, 1, 1, 1, 1, 1, 1, 1, 1, 1, 1, 1, 1, 1, 1, 1, 1, 1, 1, 1, 1, 1, 1, 1, 1, 1, 1, 1, 1, 1, 1, 1, 1, 1, 1, 1, 1, 1, 1, 1, 1, 1, 1, 1, 1, 1, 1, 1, 1, 1, 1, 1, 1, 1, 1, 4 ),
 ( 0.000000000000000000, 0.2500000000000000000, 0.5000000000000000000, 0.7500000000000000000, 1.000000000000000000 ),
 ( -0.01000000000000000021, 0.000000000000000000, 0.002255859375000000052, 0.004511718750000000104, 0.006767578124999999722, 0.009023437500000000208, 0.01127929687499999896, 0.01353515624999999944, 0.01579101562499999820, 0.01804687500000000042, 0.02255859374999999792, 0.02707031249999999889, 0.03158203124999999639, 0.03609375000000000083, 0.04060546874999999833, 0.04511718749999999584, 0.04962890625000000028, 0.05414062499999999778, 0.05865234375000000222, 0.06316406249999999278, 0.06767578124999999722, 0.07218750000000000167, 0.07669921874999999223, 0.08121093749999999667, 0.09023437499999999167, 0.09925781250000000056, 0.1082812499999999956, 0.1173046875000000044, 0.1263281249999999856, 0.1353515624999999944, 0.1443750000000000033, 0.1533984374999999845, 0.1624218749999999933, 0.1714453125000000022, 0.1804687499999999833, 0.1894921874999999922, 0.1985156250000000011, 0.2075390624999999822, 0.2165624999999999911, 0.2346093750000000089, 0.2526562499999999711, 0.2707031249999999889, 0.2887500000000000067, 0.3067968749999999689, 0.3248437499999999867, 0.3428906250000000044, 0.3609374999999999667, 0.3789843749999999845, 0.3970312500000000022, 0.4150781249999999645, 0.4331249999999999822, 0.4511718750000000000, 0.4692187500000000178, 0.4872656250000000355, 0.5053124999999999423, 0.5414062499999999778, 0.5775000000000000133, 0.6303124999999999423, 0.6567187500000000178, 0.6831249999999999822, 0.7095312499999999467, 0.7359375000000000222, 0.7623437499999999867, 0.7887500000000000622, 0.8151562500000000266, 0.8415624999999999911, 0.8679687499999999556, 0.8943750000000001421, 0.9207812499999998845, 0.9471875000000000711, 0.9603906250000000533, 0.9735937500000000355, 0.9867968750000000178, 1.000000000000000000 ),
 .UNSPECIFIED. ) ;
#2500 = CARTESIAN_POINT ( 'NONE',  ( 0.2625882174288838855, -0.9523961353426481091, 0.7085637651928656799 ) ) ;
#2501 = CARTESIAN_POINT ( 'NONE',  ( 0.1871311130424547498, -0.7120295780690556464, 0.03084641936662753381 ) ) ;
#2502 = CARTESIAN_POINT ( 'NONE',  ( -0.1743922129835729085, -0.5166151207188712791, 0.3750000000000001110 ) ) ;
#2503 = CARTESIAN_POINT ( 'NONE',  ( 0.2711450911080737769, -1.632422954829337636, 0.7869752074672371478 ) ) ;
#2504 = EDGE_CURVE ( 'NONE', #29444, #27585, #33298, .T. ) ;
#2505 = APPLIED_DATE_AND_TIME_ASSIGNMENT ( #9063, #18732, ( #12929 ) ) ;
#2506 = CARTESIAN_POINT ( 'NONE',  ( 0.3761284049005145236, -1.714742088754553029, -0.4155147620960898958 ) ) ;
#2507 = CARTESIAN_POINT ( 'NONE',  ( 0.4130427319115463902, -1.705619880099039198, 0.4224177903210530882 ) ) ;
#2508 = ADVANCED_FACE ( 'NONE', ( #11703 ), #14765, .T. ) ;
#2509 = AXIS2_PLACEMENT_3D ( 'NONE', #16655, #20161, #26527 ) ;
#2510 = CARTESIAN_POINT ( 'NONE',  ( 0.4915260346479126685, -1.695508583366576616, -0.4333519947141560857 ) ) ;
#2511 = CARTESIAN_POINT ( 'NONE',  ( 0.3699999999999797895, -2.166079853131637645, -0.4467913981637911536 ) ) ;
#2512 = CARTESIAN_POINT ( 'NONE',  ( 0.4815360835401190087, -1.665003689908300277, 0.5707417262808793801 ) ) ;
#2513 = CARTESIAN_POINT ( 'NONE',  ( 5.687846274369038479E-16, -0.3059742766594579222, -0.06173076923076999123 ) ) ;
#2514 = CARTESIAN_POINT ( 'NONE',  ( 0.3706793757908091735, -1.615012852715395741, -0.4172838525897034079 ) ) ;
#2515 = DIRECTION ( 'NONE',  ( 0.9999999999999997780, -6.162975822039154730E-33, -1.232595164407830946E-32 ) ) ;
#2516 = CARTESIAN_POINT ( 'NONE',  ( 0.7022701326239239039, -1.539209993927390219, 0.4224083929475443977 ) ) ;
#2517 = CARTESIAN_POINT ( 'NONE',  ( 0.01618294926847982027, -0.6819691077562005654, 0.5071040197741758515 ) ) ;
#2518 = CARTESIAN_POINT ( 'NONE',  ( 0.08705077985668224771, -1.275137320191813917, 0.7451449987256821839 ) ) ;
#2519 = SHAPE_DEFINITION_REPRESENTATION ( #7127, #9349 ) ;
#2520 = CARTESIAN_POINT ( 'NONE',  ( 0.5297859054048726923, -1.159963375372088823, 0.8529160106009885389 ) ) ;
#2521 = CARTESIAN_POINT ( 'NONE',  ( 0.6988007311651551756, -1.542424956370897160, 0.5852637934084858884 ) ) ;
#2522 = CARTESIAN_POINT ( 'NONE',  ( 0.03875523708678083740, -0.03329700455359455719, -0.4752403914626249226 ) ) ;
#2523 =( BOUNDED_SURFACE ( )  B_SPLINE_SURFACE ( 3, 2, ( 
 ( #4046, #2001, #13910 ),
 ( #36549, #14331, #1401 ),
 ( #26702, #29980, #36129 ),
 ( #26283, #5065, #14525 ),
 ( #30173, #26482, #1606 ),
 ( #27089, #23208, #20929 ),
 ( #17425, #33450, #5256 ),
 ( #39019, #33047, #14132 ),
 ( #8360, #17626, #24025 ),
 ( #11459, #20120, #7545 ) ),
 .UNSPECIFIED., .F., .F., .T. ) 
 B_SPLINE_SURFACE_WITH_KNOTS ( ( 4, 2, 2, 2, 4 ),
 ( 3, 3 ),
 ( -2.042636892962690354E-16, 0.0004458836822742874139, 0.0008917673645487790915, 0.001337651046823270769, 0.001783534729097762447 ),
 ( 0.000000000000000000, 1.000000000000000000 ),
 .UNSPECIFIED. ) 
 GEOMETRIC_REPRESENTATION_ITEM ( )  RATIONAL_B_SPLINE_SURFACE ( (
 ( 1.000000000000000000, 0.7270749630177930634, 1.000000000000000000),
 ( 1.000000000000000000, 0.7753295258064453188, 1.000000000000000000),
 ( 1.000000000000000000, 0.8134500463251533864, 1.000000000000000000),
 ( 1.000000000000000000, 0.8693879047592659726, 1.000000000000000000),
 ( 1.000000000000000000, 0.8872992176887145588, 1.000000000000000000),
 ( 1.000000000000000000, 0.9041895492973218706, 1.000000000000000000),
 ( 1.000000000000000000, 0.9028865482022944144, 1.000000000000000000),
 ( 1.000000000000000000, 0.8835743685064011421, 1.000000000000000000),
 ( 1.000000000000000000, 0.8656690658353223267, 1.000000000000000000),
 ( 1.000000000000000000, 0.8407181564551341468, 1.000000000000000000) ) ) 
 REPRESENTATION_ITEM ( '' )  SURFACE ( )  );
#2524 = DIRECTION ( 'NONE',  ( 1.000000000000000000, -0.000000000000000000, -0.000000000000000000 ) ) ;
#2525 = ORIENTED_EDGE ( 'NONE', *, *, #1880, .T. ) ;
#2526 = CARTESIAN_POINT ( 'NONE',  ( 0.6522089892707538805, -1.452491178199303956, 0.4224083929475448973 ) ) ;
#2527 = CARTESIAN_POINT ( 'NONE',  ( 0.004846577187571122179, -0.5767503433068859042, 0.3422196348096480656 ) ) ;
#2528 = ADVANCED_FACE ( 'NONE', ( #24678 ), #18474, .F. ) ;
#2529 = CARTESIAN_POINT ( 'NONE',  ( 0.5874265235786473305, -1.491095056082657466, 0.5633939987125622384 ) ) ;
#2531 = VERTEX_POINT ( 'NONE', #40494 ) ;
#2530 = DIRECTION ( 'NONE',  ( -1.355854680848614260E-31, 3.330669073875470114E-16, 1.000000000000000000 ) ) ;
#2532 = CARTESIAN_POINT ( 'NONE',  ( 0.6150013826522254812, -1.299199899150926374, 0.5044333340123036136 ) ) ;
#2534 = ORIENTED_EDGE ( 'NONE', *, *, #23489, .F. ) ;
#2533 = ORIENTED_EDGE ( 'NONE', *, *, #10248, .T. ) ;
#2535 = CARTESIAN_POINT ( 'NONE',  ( 0.6980568480161586375, -1.433467586945206929, 0.6380938078099552824 ) ) ;
#2536 = CYLINDRICAL_SURFACE ( 'NONE', #23761, 0.08139150547213644393 ) ;
#2537 = CYLINDRICAL_SURFACE ( 'NONE', #5527, 0.08139150547213643005 ) ;
#2538 = CALENDAR_DATE ( 2026, 13, 10 ) ;
#2539 = DIRECTION ( 'NONE',  ( 1.000000000000000000, 2.280301054154495132E-31, -1.664003471950577689E-31 ) ) ;
#2540 = ORIENTED_EDGE ( 'NONE', *, *, #26985, .F. ) ;
#2541 = CARTESIAN_POINT ( 'NONE',  ( 0.1323007547259467120, -0.7872386167069682639, 0.4801189427118005004 ) ) ;
#2542 = DIRECTION ( 'NONE',  ( -0.4999999999999955036, 0.7088756765536057269, 0.4974889699186023639 ) ) ;
#2543 = CARTESIAN_POINT ( 'NONE',  ( 0.4973151438122045964, -1.542462661965338766, 0.5710983407029659453 ) ) ;
#2545 = CARTESIAN_POINT ( 'NONE',  ( 0.07403655305110988516, -1.312857837003576833, 0.5491095645124061120 ) ) ;
#2544 = DIRECTION ( 'NONE',  ( 1.000000000000000000, 2.280301054154495132E-31, -1.664003471950577689E-31 ) ) ;
#2546 = CARTESIAN_POINT ( 'NONE',  ( 0.03174232663013761002, -1.011915959827874190, 0.5403155396012611078 ) ) ;
#2547 = EDGE_LOOP ( 'NONE', ( #27677, #37805, #21257, #21609 ) ) ;
#2548 = ORIENTED_EDGE ( 'NONE', *, *, #32777, .F. ) ;
#2549 = DIRECTION ( 'NONE',  ( -8.628166150854818811E-32, 0.1402348365093016580, 0.9901182710308954471 ) ) ;
#2550 = CARTESIAN_POINT ( 'NONE',  ( 0.4448084983678752269, -1.018341691379531344, 0.8445668428770941594 ) ) ;
#2551 = DIRECTION ( 'NONE',  ( 0.8660512985181134660, 0.4999551463232372317, 0.000000000000000000 ) ) ;
#2552 = CARTESIAN_POINT ( 'NONE',  ( -0.05464101615137770263, -2.542046649843399564, -0.2305290188067205537 ) ) ;
#2553 = DIRECTION ( 'NONE',  ( 1.000000000000000000, 2.280301054154495132E-31, -1.664003471950577689E-31 ) ) ;
#2554 = ADVANCED_FACE ( 'NONE', ( #14792 ), #34109, .T. ) ;
#2555 = DIRECTION ( 'NONE',  ( 0.8660512985181131329, 0.4999551463232376758, 0.000000000000000000 ) ) ;
#2556 = CARTESIAN_POINT ( 'NONE',  ( 0.2610261613789442992, -1.678452829011149561, 0.5218982752881765608 ) ) ;
#2557 = CARTESIAN_POINT ( 'NONE',  ( 0.3082562917470283437, -1.189540619778174380, 0.5196934755922930638 ) ) ;
#2558 = CARTESIAN_POINT ( 'NONE',  ( 0.5291583206849711507, -1.148825028536799131, 0.6606389499358795714 ) ) ;
#2559 = APPROVAL_STATUS ( 'not_yet_approved' ) ;
#2560 = DIRECTION ( 'NONE',  ( 0.000000000000000000, 0.000000000000000000, 1.000000000000000000 ) ) ;
#2561 = DIRECTION ( 'NONE',  ( 8.881784197001246407E-16, -2.361472542561082612E-16, 1.000000000000000000 ) ) ;
#2562 = DIRECTION ( 'NONE',  ( -0.4999999999999986677, 0.4254978411528150262, 0.7542887956043727860 ) ) ;
#2563 = FACE_OUTER_BOUND ( 'NONE', #39505, .T. ) ;
#2564 = ORIENTED_EDGE ( 'NONE', *, *, #36768, .F. ) ;
#2565 = CARTESIAN_POINT ( 'NONE',  ( 0.4679778500672936992, -1.237826332153874942, 0.6057417262809768888 ) ) ;
#2566 = CARTESIAN_POINT ( 'NONE',  ( -0.05615703521555030775, -0.2783003116137191535, 0.3655156233916935227 ) ) ;
#2567 = CARTESIAN_POINT ( 'NONE',  ( 0.1642982928013839161, -0.8629055878361323595, 0.5584950140652098494 ) ) ;
#2568 = ORIENTED_EDGE ( 'NONE', *, *, #40595, .T. ) ;
#2569 = CARTESIAN_POINT ( 'NONE',  ( -0.04140212552917817840, -0.01694508110950210950, -0.4702784328063241981 ) ) ;
#2570 = CARTESIAN_POINT ( 'NONE',  ( 0.02700589308869108529, -0.9048577289495857157, 0.5464201800401247144 ) ) ;
#2572 = EDGE_LOOP ( 'NONE', ( #37486, #6900 ) ) ;
#2571 = ORIENTED_EDGE ( 'NONE', *, *, #6884, .F. ) ;
#2573 = CARTESIAN_POINT ( 'NONE',  ( -0.1212602504878801113, -0.5073146173917535418, 0.1528658435936971483 ) ) ;
#2574 = CARTESIAN_POINT ( 'NONE',  ( 0.05279905671745407925, -0.03987410640504257531, 0.4667149812770405859 ) ) ;
#2575 = CARTESIAN_POINT ( 'NONE',  ( 0.04760578872587207383, -0.4700941947101299201, -0.1075272580797730498 ) ) ;
#2576 = CARTESIAN_POINT ( 'NONE',  ( 0.3569675822956203115, -1.858790014656386491, -0.3401391051804745769 ) ) ;
#2577 = CARTESIAN_POINT ( 'NONE',  ( 0.4567016086251121654, -1.219691737450557145, 0.6383600239578398616 ) ) ;
#2579 = CARTESIAN_POINT ( 'NONE',  ( 0.2043566422458189535, -1.364136262758315121, 0.5557375579486671935 ) ) ;
#2578 = CARTESIAN_POINT ( 'NONE',  ( 0.03874953289575387705, 0.4622846869243721901, 0.1151793484519291338 ) ) ;
#2580 = CARTESIAN_POINT ( 'NONE',  ( -0.05561176441985808683, -0.2541700551350222215, -0.3845131534397778772 ) ) ;
#2581 = ORIENTED_EDGE ( 'NONE', *, *, #33306, .T. ) ;
#2582 = CARTESIAN_POINT ( 'NONE',  ( 0.06588517883490634108, -1.329221574522195137, 0.5283365633529514271 ) ) ;
#2583 = VERTEX_POINT ( 'NONE', #31026 ) ;
#2584 = CARTESIAN_POINT ( 'NONE',  ( -0.2399999999999999079, -2.183180860297908144, -0.4937760292030871079 ) ) ;
#2585 = CARTESIAN_POINT ( 'NONE',  ( 0.3978516996529349870, -1.472654256470057987, 0.8275371935563656800 ) ) ;
#2587 = CARTESIAN_POINT ( 'NONE',  ( 0.5883754668686869138, -1.614204823230756203, 0.4538795894651435625 ) ) ;
#2586 = CARTESIAN_POINT ( 'NONE',  ( -0.01548846960707531660, -0.5198120922912100594, 0.07362328916748400731 ) ) ;
#2588 = CARTESIAN_POINT ( 'NONE',  ( 0.4952488905928924545, -1.196841907270136174, 0.4182417262808778013 ) ) ;
#2589 = CARTESIAN_POINT ( 'NONE',  ( 0.1996772853583087814, -2.073393704582455310, -0.6889727466378606779 ) ) ;
#2590 = VERTEX_POINT ( 'NONE', #24258 ) ;
#2591 = CARTESIAN_POINT ( 'NONE',  ( 0.4622815974667671690, -1.593090396639457396, -0.6012589109344715910 ) ) ;
#2592 = CARTESIAN_POINT ( 'NONE',  ( 0.3873602817592721181, -1.882673143022665752, -0.5129299851078027439 ) ) ;
#2593 = CARTESIAN_POINT ( 'NONE',  ( 0.2399483944973402061, -0.8897145941320553364, 0.6956011753531377018 ) ) ;
#2594 = CARTESIAN_POINT ( 'NONE',  ( 0.4640654899589395921, -1.684528450414659817, 0.4570323128730537365 ) ) ;
#2595 = CARTESIAN_POINT ( 'NONE',  ( 0.3999999999999787059, -2.097675824466503691, -0.4688691127277797022 ) ) ;
#2596 = ORIENTED_EDGE ( 'NONE', *, *, #24119, .F. ) ;
#2597 = CARTESIAN_POINT ( 'NONE',  ( 0.1614573949321077284, -0.7569534866611321577, 0.1932149833450299559 ) ) ;
#2598 = DIRECTION ( 'NONE',  ( 1.000000000000000000, -3.406373435249580326E-19, 7.771561172376097755E-16 ) ) ;
#2599 = CARTESIAN_POINT ( 'NONE',  ( -0.1443375672974067936, 0.000000000000000000, 0.000000000000000000 ) ) ;
#2600 = CARTESIAN_POINT ( 'NONE',  ( 0.1881571720199402276, -1.258443498167182817, 0.4308778177761442563 ) ) ;
#2601 = ADVANCED_FACE ( 'NONE', ( #36781 ), #37596, .T. ) ;
#2602 = EDGE_CURVE ( 'NONE', #7643, #23563, #29217, .T. ) ;
#2603 = CARTESIAN_POINT ( 'NONE',  ( 0.1895831464430141056, -0.5047047246472137205, 0.1457185332388698518 ) ) ;
#2604 = ADVANCED_FACE ( 'NONE', ( #2456 ), #5728, .T. ) ;
#2605 = CARTESIAN_POINT ( 'NONE',  ( -0.04211812644076948220, 0.2825523317586323135, 0.3743635450761847450 ) ) ;
#2606 = CARTESIAN_POINT ( 'NONE',  ( 0.009301758140802687466, -0.9958182297342890177, 0.5251311197228717420 ) ) ;
#2607 = EDGE_CURVE ( 'NONE', #25087, #617, #23867, .T. ) ;
#2608 = B_SPLINE_CURVE_WITH_KNOTS ( 'NONE', 3,
 ( #27469, #27873, #40411, #12236, #22316, #26019, #34437, #12844, #34833, #548, #19016, #6644, #28262, #31547, #16144, #31965, #22517, #941, #19217, #126, #32160, #9330, #3970, #35042, #6852, #35258, #28466, #18823, #3173, #29073, #9746, #13452, #19432, #12621 ),
 .UNSPECIFIED., .F., .F.,
 ( 4, 2, 2, 2, 2, 2, 2, 2, 2, 2, 2, 2, 2, 2, 2, 2, 4 ),
 ( 0.000000000000000000, 0.0006192929267342644345, 0.001238585853468528869, 0.001857878780202793303, 0.002477171706937057738, 0.003096464633671321739, 0.003715757560405590944, 0.004335050487139859715, 0.004954343413874128486, 0.005573636340608397258, 0.006192929267342666029, 0.006812222194076935668, 0.007431515120811204439, 0.008050808047545472343, 0.008670100974279741982, 0.009289393901014011620, 0.009908686827748279524 ),
 .UNSPECIFIED. ) ;
#2609 = CARTESIAN_POINT ( 'NONE',  ( 0.6479666109875431568, -1.454022938183795022, -0.4116638256851784528 ) ) ;
#2610 = LINE ( 'NONE', #34682, #17969 ) ;
#2611 = DIRECTION ( 'NONE',  ( 2.341930812374876608E-31, 0.6954292836768424246, -0.7185945389471826150 ) ) ;
#2612 = ADVANCED_FACE ( 'NONE', ( #18284 ), #1173, .F. ) ;
#2613 = DIRECTION ( 'NONE',  ( -1.000000000000000000, -0.000000000000000000, -0.000000000000000000 ) ) ;
#2614 = LINE ( 'NONE', #15575, #22565 ) ;
#2615 = ORIENTED_EDGE ( 'NONE', *, *, #6363, .T. ) ;
#2616 = CARTESIAN_POINT ( 'NONE',  ( 0.3593346688482155771, -1.735925422213635771, -0.5010936962835149666 ) ) ;
#2617 = CARTESIAN_POINT ( 'NONE',  ( 0.3920818884216891176, -1.687900591995562083, -0.6232001118445732457 ) ) ;
#2618 = B_SPLINE_CURVE_WITH_KNOTS ( 'NONE', 3,
 ( #29133, #7726, #13884, #23590, #26260, #32625, #26072, #26459, #7913, #16993 ),
 .UNSPECIFIED., .F., .F.,
 ( 4, 2, 2, 2, 4 ),
 ( 0.000000000000000000, 0.001019199890480618860, 0.002038399780961237719, 0.003057599671441856362, 0.004076799561922475439 ),
 .UNSPECIFIED. ) ;
#2619 = CARTESIAN_POINT ( 'NONE',  ( 0.4149016700121535006, -1.651544695139253172, -0.6216189332894249686 ) ) ;
#2620 = DIRECTION ( 'NONE',  ( 1.188678714063518227E-15, -1.000000000000000000, -3.263080277421930985E-16 ) ) ;
#2621 = VERTEX_POINT ( 'NONE', #9823 ) ;
#2622 = CARTESIAN_POINT ( 'NONE',  ( 0.4957703318102697487, -1.693058430341604081, -0.5958887926595133333 ) ) ;
#2623 = ADVANCED_FACE ( 'NONE', ( #34922 ), #19097, .T. ) ;
#2624 = CARTESIAN_POINT ( 'NONE',  ( 0.3249540854508322085, -1.179364160644205128, 0.5783250968866978647 ) ) ;
#2625 = DIRECTION ( 'NONE',  ( -1.000000000000000000, -0.000000000000000000, -0.000000000000000000 ) ) ;
#2626 = PRODUCT_DEFINITION ( 'UNKNOWN', '', #36468, #7610 ) ;
#2627 = CARTESIAN_POINT ( 'NONE',  ( 0.02872242845529807825, 0.3729171224323813982, -0.3802687114177593641 ) ) ;
#2628 = CARTESIAN_POINT ( 'NONE',  ( 0.4423174438215108362, -1.206761583220333778, 0.7319083686835440306 ) ) ;
#2630 = VERTEX_POINT ( 'NONE', #13317 ) ;
#2629 = CARTESIAN_POINT ( 'NONE',  ( -0.1642263572652579717, 0.5103503757440955857, 0.1470331037154087028 ) ) ;
#2631 = CARTESIAN_POINT ( 'NONE',  ( 0.4756538103953397711, -1.077424610118791648, 0.6442006390088441670 ) ) ;
#2632 = ORIENTED_EDGE ( 'NONE', *, *, #17439, .T. ) ;
#2633 = APPROVAL_STATUS ( 'not_yet_approved' ) ;
#2634 = FACE_BOUND ( 'NONE', #15881, .T. ) ;
#2635 = ORIENTED_EDGE ( 'NONE', *, *, #1995, .T. ) ;
#2636 = CARTESIAN_POINT ( 'NONE',  ( 0.009578720288114734097, -0.5684218271147216672, 0.04142997145147423593 ) ) ;
#2637 = ORIENTED_EDGE ( 'NONE', *, *, #30387, .F. ) ;
#2638 = CARTESIAN_POINT ( 'NONE',  ( 0.3561794159690685468, -1.622419985511465823, 0.5747848533733730392 ) ) ;
#2640 = CARTESIAN_POINT ( 'NONE',  ( 0.1761160692862425159, -0.6130882321663837509, -0.07245465855189868465 ) ) ;
#2639 = CARTESIAN_POINT ( 'NONE',  ( 0.06495584141124570443, -0.8202245329731961965, 0.08014687577841178578 ) ) ;
#2641 = DIRECTION ( 'NONE',  ( 0.8660512985181126888, 0.4999551463232384529, 0.000000000000000000 ) ) ;
#2642 = CIRCLE ( 'NONE', #28327, 0.01500000000000003934 ) ;
#2643 = VERTEX_POINT ( 'NONE', #6728 ) ;
#2644 = CARTESIAN_POINT ( 'NONE',  ( 0.4530449344480740881, -1.054480797917887180, 0.7183760019440903477 ) ) ;
#2645 = CARTESIAN_POINT ( 'NONE',  ( 0.1164452680309506771, -0.5621043433723575955, 0.2200809357625567453 ) ) ;
#2646 = ORIENTED_EDGE ( 'NONE', *, *, #20141, .T. ) ;
#2647 = CARTESIAN_POINT ( 'NONE',  ( 0.2189962940802840652, -1.687333423092645779, -0.3582481089917773365 ) ) ;
#2648 = DIRECTION ( 'NONE',  ( -0.4999551463232372317, 0.8660512985181135770, -0.000000000000000000 ) ) ;
#2649 = CIRCLE ( 'NONE', #15109, 0.03000000000000029379 ) ;
#2650 = CARTESIAN_POINT ( 'NONE',  ( 0.5970072641691556159, -1.484358014203126297, -0.4176640727536428677 ) ) ;
#2651 = CARTESIAN_POINT ( 'NONE',  ( 0.4420022301528255815, -1.686445855772801705, 0.4182417262808776903 ) ) ;
#2652 = EDGE_CURVE ( 'NONE', #19627, #30237, #31718, .T. ) ;
#2653 = CARTESIAN_POINT ( 'NONE',  ( 0.3091361241754520539, -1.774399086135407533, 0.3157417262808776548 ) ) ;
#2654 = DIRECTION ( 'NONE',  ( 0.8660512985181135770, 0.4999551463232371762, 0.000000000000000000 ) ) ;
#2655 = CARTESIAN_POINT ( 'NONE',  ( 0.09667290451365230519, -1.302890901820756620, -0.6687017097452528924 ) ) ;
#2656 = CARTESIAN_POINT ( 'NONE',  ( -0.2600000000000002309, 0.5182417262804744906, 0.3749999999999995559 ) ) ;
#2657 = DATE_TIME_ROLE ( 'classification_date' ) ;
#2658 = EDGE_CURVE ( 'NONE', #6212, #23907, #37109, .T. ) ;
#2659 = CARTESIAN_POINT ( 'NONE',  ( 0.4792622942854181112, -1.127254429899091637, 0.4859857865428779400 ) ) ;
#2660 = EDGE_CURVE ( 'NONE', #11781, #10668, #11478, .T. ) ;
#2661 = CARTESIAN_POINT ( 'NONE',  ( 0.02869712619511899723, -0.4892154842446472252, 0.09550911579581831956 ) ) ;
#2662 = DIRECTION ( 'NONE',  ( 0.8660512985181134660, 0.4999551463232372317, 0.000000000000000000 ) ) ;
#2663 = CARTESIAN_POINT ( 'NONE',  ( 0.08897272204609851798, -1.263855944153051469, 0.7613784839713820807 ) ) ;
#2664 = CARTESIAN_POINT ( 'NONE',  ( 0.3268505546336938905, -1.758215942194889969, 0.4787252747007004205 ) ) ;
#2665 = CARTESIAN_POINT ( 'NONE',  ( 0.0005306896791119474367, -0.4438826107187291981, 0.2002152464016503652 ) ) ;
#2666 = AXIS2_PLACEMENT_3D ( 'NONE', #25305, #28786, #25503 ) ;
#2667 = CARTESIAN_POINT ( 'NONE',  ( 0.1943613428509314289, -1.255083190917881675, -0.3178470422210406543 ) ) ;
#2668 = ORIENTED_EDGE ( 'NONE', *, *, #15423, .F. ) ;
#2669 = EDGE_LOOP ( 'NONE', ( #39297, #28607, #28151, #9412, #11173 ) ) ;
#2670 = CIRCLE ( 'NONE', #8556, 0.5215209409081880132 ) ;
#2671 = EDGE_CURVE ( 'NONE', #31622, #14323, #1005, .T. ) ;
#2672 = CARTESIAN_POINT ( 'NONE',  ( -0.1190772264498593247, -0.4967457283353788888, 0.1275078045371980107 ) ) ;
#2673 = EDGE_LOOP ( 'NONE', ( #19685, #31629, #23451, #6716 ) ) ;
#2674 = CYLINDRICAL_SURFACE ( 'NONE', #13172, 0.03000000000000008910 ) ;
#2675 = VECTOR ( 'NONE', #14935, 39.37007874015748143 ) ;
#2676 = CARTESIAN_POINT ( 'NONE',  ( -0.1056392956507297559, -0.4804620820570389972, 0.09550516425354510508 ) ) ;
#2678 = ORIENTED_EDGE ( 'NONE', *, *, #17977, .T. ) ;
#2677 = CARTESIAN_POINT ( 'NONE',  ( 0.2059273467974228333, -1.283046334493783025, -0.7462941026102624109 ) ) ;
#2679 = ORIENTED_EDGE ( 'NONE', *, *, #3341, .F. ) ;
#2680 = DIRECTION ( 'NONE',  ( -1.355854680848614260E-31, 3.330669073875470114E-16, 1.000000000000000000 ) ) ;
#2681 = ORIENTED_EDGE ( 'NONE', *, *, #2886, .F. ) ;
#2682 = CARTESIAN_POINT ( 'NONE',  ( -0.001068161708947345471, -0.5484958227261149677, 0.2458947828252880385 ) ) ;
#2684 = CARTESIAN_POINT ( 'NONE',  ( -0.08000000000000000167, -2.626773565144302935, -0.2726934094652516127 ) ) ;
#2683 = CARTESIAN_POINT ( 'NONE',  ( 0.4962914637724937794, -1.692757590648997557, -0.4193976862638447711 ) ) ;
#2685 = CARTESIAN_POINT ( 'NONE',  ( 0.3669101237188617803, -1.155878863020100011, 0.4953911018533934674 ) ) ;
#2686 = COORDINATED_UNIVERSAL_TIME_OFFSET ( 0, 0, .AHEAD. ) ;
#2688 = ORIENTED_EDGE ( 'NONE', *, *, #5019, .F. ) ;
#2687 = ORIENTED_EDGE ( 'NONE', *, *, #15745, .T. ) ;
#2689 = CARTESIAN_POINT ( 'NONE',  ( 0.08565325978148723152, -0.8127617527064519010, 0.1840195686883785431 ) ) ;
#2690 = CARTESIAN_POINT ( 'NONE',  ( 0.3655313958116495621, -1.732873032179087058, 0.4268294808601417190 ) ) ;
#2691 = CARTESIAN_POINT ( 'NONE',  ( -0.04087116408466824613, -0.4416914123362196687, 0.1656680454788615198 ) ) ;
#2692 = CARTESIAN_POINT ( 'NONE',  ( 0.4796062271711729608, -1.296889239581610731, 0.8144315461438738080 ) ) ;
#2693 = CARTESIAN_POINT ( 'NONE',  ( 0.5965761245944036784, -1.493465029535157029, 0.5182417262812423209 ) ) ;
#2694 = CARTESIAN_POINT ( 'NONE',  ( 0.2741618706575962294, -1.669228526676626245, 0.6701936342721495077 ) ) ;
#2695 = CIRCLE ( 'NONE', #4634, 0.1400000000000009570 ) ;
#2696 = CARTESIAN_POINT ( 'NONE',  ( 0.3203399455593453071, -1.760717822755525797, 0.5904099678045555688 ) ) ;
#2697 = CARTESIAN_POINT ( 'NONE',  ( 0.4139549699696334351, -1.708531266749635069, 0.4267841496025627790 ) ) ;
#2698 = CARTESIAN_POINT ( 'NONE',  ( 0.3965728918691002192, -1.716106284337745702, 0.4221472374420881524 ) ) ;
#2699 = ADVANCED_FACE ( 'NONE', ( #10246 ), #619, .T. ) ;
#2700 = CIRCLE ( 'NONE', #33545, 0.1033070866141734129 ) ;
#2701 = CARTESIAN_POINT ( 'NONE',  ( 0.2906430027847833331, -0.9902279025455028583, 0.7333702739393529457 ) ) ;
#2702 = CARTESIAN_POINT ( 'NONE',  ( 0.4650638207231214127, -1.115967253294534167, 0.5748459061576319806 ) ) ;
#2703 = CARTESIAN_POINT ( 'NONE',  ( -0.02000000000000000042, -2.577535374323032702, -0.2789082543815905590 ) ) ;
#2704 = LENGTH_MEASURE_WITH_UNIT ( LENGTH_MEASURE( 0.02539999999999999897 ), #18340 );
#2705 = AXIS2_PLACEMENT_3D ( 'NONE', #33179, #7856, #26815 ) ;
#2706 = EDGE_CURVE ( 'NONE', #4081, #38935, #5529, .T. ) ;
#2707 = DIRECTION ( 'NONE',  ( 0.000000000000000000, 2.964295475749157234E-14, 1.000000000000000000 ) ) ;
#2708 = CARTESIAN_POINT ( 'NONE',  ( 0.008416785622808892545, -0.6338120178247520498, 0.4051738709354697487 ) ) ;
#2709 = CARTESIAN_POINT ( 'NONE',  ( 0.07627944499376293486, -1.206878283085004444, 0.7625613511206872364 ) ) ;
#2710 = PERSON_AND_ORGANIZATION ( #28500, #32463 ) ;
#2711 = CARTESIAN_POINT ( 'NONE',  ( 0.4514527476588715560, -1.032880248282614266, 0.8272311760340308462 ) ) ;
#2712 = EDGE_CURVE ( 'NONE', #6499, #34235, #22814, .T. ) ;
#2713 = DIRECTION ( 'NONE',  ( 0.000000000000000000, 0.9343694307158671997, -0.3563057211773426602 ) ) ;
#2714 = CARTESIAN_POINT ( 'NONE',  ( 0.01548846960706645737, 0.07651041855119844470, -0.5222379212568389883 ) ) ;
#2715 = ADVANCED_FACE ( 'NONE', ( #34718 ), #16403, .F. ) ;
#2716 = CARTESIAN_POINT ( 'NONE',  ( 0.3447589852832846913, -1.668942397003103650, -0.4516098998207526694 ) ) ;
#2717 = ORIENTED_EDGE ( 'NONE', *, *, #15763, .T. ) ;
#2718 = CARTESIAN_POINT ( 'NONE',  ( 0.1999999999999789724, -2.183180860297921466, -0.2437760292030870524 ) ) ;
#2719 = CARTESIAN_POINT ( 'NONE',  ( 0.2424357324133526170, -1.539388940635932457, 0.9028508052754699031 ) ) ;
#2720 = EDGE_CURVE ( 'NONE', #13521, #23751, #10803, .T. ) ;
#2721 = CIRCLE ( 'NONE', #18488, 0.1946589359789743512 ) ;
#2722 = CARTESIAN_POINT ( 'NONE',  ( 0.5284083360280649178, -1.405426350308686345, 0.7820653062704271408 ) ) ;
#2724 = ORIENTED_EDGE ( 'NONE', *, *, #1929, .F. ) ;
#2723 = CARTESIAN_POINT ( 'NONE',  ( 0.3546403334084172743, -1.742554324808940347, 0.4373760386089020624 ) ) ;
#2725 = EDGE_CURVE ( 'NONE', #1334, #8744, #25950, .T. ) ;
#2726 = CARTESIAN_POINT ( 'NONE',  ( 0.5556047631917466756, -1.190343314783628870, 0.5823040822259395455 ) ) ;
#2728 = ORIENTED_EDGE ( 'NONE', *, *, #38593, .F. ) ;
#2727 = ORIENTED_EDGE ( 'NONE', *, *, #7131, .T. ) ;
#2729 = CARTESIAN_POINT ( 'NONE',  ( 0.4837496661226462491, -1.089885176164768765, 0.8053770729510393300 ) ) ;
#2730 = CONICAL_SURFACE ( 'NONE', #23767, 0.5515209409081860414, 1.047197551196597409 ) ;
#2731 = DIRECTION ( 'NONE',  ( 0.000000000000000000, 0.000000000000000000, -1.000000000000000000 ) ) ;
#2732 = TOROIDAL_SURFACE ( 'NONE', #716, 0.5250000000000000222, 0.01499999999999999944 ) ;
#2733 = CARTESIAN_POINT ( 'NONE',  ( -0.01548846960712763066, 0.4730347584885825629, 0.2341461249029053171 ) ) ;
#2734 = CARTESIAN_POINT ( 'NONE',  ( 0.5536297569049346556, -1.186194075236972179, 0.6057417262809815517 ) ) ;
#2735 = EDGE_LOOP ( 'NONE', ( #13647, #1933, #16103, #29692 ) ) ;
#2736 = B_SPLINE_CURVE_WITH_KNOTS ( 'NONE', 3,
 ( #2295, #8443, #37036, #33746, #36219, #17700, #4951, #5558, #33338, #23693 ),
 .UNSPECIFIED., .F., .F.,
 ( 4, 2, 2, 2, 4 ),
 ( 0.001421410091499676447, 0.001776295181873929763, 0.002131180272248183079, 0.002486065362622435961, 0.002840950452996689277 ),
 .UNSPECIFIED. ) ;
#2737 = CARTESIAN_POINT ( 'NONE',  ( 0.1116805044116661316, -0.7434698432209100316, 0.4023817199705208569 ) ) ;
#2738 = DIRECTION ( 'NONE',  ( -0.000000000000000000, -0.3882559824134205750, 0.9215515678030121727 ) ) ;
#2739 = CARTESIAN_POINT ( 'NONE',  ( 0.1049838256438099249, -0.5659121791580637995, 0.2385271282840315255 ) ) ;
#2741 = CARTESIAN_POINT ( 'NONE',  ( 0.06581764578086118922, -1.340728352476674212, 0.5449258910593480776 ) ) ;
#2740 = CARTESIAN_POINT ( 'NONE',  ( 0.3172915166155709232, -1.763408040713600577, 0.5249560652895838286 ) ) ;
#2742 = CARTESIAN_POINT ( 'NONE',  ( -0.05283102792148802046, -0.3063958269170686255, 0.3541938269410537243 ) ) ;
#2743 = ORIENTED_EDGE ( 'NONE', *, *, #22017, .F. ) ;
#2744 = CARTESIAN_POINT ( 'NONE',  ( 0.4694680599816452027, -1.673450296079499466, 0.5834365554883687022 ) ) ;
#2745 = CARTESIAN_POINT ( 'NONE',  ( 0.2329990834885074247, -0.7658510446276335371, 0.7180707385985112268 ) ) ;
#2746 = DIRECTION ( 'NONE',  ( 0.000000000000000000, 0.000000000000000000, -1.000000000000000000 ) ) ;
#2747 = DIRECTION ( 'NONE',  ( 0.000000000000000000, 0.000000000000000000, -1.000000000000000000 ) ) ;
#2748 = SHAPE_REPRESENTATION_RELATIONSHIP ( 'NONE' , 'NONE' ,  #8026, #11298 ) ;
#2749 = CIRCLE ( 'NONE', #25756, 0.01500000000000005322 ) ;
#2750 = ADVANCED_FACE ( 'NONE', ( #1814 ), #12136, .T. ) ;
#2751 = DIRECTION ( 'NONE',  ( -0.4999551463232372317, 0.8660512985181135770, -0.000000000000000000 ) ) ;
#2752 = LINE ( 'NONE', #15302, #31810 ) ;
#2753 = ADVANCED_FACE ( 'NONE', ( #15560 ), #13441, .T. ) ;
#2754 = CARTESIAN_POINT ( 'NONE',  ( 0.05999999999999990757, 0.000000000000000000, 0.000000000000000000 ) ) ;
#2755 = CARTESIAN_POINT ( 'NONE',  ( 0.1967848402874973202, -0.7048484731626001309, 0.3032743993732655574 ) ) ;
#2756 = PERSON_AND_ORGANIZATION_ROLE ( 'classification_officer' ) ;
#2757 = VECTOR ( 'NONE', #18322, 39.37007874015748143 ) ;
#2758 =( BOUNDED_SURFACE ( )  B_SPLINE_SURFACE ( 3, 2, ( 
 ( #19857, #25632, #16366 ),
 ( #385, #22557, #28904 ),
 ( #4003, #37973, #10393 ),
 ( #770, #22956, #9783 ),
 ( #38758, #1174, #13276 ),
 ( #29329, #32391, #13675 ),
 ( #38163, #15962, #28722 ),
 ( #10589, #25844, #22353 ),
 ( #9987, #19053, #23163 ),
 ( #6484, #31590, #3406 ) ),
 .UNSPECIFIED., .F., .F., .T. ) 
 B_SPLINE_SURFACE_WITH_KNOTS ( ( 4, 2, 2, 2, 4 ),
 ( 3, 3 ),
 ( 0.01180411870105455355, 0.01260860704157424489, 0.01341309538209393623, 0.01421758372261362757, 0.01502207206313332065 ),
 ( 0.000000000000000000, 0.6794541557782065588 ),
 .UNSPECIFIED. ) 
 GEOMETRIC_REPRESENTATION_ITEM ( )  RATIONAL_B_SPLINE_SURFACE ( (
 ( 1.000000000000000000, 0.8005432181983026529, 0.8721299149832257847),
 ( 1.000000000000000000, 0.8005023781569950980, 0.8721037327721876675),
 ( 1.000000000000000000, 0.8004856833031734897, 0.8720930298401630143),
 ( 1.000000000000000000, 0.8004816785315187477, 0.8720904624143410722),
 ( 1.000000000000000000, 0.8004939698596951203, 0.8720983422826746878),
 ( 1.000000000000000000, 0.8005299687168438982, 0.8721214208507863663),
 ( 1.000000000000000000, 0.8005535718565474079, 0.8721365526274713620),
 ( 1.000000000000000000, 0.8006044241474448153, 0.8721691536085041108),
 ( 1.000000000000000000, 0.8006320503125461396, 0.8721868645133341591),
 ( 1.000000000000000000, 0.8006591322813667588, 0.8722042265384517545) ) ) 
 REPRESENTATION_ITEM ( '' )  SURFACE ( )  );
#2759 = CIRCLE ( 'NONE', #34286, 0.01499999999999999424 ) ;
#2760 = CARTESIAN_POINT ( 'NONE',  ( 0.1734973056165642902, -1.209394307038482497, -0.5155029497116575543 ) ) ;
#2761 = AXIS2_PLACEMENT_3D ( 'NONE', #8730, #15720, #134 ) ;
#2762 = DIRECTION ( 'NONE',  ( 1.000000000000000000, 1.450080480853946466E-15, -8.359287477863926836E-16 ) ) ;
#2763 = CARTESIAN_POINT ( 'NONE',  ( 0.5846118587689395074, -1.493149640613376627, 0.5722307761754854560 ) ) ;
#2764 = LINE ( 'NONE', #33611, #32435 ) ;
#2765 = ORIENTED_EDGE ( 'NONE', *, *, #7608, .T. ) ;
#2766 = DIRECTION ( 'NONE',  ( 1.000000000000000000, 0.000000000000000000, 0.000000000000000000 ) ) ;
#2767 = CARTESIAN_POINT ( 'NONE',  ( -0.08000000000000000167, -2.198867511061768809, -0.9423512173156428640 ) ) ;
#2768 = CARTESIAN_POINT ( 'NONE',  ( 0.1948208630905133021, -0.8880093436342747504, 0.6128872966510791054 ) ) ;
#2769 = VERTEX_POINT ( 'NONE', #17812 ) ;
#2770 = CARTESIAN_POINT ( 'NONE',  ( -0.05138886601528149661, -0.02227547295148940218, -0.4715784802958458699 ) ) ;
#2771 = CARTESIAN_POINT ( 'NONE',  ( 0.06357782896711253184, -1.038394445277960987, 0.7229233463101174539 ) ) ;
#2773 = EDGE_LOOP ( 'NONE', ( #36991, #11699, #3234, #14701 ) ) ;
#2772 = VERTEX_POINT ( 'NONE', #36945 ) ;
#2774 = CARTESIAN_POINT ( 'NONE',  ( -0.1163549140004252191, -0.5320595946631425655, 0.1429098354137926519 ) ) ;
#2775 = VERTEX_POINT ( 'NONE', #40023 ) ;
#2776 = CARTESIAN_POINT ( 'NONE',  ( 0.04285427992854268925, -0.07198917448059444224, 0.4895546022328310931 ) ) ;
#2777 = CARTESIAN_POINT ( 'NONE',  ( 0.7409681548321257472, -1.515722218252784748, 0.5271419462256154986 ) ) ;
#2778 = CARTESIAN_POINT ( 'NONE',  ( 0.3583460058031623929, -1.906970946538292910, -0.5088717446659136723 ) ) ;
#2779 = DIRECTION ( 'NONE',  ( 0.000000000000000000, 0.000000000000000000, -1.000000000000000000 ) ) ;
#2780 = TOROIDAL_SURFACE ( 'NONE', #4723, 0.6154198107346402491, 0.7750185148639454624 ) ;
#2782 = CARTESIAN_POINT ( 'NONE',  ( 0.2211959769661342168, -1.309495541150525799, -0.2869361388274796476 ) ) ;
#2781 = CARTESIAN_POINT ( 'NONE',  ( -0.1141309172362121732, 0.06118878220587060240, 0.05231945263244267008 ) ) ;
#2783 = CARTESIAN_POINT ( 'NONE',  ( 0.04047170147976334592, -0.3430616206016776637, -0.3654769923554794797 ) ) ;
#2784 = ORIENTED_EDGE ( 'NONE', *, *, #22552, .F. ) ;
#2785 = CARTESIAN_POINT ( 'NONE',  ( -0.01548846960707490547, 0.09319974324249648279, 0.5318964258758775987 ) ) ;
#2786 = VERTEX_POINT ( 'NONE', #39622 ) ;
#2787 = AXIS2_PLACEMENT_3D ( 'NONE', #37656, #37254, #15455 ) ;
#2788 = CARTESIAN_POINT ( 'NONE',  ( 0.05999999999999990757, 0.2217800815169825301, -0.07875759618522079619 ) ) ;
#2789 = VECTOR ( 'NONE', #15660, 39.37007874015748143 ) ;
#2790 = CARTESIAN_POINT ( 'NONE',  ( 0.07310625969965998949, -0.5492403936048265711, 0.2026465080310040634 ) ) ;
#2792 = CARTESIAN_POINT ( 'NONE',  ( 0.5998866944813456836, -1.596483326503712163, 0.4395608873836986397 ) ) ;
#2791 = CARTESIAN_POINT ( 'NONE',  ( -0.1167294259372886195, -0.5331983348239496268, 0.1476740372344541030 ) ) ;
#2793 = CARTESIAN_POINT ( 'NONE',  ( 0.4661714095618022524, -1.154128127646582458, 0.4228544605197694373 ) ) ;
#2794 = CARTESIAN_POINT ( 'NONE',  ( 0.1575440928747191827, -1.280321311252621497, -0.3327596545001944017 ) ) ;
#2795 = CIRCLE ( 'NONE', #20507, 0.01500000000000004802 ) ;
#2796 = CARTESIAN_POINT ( 'NONE',  ( -0.2399999999999999079, -2.139295658456680904, -0.2024034539465678073 ) ) ;
#2797 = CARTESIAN_POINT ( 'NONE',  ( 0.3977485604613671955, -1.756321122263676093, -0.3111787470529240873 ) ) ;
#2798 = CARTESIAN_POINT ( 'NONE',  ( 0.1427444512807377885, -0.6541520024106974862, 0.4271693757410587322 ) ) ;
#2799 = CARTESIAN_POINT ( 'NONE',  ( 0.4778399605452497423, -1.666371875539310432, 0.5376480933357082881 ) ) ;
#2800 = DIRECTION ( 'NONE',  ( -0.4999551463232372317, 0.8660512985181135770, -0.000000000000000000 ) ) ;
#2801 = VERTEX_POINT ( 'NONE', #11846 ) ;
#2802 = CARTESIAN_POINT ( 'NONE',  ( -0.03662792686184404567, 0.4431041838557920332, 0.1872093443778342081 ) ) ;
#2803 = PLANE ( 'NONE',  #22550 ) ;
#2804 = DIRECTION ( 'NONE',  ( -1.000000000000000000, -2.341930812374887555E-31, 1.664003471950578127E-31 ) ) ;
#2805 = CARTESIAN_POINT ( 'NONE',  ( -0.2299999999999999267, 0.5182417262804744906, 0.09999999999999989453 ) ) ;
#2806 = CARTESIAN_POINT ( 'NONE',  ( 0.6116693357450743163, -1.291191393066782211, 0.8405059385265429839 ) ) ;
#2807 = CARTESIAN_POINT ( 'NONE',  ( -0.03170752374382458660, 0.2433701302032824365, 0.4274053688542782670 ) ) ;
#2808 = CARTESIAN_POINT ( 'NONE',  ( 0.02620755023972913891, -1.037821530677986992, 0.5805157883271023778 ) ) ;
#2809 = AXIS2_PLACEMENT_3D ( 'NONE', #31198, #9364, #21943 ) ;
#2810 = DIRECTION ( 'NONE',  ( 1.000000000000000000, 1.138269997360101095E-15, -8.537024980200757723E-16 ) ) ;
#2811 = LINE ( 'NONE', #18038, #1576 ) ;
#2812 = CARTESIAN_POINT ( 'NONE',  ( 0.08740683213217560754, -0.8118925016582974052, 0.2366527497468325636 ) ) ;
#2813 = CARTESIAN_POINT ( 'NONE',  ( 0.07216878364870311924, 0.05141091571461162829, 0.1249999999999999029 ) ) ;
#2814 = CARTESIAN_POINT ( 'NONE',  ( 0.3699999999999786793, -2.166079853131637645, -0.4467913981637915422 ) ) ;
#2815 = CIRCLE ( 'NONE', #25823, 0.07499999999999977518 ) ;
#2816 = AXIS2_PLACEMENT_3D ( 'NONE', #30224, #5126, #9044 ) ;
#2817 = EDGE_LOOP ( 'NONE', ( #37631, #37371, #35607, #37980 ) ) ;
#2818 = CARTESIAN_POINT ( 'NONE',  ( 0.5843377990077387452, -1.469343909573061158, -0.6034783832058462361 ) ) ;
#2819 = CIRCLE ( 'NONE', #32347, 0.1033070866141734129 ) ;
#2820 = CARTESIAN_POINT ( 'NONE',  ( -0.08000000000000000167, -2.551729310907437043, -0.5086726180052709712 ) ) ;
#2821 = VECTOR ( 'NONE', #21632, 39.37007874015748143 ) ;
#2822 = ORIENTED_EDGE ( 'NONE', *, *, #15988, .T. ) ;
#2823 = CARTESIAN_POINT ( 'NONE',  ( 0.5335660117596170426, -1.671239694278476628, -0.5770658812888499467 ) ) ;
#2824 = AXIS2_PLACEMENT_3D ( 'NONE', #26102, #6528, #1215 ) ;
#2825 = CARTESIAN_POINT ( 'NONE',  ( 0.7059656540691128246, -1.571716619208481935, -0.5155029497116575543 ) ) ;
#2826 = DIRECTION ( 'NONE',  ( -1.000000000000000000, -7.857794173099924470E-32, -8.628166150854818811E-32 ) ) ;
#2827 = DIRECTION ( 'NONE',  ( -1.000000000000000000, -1.138269997360101095E-15, 1.138269997360101095E-15 ) ) ;
#2828 = CARTESIAN_POINT ( 'NONE',  ( 0.5105415332760498970, -1.310647974363944090, 0.6145840706319117830 ) ) ;
#2830 = ORIENTED_EDGE ( 'NONE', *, *, #10049, .F. ) ;
#2829 = CARTESIAN_POINT ( 'NONE',  ( -2.112273405726188513E-14, -2.097675824466503691, -0.4937760292030871079 ) ) ;
#2831 = CARTESIAN_POINT ( 'NONE',  ( 0.3550881284155063544, -0.9867921891001451007, 0.6236314015414725631 ) ) ;
#2832 = ORIENTED_EDGE ( 'NONE', *, *, #17594, .T. ) ;
#2833 = PERSON_AND_ORGANIZATION_ROLE ( 'creator' ) ;
#2834 = CARTESIAN_POINT ( 'NONE',  ( 0.1052201234866705776, -1.408655232269138358, 0.5916332308596470302 ) ) ;
#2835 = VERTEX_POINT ( 'NONE', #30778 ) ;
#2836 = ORIENTED_EDGE ( 'NONE', *, *, #37298, .F. ) ;
#2837 = CARTESIAN_POINT ( 'NONE',  ( 0.07484919615358114064, -0.7926208454270931014, 0.6479314650129559539 ) ) ;
#2839 = CARTESIAN_POINT ( 'NONE',  ( 0.1136133567237439662, -0.6088964843684741002, -0.08269403125744159699 ) ) ;
#2838 = DIRECTION ( 'NONE',  ( 0.5000000000000019984, 0.4646411234949395785, -0.7308273574226392677 ) ) ;
#2840 = DIRECTION ( 'NONE',  ( -1.000000000000000000, -6.779273404243070203E-32, -4.314083075427408311E-32 ) ) ;
#2841 = TOROIDAL_SURFACE ( 'NONE', #31126, 0.05330708661417323663, 0.01000000000000000021 ) ;
#2842 = VERTEX_POINT ( 'NONE', #15348 ) ;
#2843 = ORIENTED_EDGE ( 'NONE', *, *, #1771, .F. ) ;
#2844 = CARTESIAN_POINT ( 'NONE',  ( 0.4773881915714036639, -1.084785724581697863, 0.7107894162981950315 ) ) ;
#2845 = ADVANCED_FACE ( 'NONE', ( #33650, #30584 ), #5862, .F. ) ;
#2846 = CARTESIAN_POINT ( 'NONE',  ( 0.2807752934945104695, -1.015156109853498023, 0.7786345481072077801 ) ) ;
#2847 = ORIENTED_EDGE ( 'NONE', *, *, #15014, .F. ) ;
#2848 = CARTESIAN_POINT ( 'NONE',  ( 0.4015936175283410514, -1.155705023113092533, 0.5182417262812423209 ) ) ;
#2849 = CARTESIAN_POINT ( 'NONE',  ( 0.000000000000000000, -0.4700000000000001954, 0.000000000000000000 ) ) ;
#2850 = VECTOR ( 'NONE', #9839, 39.37007874015748143 ) ;
#2851 = VECTOR ( 'NONE', #17766, 39.37007874015748143 ) ;
#2852 = CARTESIAN_POINT ( 'NONE',  ( 0.5774070013789848188, -1.563126340145571058, -0.4407173397374128387 ) ) ;
#2853 = CARTESIAN_POINT ( 'NONE',  ( -0.1190701091186102401, -0.4967104654273956088, 0.3286746847624749668 ) ) ;
#2854 = AXIS2_PLACEMENT_3D ( 'NONE', #32552, #20631, #35850 ) ;
#2855 = DIRECTION ( 'NONE',  ( -0.4999999999999986677, 0.8653188367530366687, 0.03497585968025478109 ) ) ;
#2856 = CARTESIAN_POINT ( 'NONE',  ( 0.7483483892508734359, -1.515136533364971339, 0.3157417262808776548 ) ) ;
#2857 = DIRECTION ( 'NONE',  ( -1.000000000000000000, -0.000000000000000000, -0.000000000000000000 ) ) ;
#2858 = EDGE_CURVE ( 'NONE', #30450, #23564, #11102, .T. ) ;
#2859 = LINE ( 'NONE', #34728, #29966 ) ;
#2860 = LINE ( 'NONE', #2656, #25294 ) ;
#2861 = APPROVAL_ROLE ( '' ) ;
#2862 = APPLIED_PERSON_AND_ORGANIZATION_ASSIGNMENT ( #23532, #20233, ( #39117 ) ) ;
#2863 = CARTESIAN_POINT ( 'NONE',  ( 0.2615876942762666579, -0.9557769062746830357, 0.5027841231788432452 ) ) ;
#2864 = CARTESIAN_POINT ( 'NONE',  ( 0.4673658794513684822, -1.111510721115457123, 0.5568865556175225384 ) ) ;
#2865 = CARTESIAN_POINT ( 'NONE',  ( 0.4480069854757587899, -1.224024607427070199, 0.6057417262810179670 ) ) ;
#2866 = CARTESIAN_POINT ( 'NONE',  ( 0.01548846960707524721, 0.000000000000000000, 0.000000000000000000 ) ) ;
#2867 = CARTESIAN_POINT ( 'NONE',  ( 0.007928552535923857544, -0.8847668029847218785, 0.5082548692313750838 ) ) ;
#2868 = CARTESIAN_POINT ( 'NONE',  ( 0.2722331219925429036, -1.671874623808670135, 0.4849083929475441201 ) ) ;
#2869 = CIRCLE ( 'NONE', #35041, 0.03000000000000002318 ) ;
#2870 = DIRECTION ( 'NONE',  ( 1.000000000000000000, 0.000000000000000000, 0.000000000000000000 ) ) ;
#2871 = CARTESIAN_POINT ( 'NONE',  ( 0.3666095998147628765, -1.617393197634767299, 0.4854686549615687685 ) ) ;
#2872 = ORIENTED_EDGE ( 'NONE', *, *, #18200, .T. ) ;
#2873 = AXIS2_PLACEMENT_3D ( 'NONE', #11161, #4378, #16738 ) ;
#2874 = VERTEX_POINT ( 'NONE', #9159 ) ;
#2875 = AXIS2_PLACEMENT_3D ( 'NONE', #36764, #15380, #27528 ) ;
#2876 = CARTESIAN_POINT ( 'NONE',  ( 0.4102339696967467475, -1.075663819259173870, 0.5182417262812423209 ) ) ;
#2877 = ORIENTED_EDGE ( 'NONE', *, *, #21233, .T. ) ;
#2878 = DIRECTION ( 'NONE',  ( -1.000000000000000000, -0.000000000000000000, -0.000000000000000000 ) ) ;
#2879 = CARTESIAN_POINT ( 'NONE',  ( 0.3999999999999787059, -2.183180860297921466, -0.4937760292030871079 ) ) ;
#2880 = CARTESIAN_POINT ( 'NONE',  ( 0.5884947987833728522, -1.442678314496853131, 0.6829111437943111707 ) ) ;
#2882 = ORIENTED_EDGE ( 'NONE', *, *, #14497, .T. ) ;
#2881 = CARTESIAN_POINT ( 'NONE',  ( 0.01000299637147959199, -0.5446455199555007010, 0.07760565969044912193 ) ) ;
#2883 = AXIS2_PLACEMENT_3D ( 'NONE', #27376, #39901, #24281 ) ;
#2884 = ORIENTED_EDGE ( 'NONE', *, *, #2720, .F. ) ;
#2885 = DIRECTION ( 'NONE',  ( -0.05576617209162638977, -0.2535907321156579686, 0.9657027879401052228 ) ) ;
#2886 = EDGE_CURVE ( 'NONE', #40221, #36916, #16735, .T. ) ;
#2887 = ORIENTED_EDGE ( 'NONE', *, *, #35863, .F. ) ;
#2888 = CIRCLE ( 'NONE', #9457, 0.01499999999999999251 ) ;
#2889 = CARTESIAN_POINT ( 'NONE',  ( 0.1635760886199158770, -1.208793886606414070, 0.9133870697123913640 ) ) ;
#2891 = CARTESIAN_POINT ( 'NONE',  ( 0.2277821696528544160, -1.351061424029422309, 0.4182417262808770797 ) ) ;
#2890 = CARTESIAN_POINT ( 'NONE',  ( 0.09659820559305749843, -0.8547292609823787801, 0.4202044640824337818 ) ) ;
#2892 = CARTESIAN_POINT ( 'NONE',  ( 0.1999999999999789724, -2.097675824466503247, -0.7286991843995637153 ) ) ;
#2893 = ADVANCED_FACE ( 'NONE', ( #37349 ), #14945, .F. ) ;
#2894 = EDGE_CURVE ( 'NONE', #19872, #37556, #29243, .T. ) ;
#2895 = CARTESIAN_POINT ( 'NONE',  ( 0.1499999999999996336, 0.09319974324249648279, 0.5318964258758775987 ) ) ;
#2897 = VERTEX_POINT ( 'NONE', #8359 ) ;
#2896 = ORIENTED_EDGE ( 'NONE', *, *, #15767, .T. ) ;
#2898 = EDGE_CURVE ( 'NONE', #10878, #39409, #26584, .T. ) ;
#2899 = CARTESIAN_POINT ( 'NONE',  ( 0.4675740435013452934, -1.069464823588083036, -0.4221806871052409815 ) ) ;
#2900 = CARTESIAN_POINT ( 'NONE',  ( 0.1852697703518006722, -0.8388889655799379730, 0.1397141703224135112 ) ) ;
#2901 = CARTESIAN_POINT ( 'NONE',  ( -0.05489899477340421524, -0.4472784955204494595, 0.1186631084353751558 ) ) ;
#2902 = CARTESIAN_POINT ( 'NONE',  ( 0.2730111487096660294, -0.9521603032302338177, 0.7332358461412977757 ) ) ;
#2903 = CARTESIAN_POINT ( 'NONE',  ( 0.2398899415561628889, -0.9495379235619473279, 0.6725648971787069330 ) ) ;
#2904 = CARTESIAN_POINT ( 'NONE',  ( 0.5389700097005715174, -1.668120067778418258, -0.4887748460763289837 ) ) ;
#2905 = AXIS2_PLACEMENT_3D ( 'NONE', #14308, #13887, #20294 ) ;
#2906 = CARTESIAN_POINT ( 'NONE',  ( 0.01258354067333375750, -0.4467589052256379922, 0.2540486221606858552 ) ) ;
#2907 = CIRCLE ( 'NONE', #21296, 2.001671648589477215 ) ;
#2908 = CARTESIAN_POINT ( 'NONE',  ( 0.3854584602151780448, -1.723663440349962439, 0.4240230717917121694 ) ) ;
#2909 = CARTESIAN_POINT ( 'NONE',  ( 0.6601361389616772213, -1.566348459635070522, 0.5707417262808793801 ) ) ;
#2910 = VECTOR ( 'NONE', #6313, 39.37007874015748854 ) ;
#2911 = ADVANCED_FACE ( 'NONE', ( #30974 ), #8826, .T. ) ;
#2912 = CARTESIAN_POINT ( 'NONE',  ( 0.05999999999999990757, -0.03575622569115821658, -0.2978615321325044363 ) ) ;
#2913 = CARTESIAN_POINT ( 'NONE',  ( 0.3197531882721045271, -1.462760974199709185, -0.5166151207181035598 ) ) ;
#2914 = DIRECTION ( 'NONE',  ( 1.000000000000000000, 1.243043370174342012E-14, 7.886895865933756492E-16 ) ) ;
#2915 = CARTESIAN_POINT ( 'NONE',  ( 0.003300039066125767893, -0.4845961630426517952, 0.3648084845760091732 ) ) ;
#2916 = CIRCLE ( 'NONE', #4193, 0.2149999999999999967 ) ;
#2917 = CARTESIAN_POINT ( 'NONE',  ( 0.09023307471144903502, -1.313753669190550255, 0.7175206707109292870 ) ) ;
#2918 = DATE_AND_TIME ( #28022, #33211 ) ;
#2919 = CARTESIAN_POINT ( 'NONE',  ( 0.6207796129641102167, -1.305782781463471265, 0.8357864796646383709 ) ) ;
#2920 = AXIS2_PLACEMENT_3D ( 'NONE', #16021, #22613, #12513 ) ;
#2921 = CARTESIAN_POINT ( 'NONE',  ( -0.07216878364870325802, 0.05141091571461162829, -0.1249999999999999029 ) ) ;
#2922 = CARTESIAN_POINT ( 'NONE',  ( 0.2134937173224229212, -1.278678410919930730, -0.5155029497116575543 ) ) ;
#2923 = CYLINDRICAL_SURFACE ( 'NONE', #10746, 0.1762268159172277748 ) ;
#2924 = CARTESIAN_POINT ( 'NONE',  ( -0.2746410161513782033, -2.289343986263487896, -0.7686455968847020204 ) ) ;
#2925 = ORIENTED_EDGE ( 'NONE', *, *, #31326, .F. ) ;
#2926 = FACE_OUTER_BOUND ( 'NONE', #23944, .T. ) ;
#2927 = CARTESIAN_POINT ( 'NONE',  ( 0.2326053079067355867, -1.504550822924993536, 0.9203436614353645018 ) ) ;
#2928 = AXIS2_PLACEMENT_3D ( 'NONE', #16307, #22091, #34611 ) ;
#2929 = CARTESIAN_POINT ( 'NONE',  ( 0.1568487634955791910, -0.6765984673290891260, 0.4608420472205499996 ) ) ;
#2931 = ORIENTED_EDGE ( 'NONE', *, *, #3385, .F. ) ;
#2930 = LINE ( 'NONE', #18776, #12567 ) ;
#2932 = CARTESIAN_POINT ( 'NONE',  ( 0.3304381985390301701, -0.8896417797241282788, 0.6549085351719812209 ) ) ;
#2934 = ORIENTED_EDGE ( 'NONE', *, *, #31085, .F. ) ;
#2933 = ORIENTED_EDGE ( 'NONE', *, *, #10901, .F. ) ;
#2935 = CARTESIAN_POINT ( 'NONE',  ( 0.6993744165018669356, -1.438184434374068399, 0.5964060907162921366 ) ) ;
#2936 = CIRCLE ( 'NONE', #39723, 0.01500000000000001159 ) ;
#2937 = EDGE_CURVE ( 'NONE', #24566, #36154, #4243, .T. ) ;
#2938 = CIRCLE ( 'NONE', #8180, 0.01499999999999994914 ) ;
#2939 = CARTESIAN_POINT ( 'NONE',  ( 0.3530204145741916433, -1.722873630718287252, -0.5364141961698728478 ) ) ;
#2940 = SECURITY_CLASSIFICATION ( '', '', #29010 ) ;
#2941 = CARTESIAN_POINT ( 'NONE',  ( 0.01548846960707511190, -0.2306506793134033284, 0.4716198300880330985 ) ) ;
#2942 = APPROVAL_DATE_TIME ( #9715, #29739 ) ;
#2943 = ADVANCED_FACE ( 'NONE', ( #24217 ), #6070, .T. ) ;
#2944 = DIRECTION ( 'NONE',  ( 1.000000000000000000, 0.000000000000000000, 0.000000000000000000 ) ) ;
#2945 = ORIENTED_EDGE ( 'NONE', *, *, #11667, .F. ) ;
#2946 = EDGE_CURVE ( 'NONE', #17948, #9996, #8549, .T. ) ;
#2947 = CARTESIAN_POINT ( 'NONE',  ( 0.08630297934288916339, -0.7465732544923662228, 0.1807232860058308743 ) ) ;
#2948 = CIRCLE ( 'NONE', #25961, 0.4614999999999880864 ) ;
#2949 = CARTESIAN_POINT ( 'NONE',  ( 0.5152864262115902649, -1.503242855671597766, 0.7141587765705896818 ) ) ;
#2951 = CARTESIAN_POINT ( 'NONE',  ( -0.002143816844750521915, -0.8544176354026742359, 0.1237328532832608491 ) ) ;
#2950 = FACE_OUTER_BOUND ( 'NONE', #8425, .T. ) ;
#2952 = CARTESIAN_POINT ( 'NONE',  ( -0.1696269498702784040, 0.4941072959623545868, 0.1354043093116672480 ) ) ;
#2953 = EDGE_CURVE ( 'NONE', #10668, #11891, #27307, .T. ) ;
#2954 = ORIENTED_EDGE ( 'NONE', *, *, #3469, .T. ) ;
#2955 = CARTESIAN_POINT ( 'NONE',  ( 0.4518928892634598293, -1.683692191370343538, 0.6017796442898305509 ) ) ;
#2956 = CARTESIAN_POINT ( 'NONE',  ( 0.6977729861270942635, -1.432737804912566082, 0.6428259928577456650 ) ) ;
#2957 = CARTESIAN_POINT ( 'NONE',  ( 0.7384722612031221489, -1.541404505398278779, -0.5155029497116575543 ) ) ;
#2958 = EDGE_CURVE ( 'NONE', #5177, #5941, #35115, .T. ) ;
#2959 = CARTESIAN_POINT ( 'NONE',  ( -0.1533385355407300699, 0.4750492940987078305, 0.3599999999999999867 ) ) ;
#2960 = EDGE_CURVE ( 'NONE', #4299, #18164, #20026, .T. ) ;
#2961 = DIRECTION ( 'NONE',  ( 0.000000000000000000, 0.000000000000000000, 1.000000000000000000 ) ) ;
#2962 = EDGE_CURVE ( 'NONE', #24540, #26513, #17934, .T. ) ;
#2963 = CARTESIAN_POINT ( 'NONE',  ( 0.3730815298380146805, -1.156738423958018291, 0.4182417262809047243 ) ) ;
#2964 = ADVANCED_FACE ( 'NONE', ( #21942 ), #16343, .T. ) ;
#2965 = AXIS2_PLACEMENT_3D ( 'NONE', #5816, #5015, #40390 ) ;
#2966 = CARTESIAN_POINT ( 'NONE',  ( 0.2675581168115488961, -1.674785173045962194, 0.4888193750310237395 ) ) ;
#2967 = DIRECTION ( 'NONE',  ( -0.007183093100618591353, -0.4999484090412826265, -0.8660253988599863062 ) ) ;
#2968 = CARTESIAN_POINT ( 'NONE',  ( 0.4609105641225965111, -1.064890115380353386, 0.6919706562625183022 ) ) ;
#2969 = AXIS2_PLACEMENT_3D ( 'NONE', #10212, #6695, #19272 ) ;
#2970 = PERSON_AND_ORGANIZATION ( #28500, #32463 ) ;
#2971 = DIRECTION ( 'NONE',  ( 0.4999551463232373427, -0.8660512985181134660, 0.000000000000000000 ) ) ;
#2972 = APPROVAL_PERSON_ORGANIZATION ( #26809, #22974, #29676 ) ;
#2973 = CARTESIAN_POINT ( 'NONE',  ( 0.5139471409257055923, -1.531975829649279808, 0.5486243274997595343 ) ) ;
#2974 = CIRCLE ( 'NONE', #31234, 0.5302738246768097241 ) ;
#2975 = CARTESIAN_POINT ( 'NONE',  ( -0.05615703521554896854, -0.01030498872321393249, 0.4592891699083805346 ) ) ;
#2976 = EDGE_LOOP ( 'NONE', ( #39123, #29194, #36082, #518 ) ) ;
#2977 = DIRECTION ( 'NONE',  ( 0.000000000000000000, 0.000000000000000000, -1.000000000000000000 ) ) ;
#2978 = CARTESIAN_POINT ( 'NONE',  ( -2.112273405726188513E-14, -2.183180860297921466, -0.4937760292030871079 ) ) ;
#2979 = SPHERICAL_SURFACE ( 'NONE', #23946, 0.01499999999999999944 ) ;
#2980 = ORIENTED_EDGE ( 'NONE', *, *, #12448, .F. ) ;
#2981 = CARTESIAN_POINT ( 'NONE',  ( -0.04308449196698978939, 0.05688586270224989944, -0.4910287377915250606 ) ) ;
#2982 = CARTESIAN_POINT ( 'NONE',  ( 0.1325631505235937146, -1.280238184107190369, 0.7308764952167086104 ) ) ;
#2984 = ORIENTED_EDGE ( 'NONE', *, *, #11756, .T. ) ;
#2983 = VERTEX_POINT ( 'NONE', #35469 ) ;
#2985 = CARTESIAN_POINT ( 'NONE',  ( -0.2746410161513779258, -2.183180860297908144, -0.4937760292030871079 ) ) ;
#2986 = ORIENTED_EDGE ( 'NONE', *, *, #10133, .T. ) ;
#2987 = CARTESIAN_POINT ( 'NONE',  ( 0.1253884927449593900, -1.293580113097495765, 0.4291439200971798318 ) ) ;
#2988 = CARTESIAN_POINT ( 'NONE',  ( 0.1992056882179587540, -2.039857513870245054, -0.3085428006972014692 ) ) ;
#2989 = AXIS2_PLACEMENT_3D ( 'NONE', #28280, #31567, #12258 ) ;
#2990 = DIRECTION ( 'NONE',  ( 0.000000000000000000, 7.931692224083225994E-17, -1.000000000000000000 ) ) ;
#2991 = EDGE_CURVE ( 'NONE', #23093, #40221, #7526, .T. ) ;
#2993 = CARTESIAN_POINT ( 'NONE',  ( 0.2211959769661343000, -1.309495541150525799, -0.5931747813493346566 ) ) ;
#2992 = CARTESIAN_POINT ( 'NONE',  ( 0.03174036153404483779, 0.5170813853140181493, 0.08825077997795766072 ) ) ;
#2994 = DIRECTION ( 'NONE',  ( 0.8660512985181129109, 0.4999551463232380089, 0.000000000000000000 ) ) ;
#2995 = ORIENTED_EDGE ( 'NONE', *, *, #14478, .T. ) ;
#2996 = CONICAL_SURFACE ( 'NONE', #17434, 0.07499999999999991396, 0.6931599075767558293 ) ;
#2997 = EDGE_CURVE ( 'NONE', #19917, #21274, #39374, .T. ) ;
#2998 = CARTESIAN_POINT ( 'NONE',  ( 0.07502636376510861405, -1.323892984169241949, 0.5081013553160158569 ) ) ;
#2999 = ORIENTED_EDGE ( 'NONE', *, *, #7874, .T. ) ;
#3000 = CYLINDRICAL_SURFACE ( 'NONE', #16128, 0.01750000000000000513 ) ;
#3001 = CARTESIAN_POINT ( 'NONE',  ( 0.4412115301948774104, -1.573601263554865293, 0.5662306361009304956 ) ) ;
#3003 = CARTESIAN_POINT ( 'NONE',  ( 0.5779288858437423571, -1.623150939738223109, 0.5629342317618580838 ) ) ;
#3002 = DIRECTION ( 'NONE',  ( -0.08131595302302933870, -0.04568309556551754247, 0.9956408843370728734 ) ) ;
#3004 = CARTESIAN_POINT ( 'NONE',  ( 0.2923286432308245808, -1.660243258845594649, -0.3694143330441917450 ) ) ;
#3005 = CARTESIAN_POINT ( 'NONE',  ( 0.1321224643482970806, -1.307861179043269040, -0.3150116852443416438 ) ) ;
#3006 = SECURITY_CLASSIFICATION ( '', '', #5898 ) ;
#3007 = UNCERTAINTY_MEASURE_WITH_UNIT (LENGTH_MEASURE( 1.000000000000000082E-05 ), #7004, 'distance_accuracy_value', 'NONE');
#3008 = LINE ( 'NONE', #6066, #16049 ) ;
#3009 = CARTESIAN_POINT ( 'NONE',  ( 0.1817222246005483210, -1.860686054201275086, -0.3146317322992087662 ) ) ;
#3010 = CARTESIAN_POINT ( 'NONE',  ( 0.1253102310817552911, -0.5531591968941835802, 0.1790963605822581683 ) ) ;
#3011 = CIRCLE ( 'NONE', #27971, 0.1346589359789736318 ) ;
#3012 = CARTESIAN_POINT ( 'NONE',  ( 0.4788046145333532677, -1.665542548548383905, 0.5304359953099284652 ) ) ;
#3013 = CARTESIAN_POINT ( 'NONE',  ( 0.05999999999999990757, 0.7171888913565960255, -0.2950238883388468514 ) ) ;
#3014 = B_SPLINE_CURVE_WITH_KNOTS ( 'NONE', 3,
 ( #27698, #14947, #40230, #18236 ),
 .UNSPECIFIED., .F., .F.,
 ( 4, 4 ),
 ( 0.02321896957645076462, 0.02481944680398503328 ),
 .UNSPECIFIED. ) ;
#3015 =( BOUNDED_SURFACE ( )  B_SPLINE_SURFACE ( 3, 2, ( 
 ( #7936, #36331, #20511 ),
 ( #33045, #20725, #33253 ),
 ( #30171, #39621, #1999 ),
 ( #14521, #5255, #8358 ) ),
 .UNSPECIFIED., .F., .F., .T. ) 
 B_SPLINE_SURFACE_WITH_KNOTS ( ( 4, 4 ),
 ( 3, 3 ),
 ( 0.001944782987540475327, 0.002901087691608646765 ),
 ( 0.000000000000000000, 1.000000000000000000 ),
 .UNSPECIFIED. ) 
 GEOMETRIC_REPRESENTATION_ITEM ( )  RATIONAL_B_SPLINE_SURFACE ( (
 ( 1.000000000000000000, 0.6942579658572588519, 1.000000000000000000),
 ( 1.000000000000000000, 0.6962136974480453988, 1.000000000000000000),
 ( 1.000000000000000000, 0.6983443629434031852, 1.000000000000000000),
 ( 1.000000000000000000, 0.6992614111707954327, 1.000000000000000000) ) ) 
 REPRESENTATION_ITEM ( '' )  SURFACE ( )  );
#3016 = CARTESIAN_POINT ( 'NONE',  ( 0.4753071910876713324, -1.208389221472485398, 0.5182417262812494263 ) ) ;
#3017 = CARTESIAN_POINT ( 'NONE',  ( 0.2217501959041398851, -1.238826317744727623, 0.5698378396483744224 ) ) ;
#3018 = DIRECTION ( 'NONE',  ( 0.4999999999999998890, 0.3297230132044474127, 0.8008013077932500945 ) ) ;
#3019 = CARTESIAN_POINT ( 'NONE',  ( 0.1826134026666640375, -1.261648033191452578, 0.4282186462236585722 ) ) ;
#3020 = EDGE_CURVE ( 'NONE', #36888, #37954, #26656, .T. ) ;
#3021 = CARTESIAN_POINT ( 'NONE',  ( 0.1896045607153576118, -0.5049209053381719103, 0.1595777137938904078 ) ) ;
#3022 = CARTESIAN_POINT ( 'NONE',  ( -0.05634490452573013425, 0.2738187358596016474, 0.3682637492038642879 ) ) ;
#3023 = CARTESIAN_POINT ( 'NONE',  ( 0.05281413292478839838, -1.208094164924696123, 0.6641569417577480872 ) ) ;
#3024 = AXIS2_PLACEMENT_3D ( 'NONE', #15931, #14007, #12632 ) ;
#3025 = CARTESIAN_POINT ( 'NONE',  ( 0.6331866186374228711, -1.597140103118768195, -0.4450843881964172688 ) ) ;
#3026 = CIRCLE ( 'NONE', #8915, 0.1000000000000000194 ) ;
#3027 = DIRECTION ( 'NONE',  ( 0.4999551463232372317, -0.8660512985181133550, 0.000000000000000000 ) ) ;
#3028 = CARTESIAN_POINT ( 'NONE',  ( 0.1654684907951354811, -0.8644978747596554491, 0.5573653326411247555 ) ) ;
#3029 = CARTESIAN_POINT ( 'NONE',  ( 0.1205378779716006349, 0.06113703066755019067, 0.04122227111665002081 ) ) ;
#3030 = DIRECTION ( 'NONE',  ( 0.4999551463232377313, -0.8660512985181132439, -0.000000000000000000 ) ) ;
#3031 = LOCAL_TIME ( 0, 53, 7.000000000000000000, #28627 ) ;
#3032 = ORIENTED_EDGE ( 'NONE', *, *, #37288, .T. ) ;
#3033 = CARTESIAN_POINT ( 'NONE',  ( -0.2399999999999999079, -4.015775813216793999, -0.6509878610687880318 ) ) ;
#3034 = CARTESIAN_POINT ( 'NONE',  ( -0.01548846960721245516, -0.07651041855108924039, -0.5222379212565266826 ) ) ;
#3035 = DIRECTION ( 'NONE',  ( -7.771561172376107616E-16, 7.170354002788761615E-17, -1.000000000000000000 ) ) ;
#3036 = CARTESIAN_POINT ( 'NONE',  ( 0.5249748772169798849, -1.642917355740116214, -0.4600979152061163702 ) ) ;
#3037 = LINE ( 'NONE', #400, #20652 ) ;
#3038 = CIRCLE ( 'NONE', #2361, 0.1400000000000007627 ) ;
#3039 = EDGE_LOOP ( 'NONE', ( #23609, #10377, #8626, #39961, #9208, #10298, #2163, #3851 ) ) ;
#3040 = DIRECTION ( 'NONE',  ( -1.000000000000000000, 0.000000000000000000, 0.000000000000000000 ) ) ;
#3041 = CARTESIAN_POINT ( 'NONE',  ( 0.6540709664215760277, -1.593060928864740156, 0.5182417262812423209 ) ) ;
#3042 = CARTESIAN_POINT ( 'NONE',  ( 0.06936654275873489761, -1.327133429011184917, 0.5458395137742713121 ) ) ;
#3043 = CARTESIAN_POINT ( 'NONE',  ( 0.05999999999999990757, 0.6655791756086271160, -0.3865134954953681201 ) ) ;
#3044 = CARTESIAN_POINT ( 'NONE',  ( 0.4746656776394587163, -1.252825698842344959, 0.6966861032914614116 ) ) ;
#3045 = EDGE_CURVE ( 'NONE', #14658, #25089, #29893, .T. ) ;
#3047 = VERTEX_POINT ( 'NONE', #4799 ) ;
#3046 = DIRECTION ( 'NONE',  ( -0.8660254037844408170, -0.3758398823372094966, 0.3297641321380312407 ) ) ;
#3048 = CARTESIAN_POINT ( 'NONE',  ( 0.3394669778924194747, -0.9758008820872865474, 0.6115353432225060226 ) ) ;
#3049 = ORIENTED_EDGE ( 'NONE', *, *, #37564, .T. ) ;
#3050 = PERSON_AND_ORGANIZATION_ROLE ( 'classification_officer' ) ;
#3051 = DIRECTION ( 'NONE',  ( -7.000205099780314469E-17, -1.000000000000000000, 6.590151126658399604E-16 ) ) ;
#3052 = ORIENTED_EDGE ( 'NONE', *, *, #22552, .T. ) ;
#3053 = ORIENTED_EDGE ( 'NONE', *, *, #21065, .F. ) ;
#3054 = CARTESIAN_POINT ( 'NONE',  ( 0.3868601653778248051, -1.605681501165217906, 0.5994997544633362541 ) ) ;
#3056 = CARTESIAN_POINT ( 'NONE',  ( 0.1847888282947060534, -0.8330427479178647010, 0.06499907415858525994 ) ) ;
#3055 = DIRECTION ( 'NONE',  ( -0.4999999999999998890, 0.6123724356957955806, -0.6123724356957935822 ) ) ;
#3057 = CARTESIAN_POINT ( 'NONE',  ( -0.05464101615137773038, -1.599201040860868339, 0.1642182323853691728 ) ) ;
#3058 = EDGE_LOOP ( 'NONE', ( #16851, #25467, #39490, #5246 ) ) ;
#3059 = ORIENTED_EDGE ( 'NONE', *, *, #24977, .T. ) ;
#3060 = ORIENTED_EDGE ( 'NONE', *, *, #30864, .F. ) ;
#3061 = AXIS2_PLACEMENT_3D ( 'NONE', #39665, #5291, #18467 ) ;
#3062 = CARTESIAN_POINT ( 'NONE',  ( 0.3558122948646044725, -0.9979958203889786050, 0.6057407852365402912 ) ) ;
#3063 = CARTESIAN_POINT ( 'NONE',  ( 0.1173840559349740853, -0.5715400563125977440, 0.2482123610220977605 ) ) ;
#3064 = EDGE_LOOP ( 'NONE', ( #6546, #9568 ) ) ;
#3065 = CARTESIAN_POINT ( 'NONE',  ( 0.1360281309732884192, -1.916305331242646570, -0.3368804578019788387 ) ) ;
#3066 = CARTESIAN_POINT ( 'NONE',  ( 0.07014435923142441076, -1.325199841737237261, 0.5075297796642793680 ) ) ;
#3067 = LOCAL_TIME ( 0, 53, 7.000000000000000000, #15889 ) ;
#3068 = DIRECTION ( 'NONE',  ( 0.8660512985181134660, 0.4999551463232372317, 0.000000000000000000 ) ) ;
#3069 = CARTESIAN_POINT ( 'NONE',  ( 0.3666666666666451579, -1.960071684622068489, -0.3089366850217884486 ) ) ;
#3070 = AXIS2_PLACEMENT_3D ( 'NONE', #21685, #21079, #2560 ) ;
#3071 = LINE ( 'NONE', #6340, #38373 ) ;
#3072 = CARTESIAN_POINT ( 'NONE',  ( 0.03654364704248811574, 0.3642884434512987379, -0.3592365245254292572 ) ) ;
#3073 = DIRECTION ( 'NONE',  ( 0.000000000000000000, 0.000000000000000000, -1.000000000000000000 ) ) ;
#3074 = DIRECTION ( 'NONE',  ( 0.000000000000000000, 0.000000000000000000, -1.000000000000000000 ) ) ;
#3075 = APPLICATION_PROTOCOL_DEFINITION ( 'international standard', 'automotive_design', 2000, #36864 ) ;
#3076 = CARTESIAN_POINT ( 'NONE',  ( 0.3767165169986340101, -1.018944133209149783, 0.6225985890371608100 ) ) ;
#3077 = DIRECTION ( 'NONE',  ( -0.3468893892380660593, -0.2594111197898882892, -0.9013177145509778665 ) ) ;
#3078 = CARTESIAN_POINT ( 'NONE',  ( 0.4638218765581886838, -1.238038477568070839, 0.6057417262809816627 ) ) ;
#3079 = CARTESIAN_POINT ( 'NONE',  ( 0.3130702568482664483, -1.175243511012216580, 0.5339619868235715439 ) ) ;
#3080 = CARTESIAN_POINT ( 'NONE',  ( 0.03359830163007831300, -1.106472467758128353, 0.6807021762515294006 ) ) ;
#3081 = DIRECTION ( 'NONE',  ( 1.000000000000000000, -0.000000000000000000, -0.000000000000000000 ) ) ;
#3082 = CARTESIAN_POINT ( 'NONE',  ( 0.1898786726785968715, -1.668530212669821600, -0.6859658009302209702 ) ) ;
#3083 = AXIS2_PLACEMENT_3D ( 'NONE', #2922, #25134, #15475 ) ;
#3084 = CARTESIAN_POINT ( 'NONE',  ( 0.3186359832558304794, -1.645093617292038957, 0.5084158906598844618 ) ) ;
#3085 = EDGE_LOOP ( 'NONE', ( #27978, #22045, #5285, #3311 ) ) ;
#3086 = EDGE_LOOP ( 'NONE', ( #7463, #3834, #34389, #25369 ) ) ;
#3087 = FACE_OUTER_BOUND ( 'NONE', #18565, .T. ) ;
#3088 = EDGE_LOOP ( 'NONE', ( #20961, #19214, #19599, #24152 ) ) ;
#3089 = SECURITY_CLASSIFICATION ( '', '', #16493 ) ;
#3090 = CARTESIAN_POINT ( 'NONE',  ( -0.01895494625228218155, 0.07381100255646892705, 0.5147985126481148255 ) ) ;
#3091 = CARTESIAN_POINT ( 'NONE',  ( 0.02869712619511915336, 0.2420104654861724158, 0.4357576342647241363 ) ) ;
#3092 = LINE ( 'NONE', #24902, #7275 ) ;
#3094 = ORIENTED_EDGE ( 'NONE', *, *, #35938, .T. ) ;
#3093 = CYLINDRICAL_SURFACE ( 'NONE', #35086, 0.5400000000000001465 ) ;
#3095 = ORIENTED_EDGE ( 'NONE', *, *, #25279, .T. ) ;
#3096 = CARTESIAN_POINT ( 'NONE',  ( -0.1450923023275085544, -0.5230583524814751417, 0.1380392329925464179 ) ) ;
#3097 = CARTESIAN_POINT ( 'NONE',  ( 0.3014137048403158770, -1.651046165962986478, 0.6735612096716837582 ) ) ;
#3099 = DIRECTION ( 'NONE',  ( -0.4999551463232372317, 0.8660512985181135770, -0.000000000000000000 ) ) ;
#3098 = FACE_OUTER_BOUND ( 'NONE', #36640, .T. ) ;
#3100 = CARTESIAN_POINT ( 'NONE',  ( 0.05999999999999990757, 0.6730055122658872291, -0.1180550278835343775 ) ) ;
#3101 = DIRECTION ( 'NONE',  ( -1.387778780781449423E-15, 6.590151126658376924E-16, -1.000000000000000000 ) ) ;
#3103 = ORIENTED_EDGE ( 'NONE', *, *, #16045, .F. ) ;
#3102 = ORIENTED_EDGE ( 'NONE', *, *, #36554, .T. ) ;
#3104 = DIRECTION ( 'NONE',  ( 0.000000000000000000, 0.000000000000000000, -1.000000000000000000 ) ) ;
#3105 = CYLINDRICAL_SURFACE ( 'NONE', #10937, 0.04330708661417322775 ) ;
#3106 = CARTESIAN_POINT ( 'NONE',  ( -0.02238765564324999430, -0.5044129532808624417, 0.09031612285223891701 ) ) ;
#3107 = CARTESIAN_POINT ( 'NONE',  ( 0.5473844695833234297, -1.374494293802986711, 0.7608074972636496014 ) ) ;
#3108 = CARTESIAN_POINT ( 'NONE',  ( 0.2821105676325378897, -1.010667300530192936, 0.7205108277189851140 ) ) ;
#3109 = CARTESIAN_POINT ( 'NONE',  ( -0.2299999999999999267, 0.5182417262804744906, 0.3599999999999993205 ) ) ;
#3110 = CARTESIAN_POINT ( 'NONE',  ( 0.3254365784322334476, -1.747317980671322157, 0.7218611321553708438 ) ) ;
#3111 = CARTESIAN_POINT ( 'NONE',  ( 0.07217859744021073998, -1.325427469710779738, 0.5682417262808779901 ) ) ;
#3112 = CARTESIAN_POINT ( 'NONE',  ( 0.3259879919982042185, -1.767950897709266611, 0.5312986935552648227 ) ) ;
#3113 = CARTESIAN_POINT ( 'NONE',  ( 0.4040419229627993936, -1.153899704180549879, 0.7428076885917280769 ) ) ;
#3114 = DIRECTION ( 'NONE',  ( -0.4999551463232372317, 0.8660512985181134660, -0.000000000000000000 ) ) ;
#3115 = DIRECTION ( 'NONE',  ( -0.5067625458874882582, -0.2925444984769761114, -0.8109312168713729285 ) ) ;
#3116 = CARTESIAN_POINT ( 'NONE',  ( 0.05279755784604373697, -0.2420637527537941869, 0.4010259520538019262 ) ) ;
#3117 = EDGE_CURVE ( 'NONE', #27710, #20709, #1167, .T. ) ;
#3118 = LINE ( 'NONE', #22458, #2789 ) ;
#3119 = CARTESIAN_POINT ( 'NONE',  ( 0.08371583302770695123, -1.272799487215662495, 0.7379929360799946103 ) ) ;
#3120 = EDGE_CURVE ( 'NONE', #7245, #8808, #1035, .T. ) ;
#3121 = PERSON_AND_ORGANIZATION ( #28500, #32463 ) ;
#3122 = CARTESIAN_POINT ( 'NONE',  ( 0.2575330336140166931, -0.6922558787343077169, 0.5832620184353838333 ) ) ;
#3123 = EDGE_CURVE ( 'NONE', #5600, #23137, #20065, .T. ) ;
#3124 = CARTESIAN_POINT ( 'NONE',  ( -0.02881408050861471171, 0.4517606495562093705, 0.2100211630561648612 ) ) ;
#3125 = DIRECTION ( 'NONE',  ( -1.000000000000000000, -0.000000000000000000, -0.000000000000000000 ) ) ;
#3126 = EDGE_CURVE ( 'NONE', #33134, #25252, #39747, .T. ) ;
#3127 = FACE_OUTER_BOUND ( 'NONE', #3085, .T. ) ;
#3128 = B_SPLINE_CURVE_WITH_KNOTS ( 'NONE', 3,
 ( #26103, #28950, #9827, #34722, #13535, #22998, #1216, #10438, #22399, #22609, #38414, #35523, #3458, #29375, #26285, #25895, #13719, #38807 ),
 .UNSPECIFIED., .F., .F.,
 ( 4, 2, 2, 2, 2, 2, 2, 2, 4 ),
 ( 0.000000000000000000, 0.0006978799593375504704, 0.001395759918675100941, 0.002093639878012653905, 0.002791519837350207953, 0.003489399796687762435, 0.004187279756025318218, 0.004885159715362874001, 0.005583039674700429784 ),
 .UNSPECIFIED. ) ;
#3129 = DIRECTION ( 'NONE',  ( -9.244463733058732095E-32, 0.1402348365094961968, 0.9901182710308678026 ) ) ;
#3130 = ORIENTED_EDGE ( 'NONE', *, *, #7231, .F. ) ;
#3131 = DIRECTION ( 'NONE',  ( -1.000000000000000000, -0.000000000000000000, -0.000000000000000000 ) ) ;
#3132 = CARTESIAN_POINT ( 'NONE',  ( 0.2689337271815545605, -1.650725020051581504, 0.7800499242891761886 ) ) ;
#3133 = CARTESIAN_POINT ( 'NONE',  ( 0.5346679333427164504, -1.402191149477463261, 0.7798264699775933062 ) ) ;
#3135 = EDGE_LOOP ( 'NONE', ( #28077, #39870, #10460, #13950 ) ) ;
#3134 = DIRECTION ( 'NONE',  ( 1.000000000000000000, 0.000000000000000000, 0.000000000000000000 ) ) ;
#3136 = CARTESIAN_POINT ( 'NONE',  ( 0.5554409461590971153, -1.190971970253151824, 0.5682417262808781011 ) ) ;
#3138 = ORIENTED_EDGE ( 'NONE', *, *, #17502, .F. ) ;
#3137 = ORIENTED_EDGE ( 'NONE', *, *, #7908, .F. ) ;
#3139 = CARTESIAN_POINT ( 'NONE',  ( 0.6575415210681188061, -1.363599502042151190, 0.7651167678683458151 ) ) ;
#3140 = DIRECTION ( 'NONE',  ( 0.4999551463232372317, -0.8660512985181135770, 0.000000000000000000 ) ) ;
#3141 = EDGE_CURVE ( 'NONE', #14090, #7026, #14797, .T. ) ;
#3142 = APPLIED_PERSON_AND_ORGANIZATION_ASSIGNMENT ( #34020, #2756, ( #7563 ) ) ;
#3143 = CARTESIAN_POINT ( 'NONE',  ( 0.4517177305807006937, -1.568671020668126914, 0.6057417262804751790 ) ) ;
#3144 = COORDINATED_UNIVERSAL_TIME_OFFSET ( 0, 0, .AHEAD. ) ;
#3145 = CARTESIAN_POINT ( 'NONE',  ( 0.1999999999999789724, -2.183180860297921466, -0.4937760292030871079 ) ) ;
#3146 = EDGE_LOOP ( 'NONE', ( #38694, #6423, #4424, #19178 ) ) ;
#3147 = CARTESIAN_POINT ( 'NONE',  ( 0.09865219997896333692, -0.7828559995779595937, 0.3308637533635402361 ) ) ;
#3148 = CARTESIAN_POINT ( 'NONE',  ( 0.3186686258432176455, -1.760399750288523357, 0.5682417262808792113 ) ) ;
#3149 = CARTESIAN_POINT ( 'NONE',  ( 0.5262759607219161806, -1.526737561883647398, 0.5945435633807139020 ) ) ;
#3150 = CARTESIAN_POINT ( 'NONE',  ( 0.6430590169175627313, -1.417851464528291139, -0.6270229543717609211 ) ) ;
#3151 = VERTEX_POINT ( 'NONE', #35687 ) ;
#3152 = CARTESIAN_POINT ( 'NONE',  ( 0.1759300380180282841, -1.231083256582695906, -0.6184399470714002645 ) ) ;
#3153 = CARTESIAN_POINT ( 'NONE',  ( 0.6633289903567118895, -1.542975281133564636, 0.6975821153327242952 ) ) ;
#3154 = CARTESIAN_POINT ( 'NONE',  ( 0.5699439007204750718, -1.617412408666830448, 0.5656496617915443004 ) ) ;
#3155 = CARTESIAN_POINT ( 'NONE',  ( 0.4121964764379724144, -1.591045810388358905, -0.3442890830420804460 ) ) ;
#3156 = LENGTH_MEASURE_WITH_UNIT ( LENGTH_MEASURE( 0.02539999999999999897 ), #25581 );
#3157 = DIRECTION ( 'NONE',  ( -1.000000000000000000, -0.000000000000000000, -0.000000000000000000 ) ) ;
#3158 = CARTESIAN_POINT ( 'NONE',  ( 0.2676785629568417257, -1.674416124214124446, 0.5054568562724600644 ) ) ;
#3159 = CARTESIAN_POINT ( 'NONE',  ( 1.365923996832131609E-16, -0.9481888444201339583, 0.1457185332388703791 ) ) ;
#3160 = CARTESIAN_POINT ( 'NONE',  ( 0.1896483993057378192, -0.6911749089203499397, 0.2228938739458891649 ) ) ;
#3161 = EDGE_CURVE ( 'NONE', #3269, #8639, #34493, .T. ) ;
#3162 = PERSON_AND_ORGANIZATION ( #28500, #32463 ) ;
#3163 = CARTESIAN_POINT ( 'NONE',  ( 0.5709043678375559372, -1.616165998060699049, 0.5779678008732025418 ) ) ;
#3164 = EDGE_CURVE ( 'NONE', #14867, #30658, #12830, .T. ) ;
#3165 = VERTEX_POINT ( 'NONE', #10799 ) ;
#3166 = EDGE_CURVE ( 'NONE', #22246, #37335, #7888, .T. ) ;
#3167 = CARTESIAN_POINT ( 'NONE',  ( 0.5845226641748834107, -1.491917136578684744, 0.5353822420918034064 ) ) ;
#3168 = EDGE_CURVE ( 'NONE', #15800, #36123, #18051, .T. ) ;
#3169 = CARTESIAN_POINT ( 'NONE',  ( -0.05543910610525255162, -0.02035452233659878693, 0.4608669713610800134 ) ) ;
#3170 = EDGE_LOOP ( 'NONE', ( #38504, #646, #4565, #254 ) ) ;
#3171 = DIRECTION ( 'NONE',  ( 0.000000000000000000, 3.330669073875470114E-16, 1.000000000000000000 ) ) ;
#3172 = CYLINDRICAL_SURFACE ( 'NONE', #28912, 0.06249999999999997918 ) ;
#3173 = CARTESIAN_POINT ( 'NONE',  ( 0.08562216985915493961, -0.7978384895209408301, 0.09062995534711226764 ) ) ;
#3174 = VERTEX_POINT ( 'NONE', #18375 ) ;
#3175 = CARTESIAN_POINT ( 'NONE',  ( -0.03478556507500901035, -0.07228131100493927208, -0.5113607228826313467 ) ) ;
#3176 = CARTESIAN_POINT ( 'NONE',  ( -0.005479581593941192964, -0.8983412709979351485, 0.5156674170252182332 ) ) ;
#3178 = ORIENTED_EDGE ( 'NONE', *, *, #36470, .T. ) ;
#3177 = ORIENTED_EDGE ( 'NONE', *, *, #2504, .F. ) ;
#3179 = DIRECTION ( 'NONE',  ( 0.000000000000000000, 1.786920323354501031E-15, -1.000000000000000000 ) ) ;
#3180 = CARTESIAN_POINT ( 'NONE',  ( 0.3351195522891313172, -1.762354232558481337, 0.5631496603913015431 ) ) ;
#3181 = EDGE_CURVE ( 'NONE', #37440, #24067, #10836, .T. ) ;
#3182 = CARTESIAN_POINT ( 'NONE',  ( 0.1804425756904262101, -1.792597923215050182, -0.3531089307126511478 ) ) ;
#3184 = CARTESIAN_POINT ( 'NONE',  ( -0.08000000000000000167, -2.274798198814180772, -0.3601501197397404264 ) ) ;
#3183 = DIRECTION ( 'NONE',  ( -0.3468893892380648936, -0.9373665302208731287, 0.03180785525185938351 ) ) ;
#3185 = DIRECTION ( 'NONE',  ( 8.881784197001246407E-16, -2.361472542561082612E-16, 1.000000000000000000 ) ) ;
#3186 = ORIENTED_EDGE ( 'NONE', *, *, #37813, .F. ) ;
#3187 = CARTESIAN_POINT ( 'NONE',  ( 0.1124437242459924158, -0.6641345740908473072, 0.4088893035250216190 ) ) ;
#3188 = ORIENTED_EDGE ( 'NONE', *, *, #6625, .F. ) ;
#3189 = ORIENTED_EDGE ( 'NONE', *, *, #28075, .F. ) ;
#3190 = CARTESIAN_POINT ( 'NONE',  ( 0.6964952729471024506, -1.533352077435225391, 0.5923684272575838738 ) ) ;
#3191 = CARTESIAN_POINT ( 'NONE',  ( 0.07283724563382373840, -0.5406377204022615457, 0.1540664544690148741 ) ) ;
#3193 = CARTESIAN_POINT ( 'NONE',  ( 0.5574362741858098769, -1.620420278163815286, 0.4861798668042197069 ) ) ;
#3192 = CARTESIAN_POINT ( 'NONE',  ( 0.5194227709487030387, -1.611319201048296623, -0.4830683290006882458 ) ) ;
#3194 = DIRECTION ( 'NONE',  ( -0.4999551463232372317, 0.8660512985181134660, -0.000000000000000000 ) ) ;
#3195 = CARTESIAN_POINT ( 'NONE',  ( 0.2634247196158754356, -0.9771240080834830977, 0.5484523488112167389 ) ) ;
#3196 = CARTESIAN_POINT ( 'NONE',  ( 0.1186103394390872201, -1.414144848331978510, 0.5683298932114988489 ) ) ;
#3197 = CARTESIAN_POINT ( 'NONE',  ( 0.4008157502961269270, -1.730613119872131733, -0.3050311287808085692 ) ) ;
#3198 = CARTESIAN_POINT ( 'NONE',  ( 0.1259887422558554904, -0.5708039110117676396, 0.2411005981708249368 ) ) ;
#3199 = CARTESIAN_POINT ( 'NONE',  ( -0.05562144613422703721, 0.2870684680408743805, 0.3605846877396484684 ) ) ;
#3200 = DIRECTION ( 'NONE',  ( 0.000000000000000000, 0.000000000000000000, -1.000000000000000000 ) ) ;
#3201 = DIRECTION ( 'NONE',  ( 0.000000000000000000, 0.000000000000000000, -1.000000000000000000 ) ) ;
#3202 = CARTESIAN_POINT ( 'NONE',  ( 0.3340217598881563554, -1.134046545150164009, -0.5155029497116575543 ) ) ;
#3203 = DIRECTION ( 'NONE',  ( 0.8660512985181133550, 0.4999551463232372317, 0.000000000000000000 ) ) ;
#3204 = CARTESIAN_POINT ( 'NONE',  ( 0.6347819612394876021, -1.328236395719069263, 0.8269854195084552773 ) ) ;
#3205 = CARTESIAN_POINT ( 'NONE',  ( -0.02872242845530542654, 0.3729171224323668543, 0.3802687114177480399 ) ) ;
#3206 = CARTESIAN_POINT ( 'NONE',  ( 0.01932545507967057402, -1.072689427073633128, 0.6194964679467892532 ) ) ;
#3207 = EDGE_CURVE ( 'NONE', #29747, #30067, #12156, .T. ) ;
#3208 = CARTESIAN_POINT ( 'NONE',  ( 0.6264012344811226152, -1.546116565118341057, -0.4272351601427545331 ) ) ;
#3209 = CARTESIAN_POINT ( 'NONE',  ( 0.1961333673497456243, -0.6677565227190264130, 0.3323178443805968052 ) ) ;
#3210 = FACE_OUTER_BOUND ( 'NONE', #27052, .T. ) ;
#3211 = CARTESIAN_POINT ( 'NONE',  ( 0.07006815180908280982, -1.315301596572416631, 0.5080907171456734428 ) ) ;
#3212 = CARTESIAN_POINT ( 'NONE',  ( 0.6409058204046232943, -1.459016202299332710, -0.5155029497116575543 ) ) ;
#3213 = ORIENTED_EDGE ( 'NONE', *, *, #3465, .F. ) ;
#3214 = CARTESIAN_POINT ( 'NONE',  ( 0.3622253751127866850, -1.756884464425456205, -0.4902987826081466327 ) ) ;
#3215 = LINE ( 'NONE', #19066, #40346 ) ;
#3216 = CARTESIAN_POINT ( 'NONE',  ( 0.3660688374457184424, -2.015896937187397597, -0.4887634650597760255 ) ) ;
#3217 = CARTESIAN_POINT ( 'NONE',  ( 0.08509557923809639435, -0.8164785559594017750, 0.1457185332388710730 ) ) ;
#3218 = CARTESIAN_POINT ( 'NONE',  ( 0.3699999999999786793, -2.166079853131637645, -0.5407606602423824516 ) ) ;
#3219 = ORIENTED_EDGE ( 'NONE', *, *, #26053, .F. ) ;
#3220 = DIRECTION ( 'NONE',  ( 0.000000000000000000, 0.000000000000000000, -1.000000000000000000 ) ) ;
#3221 = CARTESIAN_POINT ( 'NONE',  ( 0.1871240791749231025, -1.373980404802405353, 0.5685824782455963788 ) ) ;
#3222 = DIRECTION ( 'NONE',  ( -0.4999551463232377313, 0.8660512985181132439, -0.000000000000000000 ) ) ;
#3223 = EDGE_CURVE ( 'NONE', #17694, #31075, #21360, .T. ) ;
#3224 = DIRECTION ( 'NONE',  ( -2.157041537713702240E-32, 0.8709776783778059306, -0.4913225862583635584 ) ) ;
#3225 = CARTESIAN_POINT ( 'NONE',  ( 0.3342347797450085922, -1.058365783522508208, 0.7408787376446750450 ) ) ;
#3227 = CARTESIAN_POINT ( 'NONE',  ( 0.5455881031540378290, -1.595019605959082654, -0.5473203437262895710 ) ) ;
#3226 = CARTESIAN_POINT ( 'NONE',  ( -0.2399999999999999079, -3.068736697824635318, 0.08412833800243585403 ) ) ;
#3228 = CARTESIAN_POINT ( 'NONE',  ( 0.4765072543226545609, -1.073695880004174930, 0.6154142099768207252 ) ) ;
#3229 = VERTEX_POINT ( 'NONE', #24777 ) ;
#3230 = EDGE_CURVE ( 'NONE', #9944, #12909, #371, .T. ) ;
#3231 = DATE_AND_TIME ( #12096, #27994 ) ;
#3232 = APPLICATION_CONTEXT ( 'configuration controlled 3d designs of mechanical parts and assemblies' ) ;
#3233 = CARTESIAN_POINT ( 'NONE',  ( 0.02691720668820642148, -0.9716517312894669134, 0.6480984491125419966 ) ) ;
#3234 = ORIENTED_EDGE ( 'NONE', *, *, #29852, .F. ) ;
#3235 = ORIENTED_EDGE ( 'NONE', *, *, #27838, .F. ) ;
#3236 =( BOUNDED_SURFACE ( )  B_SPLINE_SURFACE ( 3, 2, ( 
 ( #23140, #29086, #22939 ),
 ( #29914, #953, #26218 ),
 ( #7470, #11180, #13464 ),
 ( #20048, #26418, #4189 ),
 ( #29304, #32580, #10376 ),
 ( #1151, #17358, #36071 ),
 ( #1756, #1542, #14063 ),
 ( #32774, #4396, #29497 ),
 ( #26640, #26029, #14268 ),
 ( #7689, #35454, #13652 ),
 ( #10566, #38953, #13845 ),
 ( #1337, #7870, #10783 ),
 ( #23356, #35875, #20253 ),
 ( #17149, #39361, #29698 ),
 ( #39170, #10996, #26832 ),
 ( #23554, #20443, #4783 ),
 ( #15280, #24344, #39966 ),
 ( #33582, #39548, #11382 ),
 ( #8687, #23954, #18364 ),
 ( #30910, #8297, #27237 ),
 ( #36878, #8491, #30303 ),
 ( #1940, #27441, #18163 ) ),
 .UNSPECIFIED., .F., .F., .T. ) 
 B_SPLINE_SURFACE_WITH_KNOTS ( ( 4, 2, 2, 2, 2, 2, 2, 2, 2, 2, 4 ),
 ( 3, 3 ),
 ( 0.002013519961495850458, 0.002780892266055759107, 0.003548264570615667322, 0.004315636875175575538, 0.004699323027455529211, 0.005083009179735483753, 0.005466695332015438294, 0.005850381484295391968, 0.006617753788855301050, 0.007385126093415209265, 0.008152498397975117481 ),
 ( 0.000000000000000000, 1.000000000000000000 ),
 .UNSPECIFIED. ) 
 GEOMETRIC_REPRESENTATION_ITEM ( )  RATIONAL_B_SPLINE_SURFACE ( (
 ( 1.000000000000000000, 0.7283825911960394306, 1.000000000000000000),
 ( 1.000000000000000000, 0.7404375345927788343, 1.000000000000000000),
 ( 1.000000000000000000, 0.7521483142434980396, 1.000000000000000000),
 ( 1.000000000000000000, 0.7744460733777461803, 1.000000000000000000),
 ( 1.000000000000000000, 0.7845612039380909231, 1.000000000000000000),
 ( 1.000000000000000000, 0.8022035258263227053, 1.000000000000000000),
 ( 1.000000000000000000, 0.8093965293320134480, 1.000000000000000000),
 ( 1.000000000000000000, 0.8169028692726254537, 1.000000000000000000),
 ( 1.000000000000000000, 0.8188329634863041884, 1.000000000000000000),
 ( 1.000000000000000000, 0.8214004505364363995, 1.000000000000000000),
 ( 1.000000000000000000, 0.8220602406259868156, 1.000000000000000000),
 ( 1.000000000000000000, 0.8220736605436752553, 1.000000000000000000),
 ( 1.000000000000000000, 0.8214126668415123733, 1.000000000000000000),
 ( 1.000000000000000000, 0.8188520474558839135, 1.000000000000000000),
 ( 1.000000000000000000, 0.8169545908334268081, 1.000000000000000000),
 ( 1.000000000000000000, 0.8094771004219970534, 1.000000000000000000),
 ( 1.000000000000000000, 0.8022723753809176683, 1.000000000000000000),
 ( 1.000000000000000000, 0.7845733350635825110, 1.000000000000000000),
 ( 1.000000000000000000, 0.7744472902493447775, 1.000000000000000000),
 ( 1.000000000000000000, 0.7522916829163305286, 1.000000000000000000),
 ( 1.000000000000000000, 0.7403553004665949233, 1.000000000000000000),
 ( 1.000000000000000000, 0.7283825911960398747, 1.000000000000000000) ) ) 
 REPRESENTATION_ITEM ( '' )  SURFACE ( )  );
#3237 = CARTESIAN_POINT ( 'NONE',  ( 0.07236692127650729001, -0.7316196773536807196, 0.5741060721534142486 ) ) ;
#3239 = CARTESIAN_POINT ( 'NONE',  ( 0.1747797283729930762, -0.8954128581900229200, 0.04731367366808376940 ) ) ;
#3238 = CARTESIAN_POINT ( 'NONE',  ( 0.8248651029816849167, 0.000000000000000000, 0.000000000000000000 ) ) ;
#3240 = CARTESIAN_POINT ( 'NONE',  ( 0.06761598059943987882, -0.6219880238673772821, 0.01307546307162734019 ) ) ;
#3241 = ORIENTED_EDGE ( 'NONE', *, *, #13667, .T. ) ;
#3242 = VERTEX_POINT ( 'NONE', #37299 ) ;
#3243 = ORIENTED_EDGE ( 'NONE', *, *, #3123, .F. ) ;
#3244 = ORIENTED_EDGE ( 'NONE', *, *, #25035, .T. ) ;
#3245 = FACE_OUTER_BOUND ( 'NONE', #18679, .T. ) ;
#3246 = CARTESIAN_POINT ( 'NONE',  ( 0.5359002092464226763, -1.453873471191388544, 0.7520340848835496139 ) ) ;
#3247 = EDGE_LOOP ( 'NONE', ( #34094, #337, #32721, #15715, #14050 ) ) ;
#3248 = CARTESIAN_POINT ( 'NONE',  ( 0.1869154501082920528, -0.7268340247273499255, 0.03292103754823103717 ) ) ;
#3249 = CARTESIAN_POINT ( 'NONE',  ( 0.01548846960707309615, -0.09061086148586028344, 0.5171215251570917548 ) ) ;
#3250 = FACE_BOUND ( 'NONE', #26826, .T. ) ;
#3251 = CARTESIAN_POINT ( 'NONE',  ( 0.5616682974235900350, -1.585511599874633193, -0.5166151207188732775 ) ) ;
#3252 = CARTESIAN_POINT ( 'NONE',  ( -0.1133687188271738921, -0.5183431199920780497, 0.3403596628068928376 ) ) ;
#3253 = CARTESIAN_POINT ( 'NONE',  ( -0.08000000000000000167, -2.116970787486931460, -0.3045972195783253067 ) ) ;
#3254 = DIRECTION ( 'NONE',  ( 0.6185154643211973058, 0.3739688674182602979, -0.6910759050910669776 ) ) ;
#3255 = DIRECTION ( 'NONE',  ( -1.355854680848614478E-31, 3.330669073875470114E-16, 1.000000000000000000 ) ) ;
#3256 = CARTESIAN_POINT ( 'NONE',  ( 0.1319437676963613748, -1.258139845592547434, 0.6230237721763144387 ) ) ;
#3257 = CARTESIAN_POINT ( 'NONE',  ( 0.2414668910093290266, -2.060278424428106270, -0.6831623107723641120 ) ) ;
#3258 = DIRECTION ( 'NONE',  ( 0.000000000000000000, 0.3882559824134205195, -0.9215515678030119506 ) ) ;
#3259 = CALENDAR_DATE ( 2026, 13, 10 ) ;
#3260 = ADVANCED_FACE ( 'NONE', ( #36499 ), #14685, .T. ) ;
#3261 = CARTESIAN_POINT ( 'NONE',  ( 0.2734279889346977188, -0.9622732688880970553, 0.5233991146725487376 ) ) ;
#3262 = CARTESIAN_POINT ( 'NONE',  ( -0.01548846960707463312, 0.3772621329472714558, -0.3651003739303425033 ) ) ;
#3263 = DIRECTION ( 'NONE',  ( 0.4999551463232372317, -0.8660512985181134660, 0.000000000000000000 ) ) ;
#3264 = FACE_BOUND ( 'NONE', #22642, .T. ) ;
#3265 = CARTESIAN_POINT ( 'NONE',  ( 0.1721302213443809126, -1.453494483496651890, 0.7931418093652549128 ) ) ;
#3266 = CARTESIAN_POINT ( 'NONE',  ( -0.08000000000000000167, -2.183180860297908144, -0.4937760292030871079 ) ) ;
#3267 = CARTESIAN_POINT ( 'NONE',  ( 0.05999999999999990757, -0.3458405862425447119, -0.2552451372150014719 ) ) ;
#3268 = CARTESIAN_POINT ( 'NONE',  ( 0.3587090678007808231, -1.161727987938869555, 0.4182417262808778013 ) ) ;
#3269 = VERTEX_POINT ( 'NONE', #33405 ) ;
#3270 = ORIENTED_EDGE ( 'NONE', *, *, #3938, .T. ) ;
#3271 = CARTESIAN_POINT ( 'NONE',  ( 0.03309060444528755252, -0.3730661130945429060, -0.3633899800202398112 ) ) ;
#3272 = ORIENTED_EDGE ( 'NONE', *, *, #10704, .F. ) ;
#3273 = CARTESIAN_POINT ( 'NONE',  ( -0.2399999999999999079, -2.183180860297908144, -0.4937760292030871079 ) ) ;
#3274 = CARTESIAN_POINT ( 'NONE',  ( 0.04230188431063456461, 0.2825024449121547598, 0.3739792551055085013 ) ) ;
#3275 = CARTESIAN_POINT ( 'NONE',  ( 0.5983201278204041129, -1.462679505942070080, 0.6053214617447383317 ) ) ;
#3277 = ORIENTED_EDGE ( 'NONE', *, *, #12815, .T. ) ;
#3276 = CARTESIAN_POINT ( 'NONE',  ( -0.02000000000000000042, -1.944084441611813707, -0.4562887203618206655 ) ) ;
#3278 = EDGE_LOOP ( 'NONE', ( #19123, #8535, #12577, #1048 ) ) ;
#3279 = CARTESIAN_POINT ( 'NONE',  ( 0.2018730987858452508, -0.7302160269438148221, 0.3392082505062085640 ) ) ;
#3280 = ORIENTED_EDGE ( 'NONE', *, *, #12547, .F. ) ;
#3281 = CARTESIAN_POINT ( 'NONE',  ( 0.02614423585516349388, -0.6518502750570457360, 0.4684854799394865821 ) ) ;
#3283 = CARTESIAN_POINT ( 'NONE',  ( 0.2038749045098602886, -1.364881829950852721, 0.4182417262808790226 ) ) ;
#3282 = CARTESIAN_POINT ( 'NONE',  ( 0.2680263476856213911, -1.006194344260251006, 0.7179568291910547462 ) ) ;
#3284 = DIRECTION ( 'NONE',  ( 1.000000000000000000, 0.000000000000000000, 0.000000000000000000 ) ) ;
#3285 = CARTESIAN_POINT ( 'NONE',  ( 0.01217390823686615060, -0.4283984760907826872, 0.1286254401998236097 ) ) ;
#3286 = APPROVAL_STATUS ( 'not_yet_approved' ) ;
#3287 = DIRECTION ( 'NONE',  ( 0.000000000000000000, 0.000000000000000000, -1.000000000000000000 ) ) ;
#3289 = ORIENTED_EDGE ( 'NONE', *, *, #13186, .F. ) ;
#3288 = ORIENTED_EDGE ( 'NONE', *, *, #5421, .T. ) ;
#3290 = DIRECTION ( 'NONE',  ( -1.000000000000000000, -6.779273404243070203E-32, -4.314083075427408311E-32 ) ) ;
#3291 = CARTESIAN_POINT ( 'NONE',  ( 0.1852697703518008665, -0.8388889655799581790, 0.1410250186500984493 ) ) ;
#3292 = CARTESIAN_POINT ( 'NONE',  ( -0.04760454375021171830, -0.4700983808485184046, 0.1075238135162354253 ) ) ;
#3293 = CARTESIAN_POINT ( 'NONE',  ( 0.5861427556958135332, -1.492383513481604362, 0.5940502790402875100 ) ) ;
#3294 = CARTESIAN_POINT ( 'NONE',  ( 0.2009823985145610392, -0.8991965598532170034, 0.5949443444603982334 ) ) ;
#3295 = CARTESIAN_POINT ( 'NONE',  ( 0.2682897491456118222, -1.618043430020381646, 0.8112229545981489709 ) ) ;
#3296 = CARTESIAN_POINT ( 'NONE',  ( 0.02257819890113409514, -0.5399740301406672494, 0.4766629420431791608 ) ) ;
#3297 = CARTESIAN_POINT ( 'NONE',  ( 0.4469283285619459201, -1.099869350908816878, -0.4033480720695140631 ) ) ;
#3298 = FACE_OUTER_BOUND ( 'NONE', #22679, .T. ) ;
#3299 = DIRECTION ( 'NONE',  ( -0.4999999999999968359, 0.8555732718332328401, 0.1341431195573592750 ) ) ;
#3300 = DIRECTION ( 'NONE',  ( -1.000000000000000000, -0.000000000000000000, -0.000000000000000000 ) ) ;
#3301 = CARTESIAN_POINT ( 'NONE',  ( 0.5140835254510695007, -1.350566565279668119, 0.5182417262812423209 ) ) ;
#3302 = CONICAL_SURFACE ( 'NONE', #11179, 0.04999999999999994726, 1.047197551196598964 ) ;
#3303 = CARTESIAN_POINT ( 'NONE',  ( 0.04230170315644018325, -0.2824006788359444409, 0.3740536075335759159 ) ) ;
#3304 = CARTESIAN_POINT ( 'NONE',  ( -0.08000000000000000167, -1.851224977018630868, -0.7958870385335592434 ) ) ;
#3305 = CARTESIAN_POINT ( 'NONE',  ( 0.09388211606716308222, -1.317406247416022858, 0.7243147876381810235 ) ) ;
#3306 = DATE_AND_TIME ( #31496, #15512 ) ;
#3307 = CIRCLE ( 'NONE', #3977, 0.01499999999999999424 ) ;
#3308 = CARTESIAN_POINT ( 'NONE',  ( 0.7044564683220037038, -1.517225624775331072, 0.5721507375637494563 ) ) ;
#3309 = VERTEX_POINT ( 'NONE', #18178 ) ;
#3310 = DIRECTION ( 'NONE',  ( -1.000000000000000000, -0.000000000000000000, -0.000000000000000000 ) ) ;
#3311 = ORIENTED_EDGE ( 'NONE', *, *, #25118, .F. ) ;
#3312 = CARTESIAN_POINT ( 'NONE',  ( 0.4694390894638814093, -1.155687545037050956, -0.4112888527604742772 ) ) ;
#3313 = CARTESIAN_POINT ( 'NONE',  ( 0.2709798375537315063, -1.666113143576919642, 0.7428107703390531835 ) ) ;
#3314 = CARTESIAN_POINT ( 'NONE',  ( 0.5947316391157766446, -1.487148168449749619, 0.5691497089179062829 ) ) ;
#3316 = ORIENTED_EDGE ( 'NONE', *, *, #9778, .T. ) ;
#3315 = CARTESIAN_POINT ( 'NONE',  ( 0.5436011381715165625, -1.169374965638590558, 0.5906050259210040565 ) ) ;
#3318 = EDGE_LOOP ( 'NONE', ( #13637, #9817 ) ) ;
#3317 = VERTEX_POINT ( 'NONE', #36698 ) ;
#3319 = CARTESIAN_POINT ( 'NONE',  ( -0.02953079040095700838, 0.000000000000000000, 0.000000000000000000 ) ) ;
#3320 = VERTEX_POINT ( 'NONE', #9111 ) ;
#3321 = CARTESIAN_POINT ( 'NONE',  ( 0.3322271507484021447, -1.669294652568602988, -0.6327274659999716500 ) ) ;
#3322 = CARTESIAN_POINT ( 'NONE',  ( 0.4860430332212200000, -1.937050167757587760, 0.5182417262812423209 ) ) ;
#3323 = DATE_AND_TIME ( #6818, #33930 ) ;
#3324 = AXIS2_PLACEMENT_3D ( 'NONE', #11987, #21473, #2731 ) ;
#3325 = DIRECTION ( 'NONE',  ( -0.4999551463232372872, 0.8660512985181134660, 0.000000000000000000 ) ) ;
#3326 = ORIENTED_EDGE ( 'NONE', *, *, #40406, .F. ) ;
#3327 = ADVANCED_FACE ( 'NONE', ( #8506 ), #36462, .T. ) ;
#3328 = EDGE_CURVE ( 'NONE', #35047, #21906, #30730, .T. ) ;
#3329 = CARTESIAN_POINT ( 'NONE',  ( 0.08809811930380141709, -0.7701783715479050274, 0.2329054462128774816 ) ) ;
#3330 = CARTESIAN_POINT ( 'NONE',  ( 0.08990936761271779709, -0.5436479961250808568, 0.1446695161202876112 ) ) ;
#3331 = TOROIDAL_SURFACE ( 'NONE', #7252, 0.04500000000000023426, 0.01499999999999999944 ) ;
#3332 = CARTESIAN_POINT ( 'NONE',  ( 0.5250712364136614907, -1.526826414575088053, 0.5708821469565591444 ) ) ;
#3333 = CARTESIAN_POINT ( 'NONE',  ( -0.02000000000000000042, -2.183180860297908144, -0.4937760292030871079 ) ) ;
#3334 = CARTESIAN_POINT ( 'NONE',  ( -0.1595531559346308192, 0.4954596757340662960, 0.1197284696570143359 ) ) ;
#3335 = AXIS2_PLACEMENT_3D ( 'NONE', #11867, #5275, #11482 ) ;
#3336 = ORIENTED_EDGE ( 'NONE', *, *, #33349, .T. ) ;
#3338 = EDGE_CURVE ( 'NONE', #19341, #545, #19844, .T. ) ;
#3337 = VECTOR ( 'NONE', #6874, 39.37007874015748854 ) ;
#3339 = CARTESIAN_POINT ( 'NONE',  ( 0.4117959629386627185, -1.718119050787106250, 0.6105174604612256806 ) ) ;
#3340 = CARTESIAN_POINT ( 'NONE',  ( 0.6726913636366114169, -1.388499336029741515, 0.7397682110044472292 ) ) ;
#3341 = EDGE_CURVE ( 'NONE', #1885, #20917, #17765, .T. ) ;
#3342 = CARTESIAN_POINT ( 'NONE',  ( 0.5674346215910480717, -1.617636063460796025, 0.5669677346690390474 ) ) ;
#3343 = B_SPLINE_CURVE_WITH_KNOTS ( 'NONE', 3,
 ( #5754, #38040, #28790, #9661, #28380, #13138 ),
 .UNSPECIFIED., .F., .F.,
 ( 4, 2, 4 ),
 ( 0.000000000000000000, 0.0005522092370844346697, 0.001104418474168869339 ),
 .UNSPECIFIED. ) ;
#3344 = CARTESIAN_POINT ( 'NONE',  ( 0.5127413057567625776, -1.344192398881990602, 0.8010895931681089044 ) ) ;
#3345 = CARTESIAN_POINT ( 'NONE',  ( -0.1969433606228599420, 0.5138636982738220560, 0.3032895567580801144 ) ) ;
#3346 = CARTESIAN_POINT ( 'NONE',  ( -0.1059790098053070145, -0.4816261856389995044, 0.09813923389061121605 ) ) ;
#3347 = CARTESIAN_POINT ( 'NONE',  ( 0.03662792686184266483, -0.4685177067346144031, -0.1089945633920614554 ) ) ;
#3348 = CARTESIAN_POINT ( 'NONE',  ( 0.05651694441833610832, -1.310850388052192894, 0.6148622741790434887 ) ) ;
#3349 = CARTESIAN_POINT ( 'NONE',  ( 0.1843752803354802849, -0.7900634509218503743, 0.1457185332388700461 ) ) ;
#3350 = PERSON_AND_ORGANIZATION ( #28500, #32463 ) ;
#3351 = CARTESIAN_POINT ( 'NONE',  ( -0.02953079040095700838, -0.4684706630666085614, 0.2484463060367459175 ) ) ;
#3352 = EDGE_CURVE ( 'NONE', #22491, #27922, #31220, .T. ) ;
#3353 = APPLIED_PERSON_AND_ORGANIZATION_ASSIGNMENT ( #12834, #3959, ( #36468 ) ) ;
#3354 = AXIS2_PLACEMENT_3D ( 'NONE', #9615, #10231, #22801 ) ;
#3355 = CARTESIAN_POINT ( 'NONE',  ( 0.05999999999999990757, 0.5386841146467193919, -0.2575246450067292248 ) ) ;
#3356 = AXIS2_PLACEMENT_3D ( 'NONE', #27355, #15187, #5915 ) ;
#3357 = CARTESIAN_POINT ( 'NONE',  ( -0.04229883635638143069, -0.004358580242002279247, 0.4686119955506233281 ) ) ;
#3358 = AXIS2_PLACEMENT_3D ( 'NONE', #17795, #24201, #36725 ) ;
#3359 = ORIENTED_EDGE ( 'NONE', *, *, #7666, .T. ) ;
#3360 = CARTESIAN_POINT ( 'NONE',  ( -0.1205378779716004267, 0.06113703066755032944, -0.04122227111665026367 ) ) ;
#3361 = CIRCLE ( 'NONE', #36783, 0.6114999999999938263 ) ;
#3362 = FACE_OUTER_BOUND ( 'NONE', #22808, .T. ) ;
#3363 = AXIS2_PLACEMENT_3D ( 'NONE', #8148, #7749, #39015 ) ;
#3364 = FACE_OUTER_BOUND ( 'NONE', #27165, .T. ) ;
#3365 = VERTEX_POINT ( 'NONE', #30530 ) ;
#3366 = CARTESIAN_POINT ( 'NONE',  ( 0.4089992519647981384, -1.131314579718122992, 0.3157417262808777658 ) ) ;
#3367 = CARTESIAN_POINT ( 'NONE',  ( 0.1711433029897516944, -1.377856651617054062, 0.6045512896720135476 ) ) ;
#3369 = VERTEX_POINT ( 'NONE', #15295 ) ;
#3368 = ORIENTED_EDGE ( 'NONE', *, *, #38043, .F. ) ;
#3370 = DIRECTION ( 'NONE',  ( 0.000000000000000000, -0.9510565162951650775, -0.3090169943749118686 ) ) ;
#3371 = ORIENTED_EDGE ( 'NONE', *, *, #24745, .T. ) ;
#3372 = CARTESIAN_POINT ( 'NONE',  ( 0.3273012371184206293, -1.767032042405956904, 0.5424971694272759937 ) ) ;
#3373 = CARTESIAN_POINT ( 'NONE',  ( 0.3826493285555479518, -1.694417038293525524, -0.3356002933695534374 ) ) ;
#3375 = CARTESIAN_POINT ( 'NONE',  ( 2.048885995248197414E-16, 0.2900000000000004796, -5.122214988120493288E-16 ) ) ;
#3374 = FACE_OUTER_BOUND ( 'NONE', #22473, .T. ) ;
#3376 = CARTESIAN_POINT ( 'NONE',  ( 0.05269111014006448712, -0.2680748163012488527, -0.3844616952933890830 ) ) ;
#3377 = ORIENTED_EDGE ( 'NONE', *, *, #35859, .T. ) ;
#3378 = AXIS2_PLACEMENT_3D ( 'NONE', #3057, #25883, #16215 ) ;
#3379 = CARTESIAN_POINT ( 'NONE',  ( -0.03158843595483510486, 0.2432919444504241524, -0.4277514783322111658 ) ) ;
#3380 = ORIENTED_EDGE ( 'NONE', *, *, #7469, .T. ) ;
#3381 = ORIENTED_EDGE ( 'NONE', *, *, #18262, .T. ) ;
#3382 = CARTESIAN_POINT ( 'NONE',  ( 0.09071780102537924106, -0.6083146503190497434, 0.1978526169899092468 ) ) ;
#3383 = ORIENTED_EDGE ( 'NONE', *, *, #31153, .F. ) ;
#3384 = ORIENTED_EDGE ( 'NONE', *, *, #4625, .T. ) ;
#3385 = EDGE_CURVE ( 'NONE', #33435, #17597, #6238, .T. ) ;
#3386 = FACE_BOUND ( 'NONE', #25931, .T. ) ;
#3387 = CARTESIAN_POINT ( 'NONE',  ( 0.4410457167306740534, -1.573541075230501241, 0.5635949220671795379 ) ) ;
#3388 = FACE_OUTER_BOUND ( 'NONE', #15781, .T. ) ;
#3389 = CARTESIAN_POINT ( 'NONE',  ( 0.3031470318619229887, -1.653998006306516055, -0.3710263027724181040 ) ) ;
#3390 = CARTESIAN_POINT ( 'NONE',  ( 0.2803729568343131806, -0.9884757496409375399, 0.5728653952958084883 ) ) ;
#3391 = ADVANCED_FACE ( 'NONE', ( #27036 ), #31859, .F. ) ;
#3392 = VECTOR ( 'NONE', #28196, 39.37007874015748143 ) ;
#3393 = ADVANCED_FACE ( 'NONE', ( #5405 ), #25324, .F. ) ;
#3394 = CYLINDRICAL_SURFACE ( 'NONE', #8812, 0.06250000000000001388 ) ;
#3395 = CARTESIAN_POINT ( 'NONE',  ( 0.1887530776919918163, -0.4596756685375818496, 0.1557014379196421383 ) ) ;
#3396 = EDGE_CURVE ( 'NONE', #37512, #15646, #7557, .T. ) ;
#3397 = CARTESIAN_POINT ( 'NONE',  ( 0.5818399341603623931, -1.494769269184020866, 0.5993433759778750147 ) ) ;
#3398 = CARTESIAN_POINT ( 'NONE',  ( -0.05283710938261135942, 0.3063690517300509675, 0.3541964274677629754 ) ) ;
#3399 = AXIS2_PLACEMENT_3D ( 'NONE', #5164, #11350, #40130 ) ;
#3400 = DIRECTION ( 'NONE',  ( 1.664003471950577032E-31, 3.330669073875470114E-16, 1.000000000000000000 ) ) ;
#3401 = FACE_OUTER_BOUND ( 'NONE', #6161, .T. ) ;
#3402 = AXIS2_PLACEMENT_3D ( 'NONE', #1186, #30279, #8475 ) ;
#3403 = CARTESIAN_POINT ( 'NONE',  ( 0.1127117262141932863, -0.6977186850741163848, 0.5101031591922252639 ) ) ;
#3404 = PLANE ( 'NONE',  #40456 ) ;
#3405 = CARTESIAN_POINT ( 'NONE',  ( 0.2529714763052502979, -0.7233805682233873657, 0.5452257223911994855 ) ) ;
#3406 = CARTESIAN_POINT ( 'NONE',  ( 0.4051896412206086873, -1.145861017645314783, 0.4245813808998249450 ) ) ;
#3407 = EDGE_CURVE ( 'NONE', #25927, #37283, #33816, .T. ) ;
#3408 = CARTESIAN_POINT ( 'NONE',  ( 0.05758214410466930278, -1.240647563727545144, 0.6561832231837511076 ) ) ;
#3409 = CARTESIAN_POINT ( 'NONE',  ( 0.6126544994249021325, -1.576059959616806561, -0.4529311371484831539 ) ) ;
#3410 = DIRECTION ( 'NONE',  ( 0.000000000000000000, 0.000000000000000000, -1.000000000000000000 ) ) ;
#3411 = CARTESIAN_POINT ( 'NONE',  ( 0.3984114568195522010, -1.599003643269838904, -0.5155029497116575543 ) ) ;
#3412 = CARTESIAN_POINT ( 'NONE',  ( 0.2637479789745994507, -0.6009450727723176788, 0.1023043458361303365 ) ) ;
#3413 = CARTESIAN_POINT ( 'NONE',  ( 0.7749447939048204059, -1.514576267321142256, -0.5155029497116575543 ) ) ;
#3414 = VERTEX_POINT ( 'NONE', #31948 ) ;
#3415 = CARTESIAN_POINT ( 'NONE',  ( -0.2399999999999999079, -1.832519782180105805, -0.1219017476496882246 ) ) ;
#3416 = CARTESIAN_POINT ( 'NONE',  ( 0.4614790457781012822, -1.239149285203732687, 0.7960982376345531186 ) ) ;
#3417 = CARTESIAN_POINT ( 'NONE',  ( 0.1999999999999794720, -2.097675824466503247, -0.2588528740066096678 ) ) ;
#3418 = VECTOR ( 'NONE', #25725, 39.37007874015748143 ) ;
#3419 = DIRECTION ( 'NONE',  ( 0.8660512985181136880, 0.4999551463232369541, 0.000000000000000000 ) ) ;
#3420 = CARTESIAN_POINT ( 'NONE',  ( -0.05283094505690077991, -0.03968992937477339167, 0.4666439588235272162 ) ) ;
#3421 = PERSON ( 'NAUO-PER18', 'UNSPECIFIED', 'UNSPECIFIED', ('UNSPECIFIED'), ('UNSPECIFIED'), ('UNSPECIFIED') ) ;
#3422 = ORIENTED_EDGE ( 'NONE', *, *, #12408, .F. ) ;
#3423 = CARTESIAN_POINT ( 'NONE',  ( 0.5445533481859567981, -1.664896911350843389, -0.5554955765310773952 ) ) ;
#3424 = AXIS2_PLACEMENT_3D ( 'NONE', #6422, #25379, #37912 ) ;
#3425 = TOROIDAL_SURFACE ( 'NONE', #26435, 0.04749999999977547877, 0.01000000000000000021 ) ;
#3426 = CARTESIAN_POINT ( 'NONE',  ( 0.1872855758231053713, -1.374285790641261329, 0.4677874389472473915 ) ) ;
#3427 = DIRECTION ( 'NONE',  ( 0.000000000000000000, 0.000000000000000000, -1.000000000000000000 ) ) ;
#3428 = CARTESIAN_POINT ( 'NONE',  ( 0.04946426091936732133, 0.3082279967728599468, -0.3644356914998777563 ) ) ;
#3429 = AXIS2_PLACEMENT_3D ( 'NONE', #7064, #25603, #25411 ) ;
#3430 = CARTESIAN_POINT ( 'NONE',  ( 0.5010253830127560093, -1.294911479982484348, 0.5984545886549959004 ) ) ;
#3432 = FACE_OUTER_BOUND ( 'NONE', #37588, .T. ) ;
#3431 = DIRECTION ( 'NONE',  ( 0.0001066307966871704452, -1.551735798909009237E-06, -0.9999999943137325431 ) ) ;
#3433 = CARTESIAN_POINT ( 'NONE',  ( 0.4383612739836618144, -1.052766492039166391, 0.6342478131430038246 ) ) ;
#3434 = ORIENTED_EDGE ( 'NONE', *, *, #4412, .F. ) ;
#3435 = SECURITY_CLASSIFICATION_LEVEL ( 'unclassified' ) ;
#3436 = CARTESIAN_POINT ( 'NONE',  ( 0.05062930621939953219, -1.075691773360101466, 0.7334325894009673386 ) ) ;
#3437 = ORIENTED_EDGE ( 'NONE', *, *, #7884, .F. ) ;
#3438 = EDGE_CURVE ( 'NONE', #39658, #5888, #18802, .T. ) ;
#3439 = CARTESIAN_POINT ( 'NONE',  ( 0.3847140583749202869, -1.605421369524298703, 0.5663922353625259198 ) ) ;
#3441 = CARTESIAN_POINT ( 'NONE',  ( 0.1127291481688585117, -0.7509215673570545091, -0.08735086836678220001 ) ) ;
#3440 = DIRECTION ( 'NONE',  ( 0.8660512985181136880, 0.4999551463232368431, 0.000000000000000000 ) ) ;
#3442 = CARTESIAN_POINT ( 'NONE',  ( 0.06918013971839866161, -0.5399928739580638348, 0.1359763300881502157 ) ) ;
#3443 = EDGE_LOOP ( 'NONE', ( #40262, #19545 ) ) ;
#3444 = EDGE_CURVE ( 'NONE', #4902, #34794, #8533, .T. ) ;
#3445 = EDGE_LOOP ( 'NONE', ( #3186, #24154, #21307, #36770 ) ) ;
#3446 = ORIENTED_EDGE ( 'NONE', *, *, #1612, .T. ) ;
#3447 = CARTESIAN_POINT ( 'NONE',  ( -0.1210148435730035998, -0.5061394519556905447, 0.1438724812234790928 ) ) ;
#3448 = EDGE_CURVE ( 'NONE', #9944, #16485, #22106, .T. ) ;
#3449 = CARTESIAN_POINT ( 'NONE',  ( 0.1830018851694050763, -0.7784347268374490758, 0.5945923564955621909 ) ) ;
#3450 = ORIENTED_EDGE ( 'NONE', *, *, #35646, .T. ) ;
#3451 = CARTESIAN_POINT ( 'NONE',  ( 0.3901895921616377327, -1.764522914000479670, -0.5281946013978575660 ) ) ;
#3452 = CARTESIAN_POINT ( 'NONE',  ( 0.06943685245347047674, -1.818941598116789793, -0.3556487151594290297 ) ) ;
#3453 = FACE_OUTER_BOUND ( 'NONE', #26820, .T. ) ;
#3454 = FACE_OUTER_BOUND ( 'NONE', #19720, .T. ) ;
#3455 = ORIENTED_EDGE ( 'NONE', *, *, #3338, .F. ) ;
#3456 = DIRECTION ( 'NONE',  ( 5.551115123125956498E-17, 0.000000000000000000, -1.000000000000000000 ) ) ;
#3457 = AXIS2_PLACEMENT_3D ( 'NONE', #16722, #23320, #38915 ) ;
#3458 = CARTESIAN_POINT ( 'NONE',  ( 0.4384682549770916871, -1.691311010828499883, 0.6110381959906349136 ) ) ;
#3459 = CARTESIAN_POINT ( 'NONE',  ( -0.01548846960707531660, -0.2306506793134033284, 0.4716198300880330985 ) ) ;
#3460 = CARTESIAN_POINT ( 'NONE',  ( 0.6396239940202712582, -1.336901993116134779, 0.8551876651762376769 ) ) ;
#3461 = TOROIDAL_SURFACE ( 'NONE', #28419, 0.04749999999977547877, 0.01000000000000000021 ) ;
#3462 = CARTESIAN_POINT ( 'NONE',  ( 0.3989074838267503975, -2.038165485489161988, -0.7120309709640824103 ) ) ;
#3463 = CIRCLE ( 'NONE', #26458, 0.03000000000000003011 ) ;
#3464 = FACE_OUTER_BOUND ( 'NONE', #5660, .T. ) ;
#3465 = EDGE_CURVE ( 'NONE', #39975, #28758, #19391, .T. ) ;
#3466 = DIRECTION ( 'NONE',  ( 0.7432428574091918261, 0.4290601401620685040, 0.5133200278913008230 ) ) ;
#3467 = DIRECTION ( 'NONE',  ( 0.000000000000000000, 0.5877852522924454926, 0.8090169943749673243 ) ) ;
#3468 = APPROVAL_DATE_TIME ( #21791, #13450 ) ;
#3469 = EDGE_CURVE ( 'NONE', #5749, #36473, #18838, .T. ) ;
#3470 = VECTOR ( 'NONE', #28984, 39.37007874015748854 ) ;
#3471 = CARTESIAN_POINT ( 'NONE',  ( 0.4083208966368579995, -1.036284369767852764, 0.6331064141399478373 ) ) ;
#3472 = ADVANCED_FACE ( 'NONE', ( #28857 ), #18584, .F. ) ;
#3473 = FACE_OUTER_BOUND ( 'NONE', #20117, .T. ) ;
#3474 = CARTESIAN_POINT ( 'NONE',  ( 0.5145478920242605447, -1.185611792012001509, 0.6057417262811334302 ) ) ;
#3475 = LINE ( 'NONE', #25293, #11386 ) ;
#3476 = CARTESIAN_POINT ( 'NONE',  ( 0.02760435326350026836, -0.9850525496912549972, 0.6581503728771671557 ) ) ;
#3477 = CARTESIAN_POINT ( 'NONE',  ( 0.5935452302802395330, -1.483994409378550206, -0.3858431232416580370 ) ) ;
#3478 = CARTESIAN_POINT ( 'NONE',  ( 0.3704697912810945848, -1.166474544107110267, 0.4182417262808778013 ) ) ;
#3479 = ORIENTED_EDGE ( 'NONE', *, *, #14836, .T. ) ;
#3480 = ORIENTED_EDGE ( 'NONE', *, *, #16792, .F. ) ;
#3481 =( BOUNDED_SURFACE ( )  B_SPLINE_SURFACE ( 3, 2, ( 
 ( #5182, #8481, #11777 ),
 ( #39348, #39757, #39537 ),
 ( #11169, #17736, #1926 ),
 ( #21042, #33379, #5382 ),
 ( #23725, #4987, #10984 ),
 ( #33567, #14442, #23543 ),
 ( #36253, #39157, #8286 ),
 ( #27010, #24334, #20856 ) ),
 .UNSPECIFIED., .F., .F., .T. ) 
 B_SPLINE_SURFACE_WITH_KNOTS ( ( 4, 2, 2, 4 ),
 ( 3, 3 ),
 ( -1.735946658636840947E-05, 0.003182886954856570336, 0.004783010165578039860, 0.006383133376299508950 ),
 ( 0.000000000000000000, 1.000000000000000000 ),
 .UNSPECIFIED. ) 
 GEOMETRIC_REPRESENTATION_ITEM ( )  RATIONAL_B_SPLINE_SURFACE ( (
 ( 1.000000000000000000, 1.000000000000000000, 1.000000000000000000),
 ( 1.000000000000000000, 0.9999683261267254819, 1.000000000000000000),
 ( 1.000000000000000000, 0.9925635664889210785, 1.000000000000000000),
 ( 1.000000000000000000, 0.9822629114585049726, 1.000000000000000000),
 ( 1.000000000000000000, 0.9789426092108594046, 1.000000000000000000),
 ( 1.000000000000000000, 0.9749055716457132315, 1.000000000000000000),
 ( 1.000000000000000000, 0.9741944405893343539, 1.000000000000000000),
 ( 1.000000000000000000, 0.9760960752155037889, 1.000000000000000000) ) ) 
 REPRESENTATION_ITEM ( '' )  SURFACE ( )  );
#3482 = ORIENTED_EDGE ( 'NONE', *, *, #8005, .F. ) ;
#3483 = CARTESIAN_POINT ( 'NONE',  ( -0.02869712619511944132, 0.06034133159976073219, 0.4947855140619930592 ) ) ;
#3484 = DIRECTION ( 'NONE',  ( 0.000000000000000000, -1.000000000000000000, 0.000000000000000000 ) ) ;
#3485 = VECTOR ( 'NONE', #22618, 39.37007874015748143 ) ;
#3486 = CARTESIAN_POINT ( 'NONE',  ( 0.5760521384482631957, -1.423519085382992433, 0.6171703776866719338 ) ) ;
#3488 = VERTEX_POINT ( 'NONE', #31352 ) ;
#3487 = CARTESIAN_POINT ( 'NONE',  ( 0.1499999999999996336, -0.3232818887608602809, 0.4449593469062218531 ) ) ;
#3489 = ORIENTED_EDGE ( 'NONE', *, *, #39169, .F. ) ;
#3490 = CARTESIAN_POINT ( 'NONE',  ( 0.5904407432689540158, -1.601769558089914502, 0.4345720983630151357 ) ) ;
#3491 = VECTOR ( 'NONE', #10270, 39.37007874015748143 ) ;
#3492 = EDGE_LOOP ( 'NONE', ( #32968, #35680, #2896, #31463 ) ) ;
#3493 = AXIS2_PLACEMENT_3D ( 'NONE', #15473, #1783, #24184 ) ;
#3494 = CARTESIAN_POINT ( 'NONE',  ( 0.01170032160320996946, -0.5546732792797903766, 0.2570475303832205349 ) ) ;
#3496 = FACE_OUTER_BOUND ( 'NONE', #9241, .T. ) ;
#3495 = CARTESIAN_POINT ( 'NONE',  ( 0.6427111490925289106, -1.572123239621654900, 0.4256043397410034790 ) ) ;
#3497 = SPHERICAL_SURFACE ( 'NONE', #8266, 0.01499999999999999944 ) ;
#3498 = CARTESIAN_POINT ( 'NONE',  ( 0.01198570820082700897, -0.4922037379152022218, -0.02535380372549751390 ) ) ;
#3499 = AXIS2_PLACEMENT_3D ( 'NONE', #7808, #10102, #35207 ) ;
#3500 = EDGE_CURVE ( 'NONE', #16124, #5597, #18085, .T. ) ;
#3501 = CARTESIAN_POINT ( 'NONE',  ( -0.1211759891752730300, -0.5069122841110217381, 0.3093762286737222755 ) ) ;
#3503 = ORIENTED_EDGE ( 'NONE', *, *, #6468, .T. ) ;
#3502 = ORIENTED_EDGE ( 'NONE', *, *, #34273, .T. ) ;
#3504 = EDGE_CURVE ( 'NONE', #26250, #24229, #10192, .T. ) ;
#3505 = CYLINDRICAL_SURFACE ( 'NONE', #11265, 0.1033070866141732880 ) ;
#3506 = CARTESIAN_POINT ( 'NONE',  ( 0.1852697703518018935, -0.8388889655799397493, 0.1449575636331411899 ) ) ;
#3507 = CONICAL_SURFACE ( 'NONE', #10082, 0.1624877031048690135, 0.1745329251994329756 ) ;
#3508 = CARTESIAN_POINT ( 'NONE',  ( -0.03171102739523275899, -0.4481073524712075318, 0.2027236177532028560 ) ) ;
#3509 = DIRECTION ( 'NONE',  ( 0.000000000000000000, -0.8063205929144885431, 0.5914787413272156735 ) ) ;
#3510 =( GEOMETRIC_REPRESENTATION_CONTEXT ( 3 ) GLOBAL_UNCERTAINTY_ASSIGNED_CONTEXT ( ( #573 ) ) GLOBAL_UNIT_ASSIGNED_CONTEXT ( ( #35025, #6622, #18807 ) ) REPRESENTATION_CONTEXT ( 'NONE', 'WORKASPACE' ) );
#3511 = CARTESIAN_POINT ( 'NONE',  ( 0.1723377558215138383, -0.8672015974434073016, 0.5125204039364767983 ) ) ;
#3512 = CARTESIAN_POINT ( 'NONE',  ( 0.01058981954642434879, -0.5333385045931418045, 0.1834384537311664620 ) ) ;
#3513 = CARTESIAN_POINT ( 'NONE',  ( 0.2812803162299816750, -1.541674682308305844, 0.9904418111512126588 ) ) ;
#3514 = CARTESIAN_POINT ( 'NONE',  ( -0.2399999999999999079, -3.757033409510397881, -0.3216434158294207424 ) ) ;
#3515 = DIRECTION ( 'NONE',  ( 0.000000000000000000, 0.000000000000000000, -1.000000000000000000 ) ) ;
#3516 = LINE ( 'NONE', #9077, #32287 ) ;
#3517 = PLANE ( 'NONE',  #36506 ) ;
#3518 = AXIS2_PLACEMENT_3D ( 'NONE', #1329, #13836, #32764 ) ;
#3519 = DIRECTION ( 'NONE',  ( 0.8660512985181126888, 0.4999551463232384529, 0.000000000000000000 ) ) ;
#3520 = CYLINDRICAL_SURFACE ( 'NONE', #17894, 0.01500000000000001853 ) ;
#3521 = CARTESIAN_POINT ( 'NONE',  ( 0.2138705976722455049, -1.623983589469084832, -0.6628954696135268554 ) ) ;
#3522 = APPROVAL_ROLE ( '' ) ;
#3523 = CIRCLE ( 'NONE', #26524, 0.01500000000000002894 ) ;
#3524 = AXIS2_PLACEMENT_3D ( 'NONE', #27854, #40175, #8705 ) ;
#3525 = CARTESIAN_POINT ( 'NONE',  ( 0.3867682591249857471, -1.703546894211353413, -0.4950309488039767447 ) ) ;
#3526 = CARTESIAN_POINT ( 'NONE',  ( -0.02872242845530507613, 0.4768947642620184335, 0.2371557650701880127 ) ) ;
#3527 = DIRECTION ( 'NONE',  ( 1.000000000000000000, 6.779273404243070203E-32, 4.314083075427408311E-32 ) ) ;
#3528 = TOROIDAL_SURFACE ( 'NONE', #39672, 0.5250000000000000222, 0.01499999999999999944 ) ;
#3529 = CARTESIAN_POINT ( 'NONE',  ( 0.4689530283559364410, -1.130095828402380764, 0.4666897101730458353 ) ) ;
#3530 = ORIENTED_EDGE ( 'NONE', *, *, #38868, .F. ) ;
#3531 = CARTESIAN_POINT ( 'NONE',  ( 0.09046428421607514980, -1.271807512115344485, 0.5182417262812423209 ) ) ;
#3532 = CARTESIAN_POINT ( 'NONE',  ( 0.2595980677342931142, -1.678828727236759244, 0.5659945771154371030 ) ) ;
#3533 = CARTESIAN_POINT ( 'NONE',  ( 0.2774676337662247971, -0.9469401346137602538, 0.7275640284046342998 ) ) ;
#3535 = ORIENTED_EDGE ( 'NONE', *, *, #4922, .F. ) ;
#3534 = CARTESIAN_POINT ( 'NONE',  ( 0.5114276962200751120, -1.674740791407443918, -0.4312833531603950665 ) ) ;
#3537 = ORIENTED_EDGE ( 'NONE', *, *, #143, .T. ) ;
#3536 = VERTEX_POINT ( 'NONE', #6426 ) ;
#3538 = DIRECTION ( 'NONE',  ( -1.000000000000000000, -0.000000000000000000, -0.000000000000000000 ) ) ;
#3539 = ORIENTED_EDGE ( 'NONE', *, *, #27037, .F. ) ;
#3540 = CARTESIAN_POINT ( 'NONE',  ( 0.6442087495854491586, -1.607367720096421815, -0.5688382314396814854 ) ) ;
#3541 = PERSON_AND_ORGANIZATION_ROLE ( 'classification_officer' ) ;
#3542 = AXIS2_PLACEMENT_3D ( 'NONE', #16995, #19282, #35107 ) ;
#3543 = CARTESIAN_POINT ( 'NONE',  ( 0.6590705178848084156, -1.601721441849921268, 0.5182417262812423209 ) ) ;
#3544 = ORIENTED_EDGE ( 'NONE', *, *, #4505, .T. ) ;
#3545 = CARTESIAN_POINT ( 'NONE',  ( 0.2276060635785035757, -0.9284834125224814549, 0.6579476060701295870 ) ) ;
#3546 = VECTOR ( 'NONE', #24189, 39.37007874015748143 ) ;
#3547 = CARTESIAN_POINT ( 'NONE',  ( 0.3622253751127874066, -1.756884464425453984, -0.4902987826081479650 ) ) ;
#3548 = CIRCLE ( 'NONE', #17325, 0.06173076923076910999 ) ;
#3549 = CARTESIAN_POINT ( 'NONE',  ( 0.1156421456406209886, -0.6222233367372450585, 0.3743582360812274246 ) ) ;
#3550 = CARTESIAN_POINT ( 'NONE',  ( 0.3999999999999787059, -2.183180860297921466, -0.4937760292030871079 ) ) ;
#3551 = DIRECTION ( 'NONE',  ( 0.000000000000000000, 3.330669073875470114E-16, 1.000000000000000000 ) ) ;
#3552 = ORIENTED_EDGE ( 'NONE', *, *, #11100, .T. ) ;
#3553 = CARTESIAN_POINT ( 'NONE',  ( -0.01548846960712817709, -0.2450655194479502419, -0.4674710490748132941 ) ) ;
#3554 = CARTESIAN_POINT ( 'NONE',  ( 0.6405997180189585416, -1.336161063724098597, 0.7844527642137872903 ) ) ;
#3555 = B_SPLINE_CURVE_WITH_KNOTS ( 'NONE', 3,
 ( #37452, #19159, #9269, #31492, #15860, #281, #31698, #16079, #28622, #12990, #491, #29009 ),
 .UNSPECIFIED., .F., .F.,
 ( 4, 2, 2, 2, 2, 4 ),
 ( 0.0001995102558408363557, 0.0007825151425067985826, 0.001365520029172760837, 0.001948524915838722874, 0.002240027359171694026, 0.002531529802504664962 ),
 .UNSPECIFIED. ) ;
#3556 = AXIS2_PLACEMENT_3D ( 'NONE', #35780, #33868, #39272 ) ;
#3557 = CARTESIAN_POINT ( 'NONE',  ( 0.4262438152663739488, -1.592651821845863624, -0.6151431148613255573 ) ) ;
#3558 = CARTESIAN_POINT ( 'NONE',  ( 0.6090448915793870155, -1.479032872888494499, 0.5731864665443510143 ) ) ;
#3559 = CIRCLE ( 'NONE', #23285, 0.1600000000000007527 ) ;
#3560 = CARTESIAN_POINT ( 'NONE',  ( 0.1892549258828873926, -0.8411929458066104148, 0.2428197129412378030 ) ) ;
#3561 =( LENGTH_UNIT ( ) NAMED_UNIT ( * ) SI_UNIT ( $, .METRE. ) );
#3562 = CARTESIAN_POINT ( 'NONE',  ( -0.1088121136105144049, -0.4964308608213456875, 0.1000000000000000194 ) ) ;
#3563 = CARTESIAN_POINT ( 'NONE',  ( 0.4357360948072305229, -1.114964732312023532, -0.3896066595063904514 ) ) ;
#3564 = CARTESIAN_POINT ( 'NONE',  ( 0.03359830163007831300, -1.106472467758128353, 0.6807021762515294006 ) ) ;
#3565 = CARTESIAN_POINT ( 'NONE',  ( 0.1860214731903934160, -0.7916887388224913558, 0.2098883466634208494 ) ) ;
#3566 = DATE_AND_TIME ( #26007, #22721 ) ;
#3567 = DIRECTION ( 'NONE',  ( 1.000000000000000000, 6.779273404243070203E-32, 4.314083075427408311E-32 ) ) ;
#3568 = AXIS2_PLACEMENT_3D ( 'NONE', #38135, #19829, #9959 ) ;
#3569 = AXIS2_PLACEMENT_3D ( 'NONE', #4848, #29558, #39016 ) ;
#3570 = CARTESIAN_POINT ( 'NONE',  ( -0.04229956186878666008, 0.4429651807893704163, -0.1531492745855134174 ) ) ;
#3571 = CARTESIAN_POINT ( 'NONE',  ( -0.02242905165738922138, 0.06991915049797693682, 0.5075494376218457893 ) ) ;
#3572 = AXIS2_PLACEMENT_3D ( 'NONE', #18697, #8603, #27556 ) ;
#3573 = ORIENTED_EDGE ( 'NONE', *, *, #19114, .F. ) ;
#3574 = CARTESIAN_POINT ( 'NONE',  ( -0.1324860366999176253, 0.05739311687334418960, -0.02052745314230725732 ) ) ;
#3575 = AXIS2_PLACEMENT_3D ( 'NONE', #25539, #25734, #38067 ) ;
#3576 = CARTESIAN_POINT ( 'NONE',  ( -0.02000000000000000042, -2.589364949149576933, -0.2950346662398796171 ) ) ;
#3577 = CARTESIAN_POINT ( 'NONE',  ( 0.1861044033398533692, -0.8581774586871301347, 0.1812730634833334131 ) ) ;
#3578 = VERTEX_POINT ( 'NONE', #2957 ) ;
#3579 = CARTESIAN_POINT ( 'NONE',  ( 0.05563540667800927902, -1.335270441939011121, 0.5197417262808780025 ) ) ;
#3580 = AXIS2_PLACEMENT_3D ( 'NONE', #39183, #11007, #24356 ) ;
#3581 = CARTESIAN_POINT ( 'NONE',  ( 0.1034500356823820494, -1.184998414006736223, 0.7606213861980615221 ) ) ;
#3583 = VERTEX_POINT ( 'NONE', #38304 ) ;
#3582 = ORIENTED_EDGE ( 'NONE', *, *, #4913, .F. ) ;
#3584 = CARTESIAN_POINT ( 'NONE',  ( 0.4340705412225758231, -1.136956705126083378, 0.5182417262812423209 ) ) ;
#3585 = CIRCLE ( 'NONE', #26603, 0.5215209409081871250 ) ;
#3586 = CARTESIAN_POINT ( 'NONE',  ( 0.08888686490980646226, -1.314157010769999578, 0.4560913452963717973 ) ) ;
#3587 = DIRECTION ( 'NONE',  ( -0.4999551463232371762, 0.8660512985181134660, -0.000000000000000000 ) ) ;
#3589 = CARTESIAN_POINT ( 'NONE',  ( 0.4219866632171650478, -1.610104465087853765, -0.3647299066799348233 ) ) ;
#3588 = CARTESIAN_POINT ( 'NONE',  ( 0.5972966887670781988, -1.597972273499876250, 0.4286416649299261694 ) ) ;
#3590 = CARTESIAN_POINT ( 'NONE',  ( 0.05279755784604436147, -0.3065965315811355341, -0.3541401437853726741 ) ) ;
#3591 = VERTEX_POINT ( 'NONE', #38106 ) ;
#3592 = FACE_OUTER_BOUND ( 'NONE', #35599, .T. ) ;
#3593 = ORIENTED_EDGE ( 'NONE', *, *, #21100, .F. ) ;
#3594 = CARTESIAN_POINT ( 'NONE',  ( 0.2372193036104026098, -0.8972535433454568166, 0.6983280862938940903 ) ) ;
#3595 = ORIENTED_EDGE ( 'NONE', *, *, #11027, .T. ) ;
#3596 = ORIENTED_EDGE ( 'NONE', *, *, #2858, .T. ) ;
#3597 = CARTESIAN_POINT ( 'NONE',  ( 2.583431119901448829E-05, -0.4262564435357387160, 0.1903957133491850640 ) ) ;
#3598 = CARTESIAN_POINT ( 'NONE',  ( 0.4621341988872929574, -1.532972198998491242, 0.7252595559952519366 ) ) ;
#3599 = EDGE_CURVE ( 'NONE', #35563, #23695, #18996, .T. ) ;
#3601 = CARTESIAN_POINT ( 'NONE',  ( -0.1172401355130441442, -0.4876450271195239550, 0.3356658914665608950 ) ) ;
#3600 = CARTESIAN_POINT ( 'NONE',  ( 0.4958944217707210722, -1.624354045237602184, -0.4405887224042038808 ) ) ;
#3602 = CARTESIAN_POINT ( 'NONE',  ( 0.3356530659809335848, -1.635232883418107797, -0.3718853885041787932 ) ) ;
#3603 = CARTESIAN_POINT ( 'NONE',  ( 0.3082980917340821247, -1.007433431510620592, 0.6024509563116612343 ) ) ;
#3604 = APPROVAL ( #5392, 'UNKNOWN' ) ;
#3605 = CIRCLE ( 'NONE', #39745, 0.01000000000000002970 ) ;
#3606 = CARTESIAN_POINT ( 'NONE',  ( -0.2399999999999999079, -3.941790907013290823, -0.4709369376873030477 ) ) ;
#3607 = CARTESIAN_POINT ( 'NONE',  ( 0.4195799131931469139, -1.708669366397955081, -0.5215014756514103622 ) ) ;
#3608 = VECTOR ( 'NONE', #10580, 39.37007874015748143 ) ;
#3609 = CARTESIAN_POINT ( 'NONE',  ( 0.3653257479037889111, -1.126353351805138070, 0.8077794159112313688 ) ) ;
#3610 = CARTESIAN_POINT ( 'NONE',  ( -0.02881302694829762298, 0.3393464602396041307, -0.3647504210684009429 ) ) ;
#3611 = CONICAL_SURFACE ( 'NONE', #26621, 0.1400000000000005684, 1.047197551196600518 ) ;
#3612 = APPROVAL_PERSON_ORGANIZATION ( #25686, #13450, #19110 ) ;
#3613 = CARTESIAN_POINT ( 'NONE',  ( -0.05076541221973945167, -0.4330952608417186211, -0.1921093419630976185 ) ) ;
#3614 = CARTESIAN_POINT ( 'NONE',  ( -0.02000000000000000042, -2.313818782766725146, -0.3979462133327477114 ) ) ;
#3615 = AXIS2_PLACEMENT_3D ( 'NONE', #34066, #33653, #15138 ) ;
#3616 = CARTESIAN_POINT ( 'NONE',  ( 0.6387812025505826830, -1.332167957021822557, 0.7527387398627037873 ) ) ;
#3617 = LINE ( 'NONE', #35474, #10269 ) ;
#3618 = CARTESIAN_POINT ( 'NONE',  ( 0.05061809761307144856, -1.246180169307136154, 0.6688036225518566580 ) ) ;
#3619 = DIRECTION ( 'NONE',  ( 0.000000000000000000, 0.000000000000000000, 1.000000000000000000 ) ) ;
#3620 = CARTESIAN_POINT ( 'NONE',  ( 0.08146015332400738385, -1.318321297778865864, 0.4704503523288164346 ) ) ;
#3621 = EDGE_CURVE ( 'NONE', #27741, #9411, #28446, .T. ) ;
#3622 = CARTESIAN_POINT ( 'NONE',  ( 0.2046378645136894270, -0.9147060450658054398, 0.6214472678333320399 ) ) ;
#3623 = CARTESIAN_POINT ( 'NONE',  ( 0.01895884884825203495, 0.07380796352548452122, 0.5147901372834206013 ) ) ;
#3624 = CARTESIAN_POINT ( 'NONE',  ( 0.6982506810322021140, -1.496459467441635827, 0.4853452239463521556 ) ) ;
#3625 = EDGE_CURVE ( 'NONE', #30050, #27922, #9534, .T. ) ;
#3626 = VERTEX_POINT ( 'NONE', #9728 ) ;
#3627 = DIRECTION ( 'NONE',  ( -0.4492559606623142687, 0.000000000000000000, -0.8934030903289852388 ) ) ;
#3628 = AXIS2_PLACEMENT_3D ( 'NONE', #16065, #15848, #19563 ) ;
#3629 = ADVANCED_FACE ( 'NONE', ( #22298 ), #33163, .F. ) ;
#3630 = DIRECTION ( 'NONE',  ( -0.4999551463232372317, 0.8660512985181135770, -0.000000000000000000 ) ) ;
#3631 = ADVANCED_FACE ( 'NONE', ( #29267 ), #29665, .F. ) ;
#3632 = CARTESIAN_POINT ( 'NONE',  ( 0.3629635513856721563, -1.169857187001789534, 0.4182417262808778013 ) ) ;
#3633 = B_SPLINE_CURVE_WITH_KNOTS ( 'NONE', 3,
 ( #20055, #32372, #33201, #5006, #39556, #17573, #16960, #32782, #36490, #23146, #35883, #27029, #23962, #23560, #11390, #26646, #19837, #29311, #29504, #4791, #17366, #39367 ),
 .UNSPECIFIED., .F., .F.,
 ( 4, 2, 2, 2, 2, 2, 2, 2, 2, 2, 4 ),
 ( 0.000000000000000000, 0.001208936138749878856, 0.002417872277499757711, 0.003022340346874696597, 0.003626808416249635483, 0.004835744554999510218, 0.006044680693749383653, 0.006649148763124320370, 0.007253616832499257955, 0.008462552971249126185, 0.009671489109998996150 ),
 .UNSPECIFIED. ) ;
#3634 = AXIS2_PLACEMENT_3D ( 'NONE', #11347, #24519, #8047 ) ;
#3635 = EDGE_CURVE ( 'NONE', #13015, #38131, #34571, .T. ) ;
#3636 = ORIENTED_EDGE ( 'NONE', *, *, #33352, .F. ) ;
#3637 = CARTESIAN_POINT ( 'NONE',  ( -0.02231181081520667783, -0.2417894035777224948, -0.4519954025055052949 ) ) ;
#3638 = CARTESIAN_POINT ( 'NONE',  ( 0.1156620092545082995, -1.416098910045857862, 0.4676871692938218694 ) ) ;
#3639 = LOCAL_TIME ( 0, 53, 7.000000000000000000, #4975 ) ;
#3640 = DIRECTION ( 'NONE',  ( 1.000000000000000000, -0.000000000000000000, -0.000000000000000000 ) ) ;
#3641 = CARTESIAN_POINT ( 'NONE',  ( 0.1809287994913510722, -1.262837545876212886, -0.7414037396183944528 ) ) ;
#3642 = CARTESIAN_POINT ( 'NONE',  ( 0.5007618516461782576, -1.294244025654331498, 0.6028626338283670227 ) ) ;
#3644 = CARTESIAN_POINT ( 'NONE',  ( 0.3224045394708089374, -1.760747393242730219, 0.4928480064586597265 ) ) ;
#3643 = CARTESIAN_POINT ( 'NONE',  ( 0.03113248654051816583, -3.491513147198973073E-33, 0.6114999999999938263 ) ) ;
#3645 = CARTESIAN_POINT ( 'NONE',  ( 0.4928690250500026293, -1.082673021089655574, 0.5721439028494731405 ) ) ;
#3646 = ORIENTED_EDGE ( 'NONE', *, *, #12679, .T. ) ;
#3647 = CONTEXT_DEPENDENT_SHAPE_REPRESENTATION ( #8217, #38679 ) ;
#3648 = CARTESIAN_POINT ( 'NONE',  ( 0.05865460281497637818, -1.118264395791441101, 0.7485648030501707018 ) ) ;
#3649 = ORIENTED_EDGE ( 'NONE', *, *, #16732, .T. ) ;
#3650 = CARTESIAN_POINT ( 'NONE',  ( 0.1751718594852775535, -1.050137195076516816, 0.8364126339080514283 ) ) ;
#3651 = ADVANCED_FACE ( 'NONE', ( #20221 ), #25998, .F. ) ;
#3653 = CARTESIAN_POINT ( 'NONE',  ( 0.1845297650884798746, -0.8463068900015028317, 0.09522967538727487857 ) ) ;
#3652 = CARTESIAN_POINT ( 'NONE',  ( 0.06557244994597240251, -0.7859005477308489418, 0.03515882536214479798 ) ) ;
#3654 = LINE ( 'NONE', #28336, #783 ) ;
#3655 = APPROVAL ( #26756, 'UNSPECIFIED' ) ;
#3656 = ORIENTED_EDGE ( 'NONE', *, *, #16842, .T. ) ;
#3657 = ORIENTED_EDGE ( 'NONE', *, *, #325, .F. ) ;
#3658 = CARTESIAN_POINT ( 'NONE',  ( 0.4154885538802266520, -1.127358870322865858, 0.5795187171650935110 ) ) ;
#3659 = CARTESIAN_POINT ( 'NONE',  ( 0.1171479976344189378, -0.5695749914720167340, 0.2425808011265505881 ) ) ;
#3660 = ORIENTED_EDGE ( 'NONE', *, *, #10452, .T. ) ;
#3661 = CARTESIAN_POINT ( 'NONE',  ( 0.5221712590809916010, -1.637363247671663746, -0.4217897737303722971 ) ) ;
#3662 = CARTESIAN_POINT ( 'NONE',  ( 0.5429359209136535025, -1.169310040315109545, 0.5682417262808779901 ) ) ;
#3663 = CARTESIAN_POINT ( 'NONE',  ( 0.5967683701461131696, -1.379674245310775760, -0.6250000000000000000 ) ) ;
#3664 = CARTESIAN_POINT ( 'NONE',  ( -0.08000000000000000167, -1.599201040860868339, 0.2442182323853691606 ) ) ;
#3665 = CARTESIAN_POINT ( 'NONE',  ( 0.1909286924077255587, -1.257064795538239022, -0.6485234391946320676 ) ) ;
#3666 = CARTESIAN_POINT ( 'NONE',  ( -0.3000000000000000999, -3.253611865733782693, -0.3464478357516359575 ) ) ;
#3667 = CIRCLE ( 'NONE', #26672, 0.06000000000000031697 ) ;
#3668 = AXIS2_PLACEMENT_3D ( 'NONE', #2359, #24360, #37105 ) ;
#3669 = ADVANCED_FACE ( 'NONE', ( #17322 ), #33173, .T. ) ;
#3670 = B_SPLINE_CURVE_WITH_KNOTS ( 'NONE', 3,
 ( #38488, #16892, #19762, #10708, #35401, #4114, #1681, #26560, #23069, #1088, #35803, #16683, #35596, #20185, #19971, #13600, #26162, #7615, #38682, #4928, #4716, #32507, #39097, #10919, #39293, #32711, #13986, #23487, #7810, #14198, #11115, #23672, #33320, #8422, #39903, #11313, #33723, #21187, #20989, #14592, #30844, #11723, #18304, #8224, #24091, #20798, #40088, #39695, #26950, #36619, #5538, #2665, #18499, #27377, #36410, #24478, #1872, #36802 ),
 .UNSPECIFIED., .F., .F.,
 ( 4, 2, 2, 2, 2, 2, 2, 2, 2, 2, 2, 2, 2, 2, 2, 2, 2, 2, 2, 2, 2, 2, 2, 2, 2, 2, 2, 2, 4 ),
 ( 3.058345997481036509E-05, 0.001707590458248171112, 0.003384597456521531555, 0.005061604454794892648, 0.006738611453068253307, 0.007577114952204934070, 0.008415618451341613099, 0.01009262544961496422, 0.01176963244788831707, 0.01344663944616166992, 0.01512364644443502278, 0.01680065344270836869, 0.01847766044098172328, 0.02015466743925507440, 0.02350868143580178010, 0.02686269543234847887, 0.03021670942889519151, 0.03189371642716854610, 0.03357072342544189375, 0.04027875141853529128, 0.04195575841680863893, 0.04363276541508198658, 0.04698677941162868882, 0.04866378640990204341, 0.05034079340817539105, 0.05201780040644875258, 0.05285630390558542641, 0.05327555565515376679, 0.05369480740472210023 ),
 .UNSPECIFIED. ) ;
#3671 = CARTESIAN_POINT ( 'NONE',  ( 0.6710503155864784297, -1.387729643236325083, 0.8301965501372990941 ) ) ;
#3672 = CARTESIAN_POINT ( 'NONE',  ( 0.3972310942533077704, -2.031578862939333430, -0.5076924364714133775 ) ) ;
#3673 = CARTESIAN_POINT ( 'NONE',  ( 0.4175441604896325543, -1.126814933402447760, 0.5435073546807187572 ) ) ;
#3674 = APPROVAL_STATUS ( 'not_yet_approved' ) ;
#3675 = LOCAL_TIME ( 0, 53, 7.000000000000000000, #37060 ) ;
#3676 = FACE_OUTER_BOUND ( 'NONE', #17737, .T. ) ;
#3677 = CARTESIAN_POINT ( 'NONE',  ( -0.3000000000000000999, -3.753843787845913216, -0.2458487048530572650 ) ) ;
#3678 = PLANE ( 'NONE',  #35645 ) ;
#3679 = AXIS2_PLACEMENT_3D ( 'NONE', #16780, #35087, #26237 ) ;
#3680 = CARTESIAN_POINT ( 'NONE',  ( -0.02000000000000000042, -2.058305985490972212, -0.5970033804171128722 ) ) ;
#3681 = ADVANCED_FACE ( 'NONE', ( #16721 ), #4153, .F. ) ;
#3682 = CARTESIAN_POINT ( 'NONE',  ( 0.1492358308521446464, -1.145521527551625951, 0.9752184947445524665 ) ) ;
#3683 = CARTESIAN_POINT ( 'NONE',  ( 0.0003189345953180242532, -0.4719140995912783354, 0.02086241239832067884 ) ) ;
#3684 = EDGE_CURVE ( 'NONE', #26731, #12540, #20090, .T. ) ;
#3685 = CARTESIAN_POINT ( 'NONE',  ( -0.2399999999999999079, -2.853330612949663170, -0.6088139570729240724 ) ) ;
#3686 = ADVANCED_FACE ( 'NONE', ( #10535 ), #37356, .T. ) ;
#3687 = CARTESIAN_POINT ( 'NONE',  ( 0.2059254672957554211, -1.283047419494637520, -0.2869370717035634177 ) ) ;
#3688 = ADVANCED_FACE ( 'NONE', ( #36037 ), #1069, .T. ) ;
#3689 = EDGE_LOOP ( 'NONE', ( #36122, #15778, #15173, #18265 ) ) ;
#3690 = ORIENTED_EDGE ( 'NONE', *, *, #297, .F. ) ;
#3691 = CARTESIAN_POINT ( 'NONE',  ( 0.3795613398208534384, -1.760143698493221720, -0.5723197561600635863 ) ) ;
#3692 = EDGE_LOOP ( 'NONE', ( #31840, #15078 ) ) ;
#3693 = CARTESIAN_POINT ( 'NONE',  ( 0.03113248654051816583, -0.4415087982045245996, -0.1343585914930099934 ) ) ;
#3694 = CARTESIAN_POINT ( 'NONE',  ( 0.5751110296356755081, -1.612475604602671808, -0.4967019341012566258 ) ) ;
#3695 = DIRECTION ( 'NONE',  ( 1.000000000000000000, -0.000000000000000000, -0.000000000000000000 ) ) ;
#3697 = ORIENTED_EDGE ( 'NONE', *, *, #2435, .F. ) ;
#3696 = DIRECTION ( 'NONE',  ( 1.188678714063518227E-15, -1.000000000000000000, -3.263080277421930985E-16 ) ) ;
#3698 = CIRCLE ( 'NONE', #29984, 0.2000000000000000111 ) ;
#3699 = ORIENTED_EDGE ( 'NONE', *, *, #8675, .F. ) ;
#3700 = CARTESIAN_POINT ( 'NONE',  ( 0.1936486515345767767, -0.8111868380948229484, 0.2874045417164454164 ) ) ;
#3701 = ORIENTED_EDGE ( 'NONE', *, *, #30119, .F. ) ;
#3702 = CARTESIAN_POINT ( 'NONE',  ( 0.01084281108554383498, -0.5360844055732374436, 0.1962519228010750350 ) ) ;
#3703 = ADVANCED_FACE ( 'NONE', ( #1908 ), #9232, .F. ) ;
#3705 = FACE_OUTER_BOUND ( 'NONE', #10575, .T. ) ;
#3704 = CARTESIAN_POINT ( 'NONE',  ( 0.6528690609575362735, -1.559671037451765274, 0.4269390887829667136 ) ) ;
#3706 = FACE_OUTER_BOUND ( 'NONE', #16141, .T. ) ;
#3707 = APPLIED_APPROVAL_ASSIGNMENT ( #19454, ( #28638 ) ) ;
#3708 = LINE ( 'NONE', #3100, #13474 ) ;
#3709 = CARTESIAN_POINT ( 'NONE',  ( 0.09582489096432343645, -1.363102397044379632, -0.3305558606734421701 ) ) ;
#3711 = EDGE_LOOP ( 'NONE', ( #21390, #10679, #29640, #22225, #3539 ) ) ;
#3710 = ORIENTED_EDGE ( 'NONE', *, *, #31086, .F. ) ;
#3712 = EDGE_CURVE ( 'NONE', #9762, #20386, #22715, .T. ) ;
#3713 = CARTESIAN_POINT ( 'NONE',  ( 0.3885328309914510281, -1.773491243725594746, -0.4828692758189210843 ) ) ;
#3714 = CIRCLE ( 'NONE', #22784, 0.1000000000000000056 ) ;
#3715 = CARTESIAN_POINT ( 'NONE',  ( 0.1116628760231743317, -0.9290305928360726995, 0.1898406166415877172 ) ) ;
#3716 = CARTESIAN_POINT ( 'NONE',  ( -0.02242905165738846504, -0.4611019942560602436, 0.2233384654055033669 ) ) ;
#3717 = CARTESIAN_POINT ( 'NONE',  ( 0.5745168371614193248, -1.419270820774067854, 0.7497674921010183402 ) ) ;
#3718 = CARTESIAN_POINT ( 'NONE',  ( 0.3777855516927814961, -1.148309276396616729, 0.7252356322318088688 ) ) ;
#3719 = CARTESIAN_POINT ( 'NONE',  ( 0.07072154735683021387, -0.9109290280001659523, 0.7683321812563286279 ) ) ;
#3720 = CARTESIAN_POINT ( 'NONE',  ( 0.4809147765755076853, -1.118094034716835994, 0.5264152588799988486 ) ) ;
#3721 = B_SPLINE_CURVE_WITH_KNOTS ( 'NONE', 3,
 ( #32617, #4817, #17391, #19867, #32404, #29949, #16794, #29341 ),
 .UNSPECIFIED., .F., .F.,
 ( 4, 2, 2, 4 ),
 ( 0.0001297999473408272800, 0.002093273211076724771, 0.003075009842944673340, 0.004056746474812622343 ),
 .UNSPECIFIED. ) ;
#3722 = DIRECTION ( 'NONE',  ( 8.881784197001245421E-16, -2.361472542561082612E-16, 1.000000000000000000 ) ) ;
#3723 = CARTESIAN_POINT ( 'NONE',  ( -0.3000000000000000999, -2.253314830856113726, -0.6753616220517687507 ) ) ;
#3724 = FACE_OUTER_BOUND ( 'NONE', #11191, .T. ) ;
#3725 = CARTESIAN_POINT ( 'NONE',  ( 0.3247324306352935563, -1.759421949583405365, 0.4854534786567430427 ) ) ;
#3726 = DIRECTION ( 'NONE',  ( 0.8660512985181134660, 0.4999551463232377868, 1.998401444325281773E-15 ) ) ;
#3727 = AXIS2_PLACEMENT_3D ( 'NONE', #27001, #11767, #2106 ) ;
#3728 = CARTESIAN_POINT ( 'NONE',  ( 0.0003933147203880468725, -0.9422125792237651121, 0.2874793698223738203 ) ) ;
#3729 = CARTESIAN_POINT ( 'NONE',  ( 0.06448274526053174305, -1.286806166505041427, 0.5182417262812423209 ) ) ;
#3730 = CARTESIAN_POINT ( 'NONE',  ( 0.1950600887472297151, -2.009716898148788733, -0.6737934748930497486 ) ) ;
#3731 = APPROVAL_DATE_TIME ( #34986, #25245 ) ;
#3732 =( BOUNDED_SURFACE ( )  B_SPLINE_SURFACE ( 3, 2, ( 
 ( #36178, #39273, #1656 ),
 ( #32694, #11096, #4692 ),
 ( #4904, #20970, #1450 ),
 ( #1262, #32884, #4309 ),
 ( #7792, #7987, #27139 ),
 ( #36597, #38853, #29415 ) ),
 .UNSPECIFIED., .F., .F., .F. ) 
 B_SPLINE_SURFACE_WITH_KNOTS ( ( 4, 2, 4 ),
 ( 3, 3 ),
 ( 3.035766082959412415E-18, 0.0004219452060208952896, 0.0008438904120417875434 ),
 ( 0.000000000000000000, 1.000000000000000000 ),
 .UNSPECIFIED. ) 
 GEOMETRIC_REPRESENTATION_ITEM ( )  RATIONAL_B_SPLINE_SURFACE ( (
 ( 1.000000000000000000, 0.8275829691081225681, 1.000000000000000000),
 ( 1.000000000000000000, 0.8234190626268043101, 1.000000000000000000),
 ( 1.000000000000000000, 0.8108491116769944718, 1.000000000000000000),
 ( 1.000000000000000000, 0.7704115495969776628, 1.000000000000000000),
 ( 1.000000000000000000, 0.7425865172308375728, 1.000000000000000000),
 ( 1.000000000000000000, 0.7079223141425768917, 1.000000000000000000) ) ) 
 REPRESENTATION_ITEM ( '' )  SURFACE ( )  );
#3733 = LOCAL_TIME ( 0, 53, 7.000000000000000000, #6003 ) ;
#3734 = CARTESIAN_POINT ( 'NONE',  ( 0.3567436193415031154, -1.868336587247005021, -0.6649533621369776437 ) ) ;
#3735 = EDGE_CURVE ( 'NONE', #5941, #27272, #27198, .T. ) ;
#3736 = CARTESIAN_POINT ( 'NONE',  ( -0.05201840200954667426, 0.4415345355162883512, 0.1624690192511396847 ) ) ;
#3737 = CARTESIAN_POINT ( 'NONE',  ( -0.2746410161513779258, -3.941790907013290823, -0.4709369376873030477 ) ) ;
#3738 = AXIS2_PLACEMENT_3D ( 'NONE', #5563, #5964, #8861 ) ;
#3739 = CARTESIAN_POINT ( 'NONE',  ( -0.08000000000000000167, -2.144840178508589545, -0.3363606153560244616 ) ) ;
#3740 = VERTEX_POINT ( 'NONE', #2510 ) ;
#3741 = CARTESIAN_POINT ( 'NONE',  ( 0.1066313631270083273, -1.413218563028875829, 0.5580310067598821533 ) ) ;
#3742 = CARTESIAN_POINT ( 'NONE',  ( 0.2744681798667284456, -1.667287544441652614, 0.6824681254658000462 ) ) ;
#3743 = CARTESIAN_POINT ( 'NONE',  ( 0.5951897655464796211, -1.487216002287215622, 0.5778840690689636128 ) ) ;
#3745 = VERTEX_POINT ( 'NONE', #3253 ) ;
#3744 = DIRECTION ( 'NONE',  ( 0.000000000000000000, 0.000000000000000000, -1.000000000000000000 ) ) ;
#3747 = ORIENTED_EDGE ( 'NONE', *, *, #8109, .T. ) ;
#3746 = ORIENTED_EDGE ( 'NONE', *, *, #7412, .T. ) ;
#3748 = DIRECTION ( 'NONE',  ( -7.771561172376107616E-16, 7.170354002788761615E-17, -1.000000000000000000 ) ) ;
#3749 = ORIENTED_EDGE ( 'NONE', *, *, #28234, .F. ) ;
#3750 = ORIENTED_EDGE ( 'NONE', *, *, #9731, .T. ) ;
#3751 = DIRECTION ( 'NONE',  ( 0.000000000000000000, 1.000000000000000000, 7.931692224083225994E-17 ) ) ;
#3752 = DIRECTION ( 'NONE',  ( -1.000000000000000000, -7.857794173099924470E-32, -8.628166150854818811E-32 ) ) ;
#3753 = EDGE_CURVE ( 'NONE', #29747, #38278, #5587, .T. ) ;
#3754 = SECURITY_CLASSIFICATION_LEVEL ( 'unclassified' ) ;
#3755 = DIRECTION ( 'NONE',  ( 1.000000000000000000, 0.000000000000000000, 7.847503847416053677E-16 ) ) ;
#3756 = ORIENTED_EDGE ( 'NONE', *, *, #5610, .F. ) ;
#3757 = AXIS2_PLACEMENT_3D ( 'NONE', #18548, #3125, #12183 ) ;
#3758 = ADVANCED_FACE ( 'NONE', ( #39517 ), #35187, .T. ) ;
#3759 = CARTESIAN_POINT ( 'NONE',  ( 0.09447558850840712119, -0.7779443503602000431, 0.3004461803567781142 ) ) ;
#3760 = DIRECTION ( 'NONE',  ( 1.000000000000000000, 2.341930812374887555E-31, -1.664003471950578127E-31 ) ) ;
#3761 = CARTESIAN_POINT ( 'NONE',  ( 0.5396210408343224962, -1.519077833686574230, 0.5827304004285395189 ) ) ;
#3762 = CARTESIAN_POINT ( 'NONE',  ( 0.6353491900406211812, -1.612482177399554351, -0.4775148253361261030 ) ) ;
#3763 = CARTESIAN_POINT ( 'NONE',  ( -0.03654364704248840023, -0.2290829176602870165, 0.4574690890339265237 ) ) ;
#3764 = CARTESIAN_POINT ( 'NONE',  ( -0.1643313925801952735, 0.5105373599712236254, 0.1162626052509350555 ) ) ;
#3765 = CARTESIAN_POINT ( 'NONE',  ( 0.3766692548637607940, -1.738998721234757738, 0.6049789936288398895 ) ) ;
#3766 = CARTESIAN_POINT ( 'NONE',  ( 0.7250766506443707682, -1.477170034539755594, 0.7383090895715118673 ) ) ;
#3767 = CARTESIAN_POINT ( 'NONE',  ( 0.5779297624755960205, -1.623152544610868109, 0.5629341535590222101 ) ) ;
#3768 = CARTESIAN_POINT ( 'NONE',  ( 0.5473208382521128623, -1.395613029667247318, 0.7752695405470998447 ) ) ;
#3769 = DIRECTION ( 'NONE',  ( -1.000000000000000000, -2.280301054154495132E-31, 1.664003471950577689E-31 ) ) ;
#3770 = CARTESIAN_POINT ( 'NONE',  ( 0.1499999999999993561, -0.3688619771572893558, 0.3775276577327004723 ) ) ;
#3771 = CARTESIAN_POINT ( 'NONE',  ( -0.2399999999999999079, -2.477126460671948749, -0.4732852368073287574 ) ) ;
#3772 = CARTESIAN_POINT ( 'NONE',  ( 0.001484713323275439105, -0.9577160478316373293, 0.3237126889746802516 ) ) ;
#3773 = CARTESIAN_POINT ( 'NONE',  ( 0.5138550893713603740, -1.118750960246259307, 0.5715134594416469982 ) ) ;
#3774 = CALENDAR_DATE ( 2026, 13, 10 ) ;
#3775 = FACE_OUTER_BOUND ( 'NONE', #22812, .T. ) ;
#3776 = ADVANCED_FACE ( 'NONE', ( #15803 ), #8259, .T. ) ;
#3777 = CARTESIAN_POINT ( 'NONE',  ( -0.03664605387828201444, 0.4430871221163654727, -0.1871485295462624598 ) ) ;
#3778 = CARTESIAN_POINT ( 'NONE',  ( 0.4393112170097341340, -1.154367431024637236, 0.4182417262808776903 ) ) ;
#3779 = ORIENTED_EDGE ( 'NONE', *, *, #20222, .T. ) ;
#3780 = CARTESIAN_POINT ( 'NONE',  ( 0.4426157458868572037, -1.573711800953075279, 0.5837462811315755618 ) ) ;
#3781 = CARTESIAN_POINT ( 'NONE',  ( 0.002367394983755363291, -0.5282119844061586855, 0.1345257393686825342 ) ) ;
#3782 = CARTESIAN_POINT ( 'NONE',  ( 0.1864731436350384464, -0.8522398885375680466, 0.1983945186742870626 ) ) ;
#3783 = ORIENTED_EDGE ( 'NONE', *, *, #7385, .T. ) ;
#3784 = DIRECTION ( 'NONE',  ( 0.000000000000000000, 0.000000000000000000, -1.000000000000000000 ) ) ;
#3785 = VECTOR ( 'NONE', #10516, 39.37007874015748143 ) ;
#3786 = CARTESIAN_POINT ( 'NONE',  ( 0.1522219036447276519, -1.333917548074724957, 0.6890782258552490269 ) ) ;
#3788 = ORIENTED_EDGE ( 'NONE', *, *, #15994, .T. ) ;
#3787 = VERTEX_POINT ( 'NONE', #5161 ) ;
#3789 = DIRECTION ( 'NONE',  ( 0.000000000000000000, 0.000000000000000000, 1.000000000000000000 ) ) ;
#3790 = DIRECTION ( 'NONE',  ( -0.4999551463232372317, 0.8660512985181135770, -0.000000000000000000 ) ) ;
#3791 = CARTESIAN_POINT ( 'NONE',  ( 0.2369676045672858555, -1.593428264216547596, -0.3535318458821304355 ) ) ;
#3792 = CARTESIAN_POINT ( 'NONE',  ( 0.04762200653274697992, 0.4434980416368364264, 0.1892582844414469612 ) ) ;
#3793 = CARTESIAN_POINT ( 'NONE',  ( 0.03478489236951255031, -0.2420938338886949037, -0.4561872437641432132 ) ) ;
#3794 = VERTEX_POINT ( 'NONE', #11566 ) ;
#3795 = CARTESIAN_POINT ( 'NONE',  ( 0.03411772795726943780, -0.6984928504873072486, 0.8050285864669745051 ) ) ;
#3796 = CARTESIAN_POINT ( 'NONE',  ( 0.1724172692436113929, -0.7740579048028638498, 0.6032149419744345931 ) ) ;
#3797 = CARTESIAN_POINT ( 'NONE',  ( 0.003107293377653203969, -0.4819238241330969785, 0.3575383394813408389 ) ) ;
#3798 = CARTESIAN_POINT ( 'NONE',  ( 0.4691319308531145538, -1.557781732288214815, 0.5635712613440997387 ) ) ;
#3800 = CARTESIAN_POINT ( 'NONE',  ( -0.1123064544305908963, -0.5135141720357597750, 0.3236707397771521055 ) ) ;
#3799 = CARTESIAN_POINT ( 'NONE',  ( 0.4852701934511425286, -1.589624916429106971, -0.4498566476972361006 ) ) ;
#3801 = CARTESIAN_POINT ( 'NONE',  ( 0.5970079706708396605, -1.484385675791830561, 0.4807375746916206505 ) ) ;
#3802 = CARTESIAN_POINT ( 'NONE',  ( 0.4659064572791866143, -1.067879587118542695, 0.6257723985471262962 ) ) ;
#3803 = ORIENTED_EDGE ( 'NONE', *, *, #11426, .F. ) ;
#3804 = CARTESIAN_POINT ( 'NONE',  ( 0.6630839938131345423, -1.446213159395746128, -0.6155857397476032222 ) ) ;
#3805 = CARTESIAN_POINT ( 'NONE',  ( 0.4147044437876460932, -1.715472123057989684, -0.5245963139501007566 ) ) ;
#3806 = CARTESIAN_POINT ( 'NONE',  ( -0.04140212552917943434, 0.2627138686861255623, -0.3904233130033975541 ) ) ;
#3807 = CARTESIAN_POINT ( 'NONE',  ( -0.03874953289575389093, -0.4416968903498208476, -0.1785420710361537711 ) ) ;
#3808 = CARTESIAN_POINT ( 'NONE',  ( 0.01548846960707524721, 0.4638115001430989648, -0.2459753896937820483 ) ) ;
#3809 = CIRCLE ( 'NONE', #6437, 0.03000000000000029379 ) ;
#3810 = CARTESIAN_POINT ( 'NONE',  ( 0.5484444682544461491, -1.189958873811490347, 0.8086343185444866410 ) ) ;
#3811 = CARTESIAN_POINT ( 'NONE',  ( 0.04175646742902282271, -1.134690233913784096, 0.6571772246382447946 ) ) ;
#3812 = CARTESIAN_POINT ( 'NONE',  ( -0.1455608194604302852, -0.5249067277714103419, 0.1528658435937000626 ) ) ;
#3813 = CARTESIAN_POINT ( 'NONE',  ( -0.2399999999999999079, -3.609310082097819894, -0.4498340178114252352 ) ) ;
#3814 = CARTESIAN_POINT ( 'NONE',  ( 0.3135409431748647502, -1.021031066816359578, 0.7509690875494603457 ) ) ;
#3815 = DIRECTION ( 'NONE',  ( 0.4999551463232372317, -0.8660512985181134660, 0.000000000000000000 ) ) ;
#3816 = FACE_BOUND ( 'NONE', #30802, .T. ) ;
#3817 = ORIENTED_EDGE ( 'NONE', *, *, #16755, .F. ) ;
#3818 = DIRECTION ( 'NONE',  ( -1.355854680848614260E-31, 3.330669073875470114E-16, 1.000000000000000000 ) ) ;
#3819 = CARTESIAN_POINT ( 'NONE',  ( 0.5859993564695399337, -1.438286673147110450, 0.6889924778701744801 ) ) ;
#3820 = CARTESIAN_POINT ( 'NONE',  ( 0.4243666725459964151, -1.591076223527387423, -0.4156371400837810537 ) ) ;
#3821 = DIRECTION ( 'NONE',  ( 1.000000000000000000, -0.000000000000000000, -0.000000000000000000 ) ) ;
#3822 = VERTEX_POINT ( 'NONE', #24130 ) ;
#3823 = CARTESIAN_POINT ( 'NONE',  ( -0.1613941814439339706, 0.5013693833954219192, 0.3301047373962494036 ) ) ;
#3824 =( BOUNDED_SURFACE ( )  B_SPLINE_SURFACE ( 3, 2, ( 
 ( #891, #12792, #34785 ),
 ( #6588, #31711, #16092 ),
 ( #28635, #506, #9896 ),
 ( #6803, #19383, #31919 ),
 ( #16895, #11532, #38881 ),
 ( #29437, #13993, #14203 ),
 ( #13786, #1877, #19979 ),
 ( #32715, #8016, #11317 ),
 ( #36204, #26354, #17683 ),
 ( #20592, #23888, #14596 ),
 ( #1475, #14390, #1685 ),
 ( #24097, #20804, #36008 ),
 ( #4333, #23677, #26770 ),
 ( #26566, #7814, #10714 ),
 ( #36416, #4720, #23286 ),
 ( #39102, #7622, #10926 ),
 ( #23492, #20385, #32912 ),
 ( #36624, #32511, #8228 ) ),
 .UNSPECIFIED., .F., .F., .T. ) 
 B_SPLINE_SURFACE_WITH_KNOTS ( ( 4, 2, 2, 2, 2, 2, 2, 2, 4 ),
 ( 3, 3 ),
 ( 5.421010862427522170E-20, 0.0008416854974228110600, 0.001683370994845622120, 0.002525056492268432963, 0.003366741989691244240, 0.005050112984536865926, 0.005470955733248271564, 0.005891798481959677203, 0.006733483979382488480 ),
 ( 0.000000000000000000, 1.000000000000000000 ),
 .UNSPECIFIED. ) 
 GEOMETRIC_REPRESENTATION_ITEM ( )  RATIONAL_B_SPLINE_SURFACE ( (
 ( 1.000000000000000000, 0.9337218516597644014, 1.000000000000000000),
 ( 1.000000000000000000, 0.9180632194023589099, 1.000000000000000000),
 ( 1.000000000000000000, 0.9017816102666014189, 1.000000000000000000),
 ( 1.000000000000000000, 0.8702833930568698584, 1.000000000000000000),
 ( 1.000000000000000000, 0.8550524697729792178, 1.000000000000000000),
 ( 1.000000000000000000, 0.8283366390151297720, 1.000000000000000000),
 ( 1.000000000000000000, 0.8166982876196974273, 1.000000000000000000),
 ( 1.000000000000000000, 0.7986721614753765630, 1.000000000000000000),
 ( 1.000000000000000000, 0.7922423667821044679, 1.000000000000000000),
 ( 1.000000000000000000, 0.7799115254237425354, 1.000000000000000000),
 ( 1.000000000000000000, 0.7807892787035727311, 1.000000000000000000),
 ( 1.000000000000000000, 0.7819697445861952811, 1.000000000000000000),
 ( 1.000000000000000000, 0.7826749973298559038, 1.000000000000000000),
 ( 1.000000000000000000, 0.7867376866317696837, 1.000000000000000000),
 ( 1.000000000000000000, 0.7898188915124169096, 1.000000000000000000),
 ( 1.000000000000000000, 0.8019006071314157547, 1.000000000000000000),
 ( 1.000000000000000000, 0.8137456928813621149, 1.000000000000000000),
 ( 1.000000000000000000, 0.8282401589944672349, 1.000000000000000000) ) ) 
 REPRESENTATION_ITEM ( '' )  SURFACE ( )  );
#3825 = CARTESIAN_POINT ( 'NONE',  ( 0.2233893057605496613, -1.353603863650753469, 0.4173121127524894169 ) ) ;
#3826 = DIRECTION ( 'NONE',  ( 4.930380657631316120E-32, -0.4685245517976818208, -0.8834504764630450868 ) ) ;
#3827 = CARTESIAN_POINT ( 'NONE',  ( 0.1333333333333120430, -2.107936428766273629, -0.7005084057759864979 ) ) ;
#3828 = CARTESIAN_POINT ( 'NONE',  ( 0.4269689327050869565, -1.183341550326573177, 0.7120333345843747885 ) ) ;
#3830 = CARTESIAN_POINT ( 'NONE',  ( 0.3219857165489931061, -1.758039968903889250, 0.4848815471996625326 ) ) ;
#3829 = CARTESIAN_POINT ( 'NONE',  ( -0.2399999999999999079, -2.050023788963422078, -0.4737205214156571809 ) ) ;
#3831 = CARTESIAN_POINT ( 'NONE',  ( 0.1856290495283919040, -0.8698730627085041744, 0.1722928722954065184 ) ) ;
#3832 = ORIENTED_EDGE ( 'NONE', *, *, #6625, .T. ) ;
#3833 = CARTESIAN_POINT ( 'NONE',  ( 0.01482441653333900489, -0.9260584756313956500, 0.5696548266057109844 ) ) ;
#3834 = ORIENTED_EDGE ( 'NONE', *, *, #9692, .T. ) ;
#3835 = CARTESIAN_POINT ( 'NONE',  ( 0.3872640377415917934, -1.605414403979557925, 0.6082151896501704069 ) ) ;
#3837 = CARTESIAN_POINT ( 'NONE',  ( 0.1843176191431192545, -0.8530889732836612893, 0.1272869310077573146 ) ) ;
#3836 = CARTESIAN_POINT ( 'NONE',  ( 0.08543706580305507337, -0.8249828158407566114, 0.1015297857590274355 ) ) ;
#3838 = DIRECTION ( 'NONE',  ( 1.000000000000000000, 6.779273404243070203E-32, 4.314083075427408311E-32 ) ) ;
#3839 = ORIENTED_EDGE ( 'NONE', *, *, #13267, .F. ) ;
#3840 = ORIENTED_EDGE ( 'NONE', *, *, #6884, .T. ) ;
#3841 = ORIENTED_EDGE ( 'NONE', *, *, #38081, .F. ) ;
#3842 = CARTESIAN_POINT ( 'NONE',  ( 0.5384555088268765388, -1.160728211852388947, 0.5797400768281307792 ) ) ;
#3843 = ADVANCED_FACE ( 'NONE', ( #36651 ), #28609, .T. ) ;
#3844 = CARTESIAN_POINT ( 'NONE',  ( 0.5668525377163954326, -1.503218863262137939, 0.5717302897758860247 ) ) ;
#3845 = ORIENTED_EDGE ( 'NONE', *, *, #30859, .F. ) ;
#3846 = CARTESIAN_POINT ( 'NONE',  ( 0.3926032618789407347, -1.756026311479913948, -0.5284552501753293496 ) ) ;
#3847 = CARTESIAN_POINT ( 'NONE',  ( -0.2399999999999999079, -2.292669950144801572, -0.8383185228372386222 ) ) ;
#3848 = EDGE_CURVE ( 'NONE', #24392, #11781, #14140, .T. ) ;
#3849 = CARTESIAN_POINT ( 'NONE',  ( 0.6089166525218913106, -1.414157958342789234, -0.6250000000000001110 ) ) ;
#3850 = CARTESIAN_POINT ( 'NONE',  ( 0.4567198261210261845, -1.219045092035883293, 0.5856983068965102568 ) ) ;
#3851 = ORIENTED_EDGE ( 'NONE', *, *, #10449, .F. ) ;
#3852 = PRODUCT ( 'pulley subassembly', 'pulley subassembly', '', ( #21598 ) ) ;
#3853 = CARTESIAN_POINT ( 'NONE',  ( -0.8248651029816859159, -5.463695987328526437E-16, 0.000000000000000000 ) ) ;
#3854 = EDGE_CURVE ( 'NONE', #26513, #11533, #2353, .T. ) ;
#3855 = CARTESIAN_POINT ( 'NONE',  ( 0.2117601568378603694, -1.293150266309827101, -0.2869361388274795921 ) ) ;
#3856 = CARTESIAN_POINT ( 'NONE',  ( 0.3885621086388810763, -1.758569517285561767, -0.5425237269221726555 ) ) ;
#3857 = ADVANCED_FACE ( 'NONE', ( #28766 ), #13460, .F. ) ;
#3858 = DIRECTION ( 'NONE',  ( 0.8660512985181132439, 0.4999551463232376758, 0.000000000000000000 ) ) ;
#3859 = CARTESIAN_POINT ( 'NONE',  ( 0.07115259279998498165, -1.324306246913844021, 0.5002830441458163691 ) ) ;
#3860 = CARTESIAN_POINT ( 'NONE',  ( 0.3186320389496528627, -1.760431904683431359, 0.5682417262808792113 ) ) ;
#3861 = CARTESIAN_POINT ( 'NONE',  ( -0.2399999999999999079, -1.990692974992658737, -0.4647843861454829528 ) ) ;
#3862 = APPROVAL_STATUS ( 'not_yet_approved' ) ;
#3863 = DIRECTION ( 'NONE',  ( 0.9931241558664195557, 5.463695987328507662E-14, -0.1170658405966981674 ) ) ;
#3864 = DIRECTION ( 'NONE',  ( 0.000000000000000000, -0.9510565162951467588, -0.3090169943749687675 ) ) ;
#3865 = CARTESIAN_POINT ( 'NONE',  ( 0.1845357796896161806, -0.8398727082387180687, 0.07607969940124001407 ) ) ;
#3866 = FACE_OUTER_BOUND ( 'NONE', #18501, .T. ) ;
#3867 = DIRECTION ( 'NONE',  ( 1.000000000000000000, 2.341930812374887555E-31, -1.664003471950578127E-31 ) ) ;
#3868 = EDGE_CURVE ( 'NONE', #25706, #19455, #27960, .T. ) ;
#3869 = APPLIED_PERSON_AND_ORGANIZATION_ASSIGNMENT ( #2159, #38814, ( #33451 ) ) ;
#3870 = CARTESIAN_POINT ( 'NONE',  ( 0.2491647336858476003, -1.658092311124387708, 0.5917354811442696594 ) ) ;
#3871 = CARTESIAN_POINT ( 'NONE',  ( -0.0001404195193253628224, -0.8121462962669929730, -0.07004528601953871614 ) ) ;
#3872 = CARTESIAN_POINT ( 'NONE',  ( -2.134462193483032131E-14, -2.087756091470926112, -0.2623975632731759267 ) ) ;
#3873 = CARTESIAN_POINT ( 'NONE',  ( 0.05283102792148707677, -0.2421768296208668403, 0.4008516595826059903 ) ) ;
#3874 = LINE ( 'NONE', #12953, #38200 ) ;
#3875 = ORIENTED_EDGE ( 'NONE', *, *, #8921, .F. ) ;
#3876 = ORIENTED_EDGE ( 'NONE', *, *, #5114, .F. ) ;
#3877 = CARTESIAN_POINT ( 'NONE',  ( 0.05083665881508966922, -0.2375940621857673685, -0.4096919151850476060 ) ) ;
#3878 = VERTEX_POINT ( 'NONE', #37820 ) ;
#3879 = CARTESIAN_POINT ( 'NONE',  ( 0.1399999999999994582, 0.000000000000000000, 0.000000000000000000 ) ) ;
#3880 = DIRECTION ( 'NONE',  ( -0.8660512985181132439, -0.4999551463232375648, 0.000000000000000000 ) ) ;
#3881 = CARTESIAN_POINT ( 'NONE',  ( 0.4655342829600510046, -1.243759628728527966, 0.7615958905844258942 ) ) ;
#3883 = EDGE_LOOP ( 'NONE', ( #34607, #18105, #4572, #21562, #35821, #1572 ) ) ;
#3882 = LINE ( 'NONE', #1055, #23921 ) ;
#3884 = CARTESIAN_POINT ( 'NONE',  ( 0.2882448896600493526, -0.8342145444298804113, 0.5948296420995525802 ) ) ;
#3885 = EDGE_CURVE ( 'NONE', #17043, #33631, #16018, .T. ) ;
#3886 = ORIENTED_EDGE ( 'NONE', *, *, #27831, .F. ) ;
#3887 = CARTESIAN_POINT ( 'NONE',  ( 0.5953197980378833742, -1.599064723402610300, 0.4311035055375501135 ) ) ;
#3888 = EDGE_LOOP ( 'NONE', ( #39830, #32213, #34349, #27878 ) ) ;
#3889 = CARTESIAN_POINT ( 'NONE',  ( 0.01207517534499727083, -0.5592029808840295324, 0.2697748480126794801 ) ) ;
#3891 = CARTESIAN_POINT ( 'NONE',  ( -0.02869712619511926438, -0.2420104654861697513, 0.4357576342647261347 ) ) ;
#3890 = CARTESIAN_POINT ( 'NONE',  ( -0.02000000000000000042, -1.910390638264138685, -0.7420407338378623985 ) ) ;
#3892 = DIRECTION ( 'NONE',  ( 2.157041537713702240E-32, -0.8709776783778059306, 0.4913225862583635584 ) ) ;
#3893 = CARTESIAN_POINT ( 'NONE',  ( 0.01204206997202984797, -0.4674074136848835326, 0.008773000355436783720 ) ) ;
#3894 = CARTESIAN_POINT ( 'NONE',  ( 0.04964375069992935791, -1.483475046233223571, -0.3718814836353687703 ) ) ;
#3896 = ORIENTED_EDGE ( 'NONE', *, *, #32123, .T. ) ;
#3895 = ORIENTED_EDGE ( 'NONE', *, *, #28545, .T. ) ;
#3897 = CARTESIAN_POINT ( 'NONE',  ( -0.3000000000000000999, -3.753843787845913216, -0.2458487048530572372 ) ) ;
#3898 = CARTESIAN_POINT ( 'NONE',  ( 0.2516264960652024874, -0.9499261728892368639, 0.4858447589484862217 ) ) ;
#3899 = CARTESIAN_POINT ( 'NONE',  ( -0.03159140494780136865, 0.05458666898339525897, -0.4890560705835249600 ) ) ;
#3900 = EDGE_CURVE ( 'NONE', #33422, #25941, #20741, .T. ) ;
#3901 = CARTESIAN_POINT ( 'NONE',  ( -2.112273405726188513E-14, -2.107936428766274073, -0.2870436526301869962 ) ) ;
#3902 = CARTESIAN_POINT ( 'NONE',  ( 0.3705277829417951141, -1.241127117052787554, 0.6578903985100409413 ) ) ;
#3903 = DIRECTION ( 'NONE',  ( -1.000000000000000000, -0.000000000000000000, -0.000000000000000000 ) ) ;
#3904 = EDGE_CURVE ( 'NONE', #3966, #13311, #39109, .T. ) ;
#3905 = CARTESIAN_POINT ( 'NONE',  ( 0.4716011037672954709, -1.161152322290847971, 0.4182417262808811320 ) ) ;
#3906 = EDGE_CURVE ( 'NONE', #7093, #17060, #2142, .T. ) ;
#3907 = CARTESIAN_POINT ( 'NONE',  ( -0.1656893171628588957, 0.4813634391809756830, 0.3338433979332086632 ) ) ;
#3908 = DIRECTION ( 'NONE',  ( 7.771561172376107616E-16, -7.170354002788761615E-17, 1.000000000000000000 ) ) ;
#3909 = DIRECTION ( 'NONE',  ( 0.8660512985181135770, 0.4999551463232372317, 0.000000000000000000 ) ) ;
#3910 = CARTESIAN_POINT ( 'NONE',  ( -0.02000000000000000042, -1.699711333021935777, -0.9366211149475224262 ) ) ;
#3911 = DATE_AND_TIME ( #10913, #12163 ) ;
#3912 = FACE_OUTER_BOUND ( 'NONE', #31874, .T. ) ;
#3913 = CARTESIAN_POINT ( 'NONE',  ( 0.1797611301157409636, -0.4952674041179104814, 0.1258321121258487441 ) ) ;
#3914 = CARTESIAN_POINT ( 'NONE',  ( 0.1988232060422361613, -2.043630805496089220, -0.6812398176055290966 ) ) ;
#3915 = ADVANCED_FACE ( 'NONE', ( #35140 ), #7326, .T. ) ;
#3916 = CARTESIAN_POINT ( 'NONE',  ( 0.4394396372989468613, -1.699335966064649206, 0.4346836767675715252 ) ) ;
#3917 = CARTESIAN_POINT ( 'NONE',  ( 0.2571002409661083954, -1.568717443816634693, -0.6786148624936777507 ) ) ;
#3918 = CARTESIAN_POINT ( 'NONE',  ( -0.03301162916268465808, 0.5156255563253698826, 0.07469829950279255337 ) ) ;
#3919 = DIRECTION ( 'NONE',  ( 0.000000000000000000, 0.7071067811865475727, -0.7071067811865475727 ) ) ;
#3920 = DIRECTION ( 'NONE',  ( -1.000000000000000000, -0.000000000000000000, -0.000000000000000000 ) ) ;
#3921 = ORIENTED_EDGE ( 'NONE', *, *, #5958, .T. ) ;
#3922 = CARTESIAN_POINT ( 'NONE',  ( 0.1048591973540500683, -1.410537849644770025, 0.5682417262808777680 ) ) ;
#3923 = CARTESIAN_POINT ( 'NONE',  ( 0.2629078703310521736, -1.686706023028639478, 0.5455699756094425368 ) ) ;
#3924 = CARTESIAN_POINT ( 'NONE',  ( 0.1314486695871137090, -0.5541963170049430953, 0.1786156050719973354 ) ) ;
#3926 = ORIENTED_EDGE ( 'NONE', *, *, #14495, .F. ) ;
#3925 = CARTESIAN_POINT ( 'NONE',  ( 0.5536297569049346556, -1.186194075236972179, 0.6057417262809815517 ) ) ;
#3928 = ORIENTED_EDGE ( 'NONE', *, *, #28813, .T. ) ;
#3927 = ORIENTED_EDGE ( 'NONE', *, *, #16488, .T. ) ;
#3929 = PERSON ( 'NAUO-PER11', 'UNSPECIFIED', 'UNSPECIFIED', ('UNSPECIFIED'), ('UNSPECIFIED'), ('UNSPECIFIED') ) ;
#3930 = CARTESIAN_POINT ( 'NONE',  ( 0.6296519982359254364, -1.458631199707426385, 0.8241730067046653119 ) ) ;
#3931 = VERTEX_POINT ( 'NONE', #6942 ) ;
#3932 = CARTESIAN_POINT ( 'NONE',  ( -0.2746410161513770931, -2.853330612949663170, -0.6088139570729240724 ) ) ;
#3933 = CARTESIAN_POINT ( 'NONE',  ( -0.1667768525404892954, 0.4849111360356626044, 0.1246604372685282680 ) ) ;
#3934 = CALENDAR_DATE ( 2026, 13, 10 ) ;
#3935 = CARTESIAN_POINT ( 'NONE',  ( -0.002922341574000678326, -0.8469330747986107966, 0.04185307883324775047 ) ) ;
#3936 = EDGE_LOOP ( 'NONE', ( #6314, #18562, #36072, #36695, #22075, #6715, #6407 ) ) ;
#3937 = CARTESIAN_POINT ( 'NONE',  ( 0.1157690968366767853, -0.8206980902245742948, 0.4173617279069409824 ) ) ;
#3938 = EDGE_CURVE ( 'NONE', #13059, #29074, #36012, .T. ) ;
#3939 = FACE_OUTER_BOUND ( 'NONE', #26306, .T. ) ;
#3940 = CARTESIAN_POINT ( 'NONE',  ( 0.1903510223940173829, -0.8354967341176428031, 0.6604265076868101048 ) ) ;
#3941 = ORIENTED_EDGE ( 'NONE', *, *, #4230, .T. ) ;
#3942 = CARTESIAN_POINT ( 'NONE',  ( 0.6441828724856649702, -1.607382658460039471, -0.5688074945424951290 ) ) ;
#3943 = CARTESIAN_POINT ( 'NONE',  ( -0.05464101615137787610, -2.551729310907437043, -0.5086726180052709712 ) ) ;
#3944 = CARTESIAN_POINT ( 'NONE',  ( -0.04293324258486928141, 0.07181764475133092795, 0.4893676133895074054 ) ) ;
#3945 = ADVANCED_FACE ( 'NONE', ( #4050 ), #25775, .F. ) ;
#3946 = CIRCLE ( 'NONE', #32192, 0.05330708661417321581 ) ;
#3947 = CARTESIAN_POINT ( 'NONE',  ( 0.4191100986681001173, -1.701672718972385701, 0.4233639548768205474 ) ) ;
#3948 = CARTESIAN_POINT ( 'NONE',  ( 0.3475958263379387292, -1.626714668491045401, -0.3321210449665553122 ) ) ;
#3949 = CIRCLE ( 'NONE', #12502, 1.991674066779354213 ) ;
#3950 = DIRECTION ( 'NONE',  ( -1.000000000000000000, -2.276539994720197063E-15, 0.000000000000000000 ) ) ;
#3951 = AXIS2_PLACEMENT_3D ( 'NONE', #7811, #20381, #29840 ) ;
#3952 = CARTESIAN_POINT ( 'NONE',  ( 0.6090209075241541647, -1.479030249925110008, 0.5727419068642127797 ) ) ;
#3953 = CARTESIAN_POINT ( 'NONE',  ( -6.803815825995611946E-06, -0.7962170029740717192, -0.09155518444196047989 ) ) ;
#3954 =( NAMED_UNIT ( * ) SI_UNIT ( $, .STERADIAN. ) SOLID_ANGLE_UNIT ( ) );
#3955 = CARTESIAN_POINT ( 'NONE',  ( 0.6620678144876760429, -1.446799780631947252, -0.4151272395384200675 ) ) ;
#3956 = CARTESIAN_POINT ( 'NONE',  ( 0.01548846960703782229, 0.2306506793134120714, 0.4716198300880287131 ) ) ;
#3957 = CARTESIAN_POINT ( 'NONE',  ( 0.05796715499547382133, -1.320156192035571774, 0.6033327867956804758 ) ) ;
#3958 = CARTESIAN_POINT ( 'NONE',  ( 0.5099336548069899333, -1.112575729146672243, 0.5993070616419141627 ) ) ;
#3959 = PERSON_AND_ORGANIZATION_ROLE ( 'design_supplier' ) ;
#3960 = EDGE_CURVE ( 'NONE', #13108, #36780, #1692, .T. ) ;
#3961 = FACE_OUTER_BOUND ( 'NONE', #6511, .T. ) ;
#3962 = ADVANCED_FACE ( 'NONE', ( #29564 ), #2996, .T. ) ;
#3963 = EDGE_CURVE ( 'NONE', #20650, #11991, #13924, .T. ) ;
#3964 = CARTESIAN_POINT ( 'NONE',  ( -0.2399999999999999079, -2.183180860297908144, -0.4937760292030871079 ) ) ;
#3965 = CARTESIAN_POINT ( 'NONE',  ( 0.3164584772848521577, -1.761781577301324786, 0.5677477157759467374 ) ) ;
#3966 = VERTEX_POINT ( 'NONE', #1406 ) ;
#3967 = DIRECTION ( 'NONE',  ( 0.000000000000000000, -0.9246857012436752177, 0.3807313408632029827 ) ) ;
#3968 = CARTESIAN_POINT ( 'NONE',  ( 0.002296835029421141847, -0.5198933010532248433, 0.1369805761320314896 ) ) ;
#3969 = AXIS2_PLACEMENT_3D ( 'NONE', #22525, #6862, #31974 ) ;
#3970 = CARTESIAN_POINT ( 'NONE',  ( 0.08659183687672357410, -0.7486551410394269856, 0.03870967331810245410 ) ) ;
#3971 = ORIENTED_EDGE ( 'NONE', *, *, #13695, .F. ) ;
#3972 = CARTESIAN_POINT ( 'NONE',  ( 0.4972671625857253974, -1.080199071502573771, 0.5707417262808780478 ) ) ;
#3973 = CARTESIAN_POINT ( 'NONE',  ( 0.1927903040881008279, -0.5292341811144671837, 0.2767179517167643321 ) ) ;
#3975 = ORIENTED_EDGE ( 'NONE', *, *, #32047, .F. ) ;
#3974 = ORIENTED_EDGE ( 'NONE', *, *, #3223, .T. ) ;
#3976 = PLANE ( 'NONE',  #26437 ) ;
#3977 = AXIS2_PLACEMENT_3D ( 'NONE', #26958, #8622, #39911 ) ;
#3978 = ORIENTED_EDGE ( 'NONE', *, *, #39551, .F. ) ;
#3979 = CARTESIAN_POINT ( 'NONE',  ( 0.3560871317620682985, -1.891711383486874620, -0.4908775415153238120 ) ) ;
#3980 = DIRECTION ( 'NONE',  ( -1.000000000000000000, -2.341930812374887555E-31, 1.664003471950578127E-31 ) ) ;
#3981 = CIRCLE ( 'NONE', #25018, 0.03000000000000002318 ) ;
#3982 = DIRECTION ( 'NONE',  ( 0.8660512985181134660, 0.4999551463232372317, 0.000000000000000000 ) ) ;
#3983 = ORIENTED_EDGE ( 'NONE', *, *, #20029, .F. ) ;
#3984 = CARTESIAN_POINT ( 'NONE',  ( 0.3022532383517997912, -1.314739514998899850, 1.137766315222363822 ) ) ;
#3985 = CARTESIAN_POINT ( 'NONE',  ( 0.09335318867712337487, -0.5801916173533016030, 0.2651423415210660273 ) ) ;
#3986 = CARTESIAN_POINT ( 'NONE',  ( 0.03472485495275277889, -0.6070042031976854435, 0.5858001736030246098 ) ) ;
#3987 = CARTESIAN_POINT ( 'NONE',  ( 0.08585723802341010957, -0.5540659370326329602, 0.2123023186766486992 ) ) ;
#3989 = CARTESIAN_POINT ( 'NONE',  ( 0.3699448142092459091, -1.724996014291202195, 0.4246285625532579822 ) ) ;
#3988 = CARTESIAN_POINT ( 'NONE',  ( 0.4912428832138920343, -1.588451637922100312, -0.4575737628907398657 ) ) ;
#3990 = CARTESIAN_POINT ( 'NONE',  ( 0.1406250000000002220, -0.9233928627580063608, 0.1613420322700153120 ) ) ;
#3991 = ORIENTED_EDGE ( 'NONE', *, *, #24482, .F. ) ;
#3992 = VERTEX_POINT ( 'NONE', #35737 ) ;
#3993 = EDGE_CURVE ( 'NONE', #32724, #6555, #20123, .T. ) ;
#3994 = DIRECTION ( 'NONE',  ( 1.602373713730174099E-31, 0.9849933812515909715, 0.1725921171159281731 ) ) ;
#3995 = CARTESIAN_POINT ( 'NONE',  ( 0.2751874179112033247, -1.553387066878797240, -0.3124965672173706244 ) ) ;
#3996 = EDGE_CURVE ( 'NONE', #890, #26070, #2005, .T. ) ;
#3997 = CARTESIAN_POINT ( 'NONE',  ( -0.04047076529492919100, 0.3430644450807475709, -0.3654777640200485012 ) ) ;
#3998 = CARTESIAN_POINT ( 'NONE',  ( -0.2746410161513779258, -2.595429044015121534, -0.5484989581857646623 ) ) ;
#3999 = AXIS2_PLACEMENT_3D ( 'NONE', #8388, #7976, #24059 ) ;
#4000 = DIRECTION ( 'NONE',  ( 0.000000000000000000, -5.978086547377980964E-31, -1.000000000000000000 ) ) ;
#4001 = CARTESIAN_POINT ( 'NONE',  ( 0.6205349385892930947, -1.302967389835202772, 0.7736340727560927499 ) ) ;
#4002 = B_SPLINE_CURVE_WITH_KNOTS ( 'NONE', 3,
 ( #26798, #23520, #7225, #7436, #23317, #7839 ),
 .UNSPECIFIED., .F., .F.,
 ( 4, 2, 4 ),
 ( 0.000000000000000000, 0.0004017397477019867208, 0.0008034794954039734417 ),
 .UNSPECIFIED. ) ;
#4003 = CARTESIAN_POINT ( 'NONE',  ( 0.5369453289148307107, -1.161830891981910030, 0.5366278456428995591 ) ) ;
#4004 = CARTESIAN_POINT ( 'NONE',  ( 0.05992504362659526601, -1.332686182584564838, 0.5764222388007066433 ) ) ;
#4005 = AXIS2_PLACEMENT_3D ( 'NONE', #403, #12901, #9797 ) ;
#4006 = VECTOR ( 'NONE', #16099, 39.37007874015748854 ) ;
#4007 = CARTESIAN_POINT ( 'NONE',  ( 0.04047043078436408925, 0.4923670751789746003, -0.09403524049742247037 ) ) ;
#4008 = CARTESIAN_POINT ( 'NONE',  ( 0.5366821535715222691, -1.667685771915632165, -0.5737988098678608040 ) ) ;
#4009 = ORIENTED_EDGE ( 'NONE', *, *, #5671, .T. ) ;
#4010 = CARTESIAN_POINT ( 'NONE',  ( 0.3662562376110679030, -1.103567295189709974, 0.7374271453170119228 ) ) ;
#4011 = CARTESIAN_POINT ( 'NONE',  ( 0.05999999999999990757, 0.6730055122658872291, -0.1180550278835343775 ) ) ;
#4012 = DIRECTION ( 'NONE',  ( 1.000000000000000000, 1.445848444424219398E-15, -8.326672684688652360E-16 ) ) ;
#4013 = EDGE_LOOP ( 'NONE', ( #10496, #738, #1897, #3178 ) ) ;
#4014 = PLANE ( 'NONE',  #33177 ) ;
#4015 = CARTESIAN_POINT ( 'NONE',  ( 0.5753973661769585801, -1.420263886208666282, 0.7195733474900496418 ) ) ;
#4016 = DIRECTION ( 'NONE',  ( 1.000000000000000000, 5.586287484112844226E-16, -8.336459783983783483E-16 ) ) ;
#4017 = CARTESIAN_POINT ( 'NONE',  ( -0.05464101615137770263, -2.320036485105098301, -0.3741690811493925128 ) ) ;
#4018 = CARTESIAN_POINT ( 'NONE',  ( 0.05610887725588498132, -0.8376633732021888656, 0.2147192758300057736 ) ) ;
#4019 = ORIENTED_EDGE ( 'NONE', *, *, #6733, .T. ) ;
#4020 = CARTESIAN_POINT ( 'NONE',  ( -0.1589247078933331003, 0.4934387919091514085, 0.3384493358270195262 ) ) ;
#4021 = CARTESIAN_POINT ( 'NONE',  ( 0.3640814558764833286, -1.622621548676258518, -0.3679310410494832095 ) ) ;
#4022 = CARTESIAN_POINT ( 'NONE',  ( 0.4803259847655330095, -1.663598153568734528, 0.4773340106711829733 ) ) ;
#4023 = CARTESIAN_POINT ( 'NONE',  ( 0.1959265899308196557, -1.288818386415671036, -0.7414046965098797237 ) ) ;
#4024 = CARTESIAN_POINT ( 'NONE',  ( 0.4128242711560994871, -1.164714445187265524, 0.7168935161660692224 ) ) ;
#4025 = AXIS2_PLACEMENT_3D ( 'NONE', #39821, #37144, #36728 ) ;
#4027 = FACE_OUTER_BOUND ( 'NONE', #4029, .T. ) ;
#4026 = DIRECTION ( 'NONE',  ( 1.000000000000000000, 0.000000000000000000, 8.537024980200792236E-16 ) ) ;
#4028 = CARTESIAN_POINT ( 'NONE',  ( 0.1854168535569867549, -0.8697360073808747538, 0.1457185332388700738 ) ) ;
#4029 = EDGE_LOOP ( 'NONE', ( #8678, #29260, #25409, #23135 ) ) ;
#4030 = DATE_TIME_ROLE ( 'classification_date' ) ;
#4031 = DIRECTION ( 'NONE',  ( -1.000000000000000000, -0.000000000000000000, -0.000000000000000000 ) ) ;
#4032 = ORIENTED_EDGE ( 'NONE', *, *, #32113, .F. ) ;
#4033 = AXIS2_PLACEMENT_3D ( 'NONE', #25608, #38138, #35057 ) ;
#4034 = CARTESIAN_POINT ( 'NONE',  ( 0.2186375681070903965, -1.111317829052481443, 0.8545239218465585651 ) ) ;
#4036 = CARTESIAN_POINT ( 'NONE',  ( 0.2033340932986389682, -0.6878354212131936318, 0.3466422550156073035 ) ) ;
#4035 = CARTESIAN_POINT ( 'NONE',  ( 0.08727560228832158262, -0.7066680270200008662, 0.002681738102100845057 ) ) ;
#4037 = LINE ( 'NONE', #32427, #11255 ) ;
#4038 = ORIENTED_EDGE ( 'NONE', *, *, #2504, .T. ) ;
#4039 = CONICAL_SURFACE ( 'NONE', #24440, 0.1600000000000018352, 1.047197551196601850 ) ;
#4040 = ORIENTED_EDGE ( 'NONE', *, *, #28813, .F. ) ;
#4041 = DIRECTION ( 'NONE',  ( 0.8660512985181129109, 0.4999551463232380089, 0.000000000000000000 ) ) ;
#4042 = CARTESIAN_POINT ( 'NONE',  ( 0.1192597013057371258, -0.5508091639576637721, 0.1706685560853501427 ) ) ;
#4043 = ORIENTED_EDGE ( 'NONE', *, *, #20338, .F. ) ;
#4044 = CARTESIAN_POINT ( 'NONE',  ( 0.1874553688902439730, -0.6895457488572201976, 0.05837238906507073027 ) ) ;
#4045 = CARTESIAN_POINT ( 'NONE',  ( 0.1399999999999994582, -1.330566893520349807E-17, -0.04999999999999998890 ) ) ;
#4046 = CARTESIAN_POINT ( 'NONE',  ( 0.5959315179729322010, -1.587052097778462789, 0.4182417262808776903 ) ) ;
#4047 = CARTESIAN_POINT ( 'NONE',  ( 1.989330125873876791E-16, 0.2981948553318908290, -0.06819284191469622558 ) ) ;
#4048 = DIRECTION ( 'NONE',  ( -4.930380657631319405E-32, 0.5237184928541299689, -0.8518913899333637740 ) ) ;
#4049 = B_SPLINE_CURVE_WITH_KNOTS ( 'NONE', 3,
 ( #2588, #15341, #27080, #12262 ),
 .UNSPECIFIED., .F., .F.,
 ( 4, 4 ),
 ( 2.201117333616983429E-17, 0.0002394164967011357874 ),
 .UNSPECIFIED. ) ;
#4050 = FACE_OUTER_BOUND ( 'NONE', #3692, .T. ) ;
#4051 = CARTESIAN_POINT ( 'NONE',  ( 0.7429241260303105499, -1.515741207197444762, 0.5682417262808782121 ) ) ;
#4052 = CARTESIAN_POINT ( 'NONE',  ( 0.3931437146781530667, -1.977407099708731408, -0.4983079568841896623 ) ) ;
#4053 = CARTESIAN_POINT ( 'NONE',  ( 0.06581764578086118922, -1.340728352476674212, 0.5449258910593480776 ) ) ;
#4054 = CARTESIAN_POINT ( 'NONE',  ( 0.1166065821415038645, -1.415338206367126039, 0.5682417262808805436 ) ) ;
#4055 = PRODUCT_CONTEXT ( 'NONE', #3232, 'mechanical' ) ;
#4056 = AXIS2_PLACEMENT_3D ( 'NONE', #23864, #39888, #24262 ) ;
#4057 = CARTESIAN_POINT ( 'NONE',  ( 0.6414788747720358009, -1.458704226864308451, -0.6334847565629259103 ) ) ;
#4058 = CARTESIAN_POINT ( 'NONE',  ( 0.2317652421976991728, -1.348504658504371179, 0.5084384545799764954 ) ) ;
#4059 = CARTESIAN_POINT ( 'NONE',  ( -0.1210148435730253463, -0.5061394519557904648, 0.3122829191279373751 ) ) ;
#4060 = CARTESIAN_POINT ( 'NONE',  ( 0.1499999999999994671, 0.4770632572900446178, -0.2530032579707474083 ) ) ;
#4061 = CARTESIAN_POINT ( 'NONE',  ( 0.3812071769896587803, -1.763750790280042002, -0.4536492913031247021 ) ) ;
#4062 = CIRCLE ( 'NONE', #27074, 0.9087847906030154244 ) ;
#4063 =( BOUNDED_SURFACE ( )  B_SPLINE_SURFACE ( 3, 2, ( 
 ( #3691, #25699, #35165 ),
 ( #6966, #20342, #17645 ),
 ( #10880, #26512, #29793 ),
 ( #13740, #4480, #16853 ),
 ( #20146, #1429, #17452 ),
 ( #38639, #14350, #36359 ) ),
 .UNSPECIFIED., .F., .F., .T. ) 
 B_SPLINE_SURFACE_WITH_KNOTS ( ( 4, 2, 4 ),
 ( 3, 3 ),
 ( 0.000000000000000000, 0.0003830006634344629507, 0.0007660013268689259015 ),
 ( 0.000000000000000000, 1.000000000000000000 ),
 .UNSPECIFIED. ) 
 GEOMETRIC_REPRESENTATION_ITEM ( )  RATIONAL_B_SPLINE_SURFACE ( (
 ( 1.000000000000000000, 0.9000550641259897899, 1.000000000000000000),
 ( 1.000000000000000000, 0.9180209094310995965, 1.000000000000000000),
 ( 1.000000000000000000, 0.9393933891286406768, 1.000000000000000000),
 ( 1.000000000000000000, 0.9796198219468460477, 1.000000000000000000),
 ( 1.000000000000000000, 0.9990870677679748457, 1.000000000000000000),
 ( 1.000000000000000000, 1.000000000000000000, 1.000000000000000000) ) ) 
 REPRESENTATION_ITEM ( '' )  SURFACE ( )  );
#4064 = AXIS2_PLACEMENT_3D ( 'NONE', #70, #12563, #18957 ) ;
#4065 = CARTESIAN_POINT ( 'NONE',  ( 0.003124719664520401140, -0.5686731593868927792, 0.1286173008190011902 ) ) ;
#4066 = CARTESIAN_POINT ( 'NONE',  ( 0.0002050826195777198982, -0.5232135321910946768, -0.04216937712956515816 ) ) ;
#4067 = CONICAL_SURFACE ( 'NONE', #38259, 0.1600000000000006140, 1.047197551196598075 ) ;
#4068 = DIRECTION ( 'NONE',  ( -7.000205099780314469E-17, -1.000000000000000000, 6.590151126658399604E-16 ) ) ;
#4069 = CARTESIAN_POINT ( 'NONE',  ( 0.3245308759113119113, -1.295391163961464365, 0.5682442948123348492 ) ) ;
#4070 = LINE ( 'NONE', #14150, #19062 ) ;
#4071 = ORIENTED_EDGE ( 'NONE', *, *, #29129, .T. ) ;
#4072 = EDGE_LOOP ( 'NONE', ( #6658, #16104, #5131, #30998 ) ) ;
#4073 = ORIENTED_EDGE ( 'NONE', *, *, #16326, .T. ) ;
#4074 = DIRECTION ( 'NONE',  ( -1.000000000000000000, -2.280301054154495132E-31, 1.664003471950577689E-31 ) ) ;
#4075 = DIRECTION ( 'NONE',  ( 1.000000000000000000, -0.000000000000000000, -0.000000000000000000 ) ) ;
#4076 = CARTESIAN_POINT ( 'NONE',  ( 0.4114930829410045621, -1.163324819952073153, 0.7935316178056401881 ) ) ;
#4078 = VERTEX_POINT ( 'NONE', #33051 ) ;
#4077 = CARTESIAN_POINT ( 'NONE',  ( 1.024442997624098658E-15, -0.3059742766594579222, -1.570812596356951301E-15 ) ) ;
#4079 = CARTESIAN_POINT ( 'NONE',  ( 0.5539006188405288800, -1.190957016459229800, 0.5326915342634773731 ) ) ;
#4080 = CARTESIAN_POINT ( 'NONE',  ( 0.3402959632056912764, -1.632552626064601053, -0.5940485371126206227 ) ) ;
#4081 = VERTEX_POINT ( 'NONE', #10857 ) ;
#4082 = CARTESIAN_POINT ( 'NONE',  ( 0.5980161951564891831, -1.483775577296369219, -0.6139673809116643621 ) ) ;
#4083 = VERTEX_POINT ( 'NONE', #32653 ) ;
#4084 = CARTESIAN_POINT ( 'NONE',  ( 0.2735842598402163928, -1.463806052640699074, 0.8970317457453208521 ) ) ;
#4086 = CARTESIAN_POINT ( 'NONE',  ( -0.02869942827333585647, -0.4892109928530954388, 0.09550568247005927769 ) ) ;
#4085 = CARTESIAN_POINT ( 'NONE',  ( 0.5998866944813460167, -1.596483326503711719, 0.4395608873836979180 ) ) ;
#4087 = CARTESIAN_POINT ( 'NONE',  ( 0.3048982267989291395, -1.756746414302343240, 0.5594309555313042859 ) ) ;
#4088 = AXIS2_PLACEMENT_3D ( 'NONE', #27597, #24520, #23706 ) ;
#4089 = CARTESIAN_POINT ( 'NONE',  ( 0.1102069964470346886, -1.338716096010474477, -0.3246197190526466936 ) ) ;
#4090 = ORIENTED_EDGE ( 'NONE', *, *, #8343, .F. ) ;
#4091 = CARTESIAN_POINT ( 'NONE',  ( -0.05464101615137785528, -2.253856486606507836, -0.7252438489935795207 ) ) ;
#4092 = CARTESIAN_POINT ( 'NONE',  ( 0.2942177235634530486, -0.9707437518647973329, 0.5507622206958932010 ) ) ;
#4093 = CARTESIAN_POINT ( 'NONE',  ( 0.4076976354719489271, -1.154888438488554270, 0.4182417262808778013 ) ) ;
#4094 = LINE ( 'NONE', #28402, #5586 ) ;
#4095 = AXIS2_PLACEMENT_3D ( 'NONE', #28568, #19317, #16233 ) ;
#4096 = CIRCLE ( 'NONE', #25796, 0.06000000000000038636 ) ;
#4097 = ADVANCED_FACE ( 'NONE', ( #38808 ), #8363, .T. ) ;
#4098 = CARTESIAN_POINT ( 'NONE',  ( 0.1475391676095154925, -0.8805552411648984723, 0.5367235207948595210 ) ) ;
#4099 = CARTESIAN_POINT ( 'NONE',  ( 0.4781934768423676818, -1.682642038360962600, -0.6151431148613257793 ) ) ;
#4100 = APPLIED_PERSON_AND_ORGANIZATION_ASSIGNMENT ( #21648, #33775, ( #6386 ) ) ;
#4101 = CIRCLE ( 'NONE', #28424, 0.1699999999999995126 ) ;
#4102 = CARTESIAN_POINT ( 'NONE',  ( 0.4929769546720680351, -1.176658441934731458, 0.4224096261816105979 ) ) ;
#4103 = CARTESIAN_POINT ( 'NONE',  ( -0.1608142870582113526, 0.4995150451154150573, 0.3323678566780322585 ) ) ;
#4104 = CARTESIAN_POINT ( 'NONE',  ( 0.6666114888622571844, -1.509927429286209044, 0.4229734475664606586 ) ) ;
#4105 = CYLINDRICAL_SURFACE ( 'NONE', #37568, 0.01499999999999999424 ) ;
#4106 = AXIS2_PLACEMENT_3D ( 'NONE', #33652, #24219, #2203 ) ;
#4107 = SPHERICAL_SURFACE ( 'NONE', #26014, 0.01499999999999999944 ) ;
#4108 = CARTESIAN_POINT ( 'NONE',  ( -0.2789010053595599725, 0.4834754829570393486, 0.09999999999999961697 ) ) ;
#4109 = CARTESIAN_POINT ( 'NONE',  ( 0.1781059945513061293, -0.4912486924221262652, 0.1372122367638805851 ) ) ;
#4110 = CARTESIAN_POINT ( 'NONE',  ( 0.1100897290998920502, -1.360766454520437874, 0.6863977214180455588 ) ) ;
#4111 = CARTESIAN_POINT ( 'NONE',  ( 0.3748597602280495655, -1.730449573624088577, 0.4273137188976714462 ) ) ;
#4112 = CARTESIAN_POINT ( 'NONE',  ( 0.3619431082889854046, -1.779064720687063783, -0.4822877365339464095 ) ) ;
#4113 = AXIS2_PLACEMENT_3D ( 'NONE', #10908, #6130, #34315 ) ;
#4114 = CARTESIAN_POINT ( 'NONE',  ( 0.3114308091870697237, -1.743858490366296810, 0.7215154734554626303 ) ) ;
#4115 = DIRECTION ( 'NONE',  ( 0.8660512985181134660, 0.4999551463232371762, 0.000000000000000000 ) ) ;
#4116 = EDGE_CURVE ( 'NONE', #39495, #24591, #14135, .T. ) ;
#4117 = EDGE_CURVE ( 'NONE', #19277, #29903, #18112, .T. ) ;
#4118 = AXIS2_PLACEMENT_3D ( 'NONE', #36614, #17674, #20582 ) ;
#4119 = AXIS2_PLACEMENT_3D ( 'NONE', #26666, #18547, #14703 ) ;
#4120 = ORIENTED_EDGE ( 'NONE', *, *, #8917, .T. ) ;
#4121 = CARTESIAN_POINT ( 'NONE',  ( 0.4800914148601737041, -1.127024615723082102, 0.4875502256570667381 ) ) ;
#4122 = ORIENTED_EDGE ( 'NONE', *, *, #25359, .F. ) ;
#4123 = FACE_OUTER_BOUND ( 'NONE', #12694, .T. ) ;
#4124 = CONICAL_SURFACE ( 'NONE', #35584, 0.1600000000000006972, 1.047197551196600074 ) ;
#4125 = EDGE_CURVE ( 'NONE', #32592, #6266, #26705, .T. ) ;
#4126 = CARTESIAN_POINT ( 'NONE',  ( 0.5832970171292772843, -1.454869700092910501, 0.7147772481381597931 ) ) ;
#4127 = ADVANCED_FACE ( 'NONE', ( #14530 ), #26098, .F. ) ;
#4130 = VERTEX_POINT ( 'NONE', #18425 ) ;
#4129 = B_SPLINE_CURVE_WITH_KNOTS ( 'NONE', 3,
 ( #32178, #3989, #10383, #22946, #35463, #32985 ),
 .UNSPECIFIED., .F., .F.,
 ( 4, 2, 4 ),
 ( 0.000000000000000000, 0.0006518578806776564958, 0.001303715761355312992 ),
 .UNSPECIFIED. ) ;
#4128 = CARTESIAN_POINT ( 'NONE',  ( 0.5605867575437351036, -1.621001144914625991, -0.5473203437262892379 ) ) ;
#4131 = ADVANCED_FACE ( 'NONE', ( #34476 ), #36744, .T. ) ;
#4133 = ORIENTED_EDGE ( 'NONE', *, *, #25582, .T. ) ;
#4132 = ORIENTED_EDGE ( 'NONE', *, *, #15204, .F. ) ;
#4134 = CARTESIAN_POINT ( 'NONE',  ( 0.5014952879285534681, -1.689753520714762924, -0.5927250296114048300 ) ) ;
#4135 = ORIENTED_EDGE ( 'NONE', *, *, #15487, .T. ) ;
#4136 = CARTESIAN_POINT ( 'NONE',  ( -0.01391884973526399255, -0.5383837722425610650, 0.2220458723941181878 ) ) ;
#4137 = CARTESIAN_POINT ( 'NONE',  ( 0.6185380437909798745, -1.622186936341058372, -0.5032892897206091565 ) ) ;
#4138 = APPROVAL_DATE_TIME ( #37691, #36670 ) ;
#4139 = CARTESIAN_POINT ( 'NONE',  ( -0.001424324173367915976, -0.4210325180397652134, -0.01138449076159632478 ) ) ;
#4140 = ORIENTED_EDGE ( 'NONE', *, *, #34287, .F. ) ;
#4141 = CARTESIAN_POINT ( 'NONE',  ( 0.08528037396856456842, -0.7892970555466644056, 0.1714812305220828614 ) ) ;
#4142 = CARTESIAN_POINT ( 'NONE',  ( 0.08991044991096724948, -0.5436620188964982336, 0.1477941536733499428 ) ) ;
#4143 = CARTESIAN_POINT ( 'NONE',  ( 0.4295717892363857815, -1.330470044908041549, 0.8374933259477883585 ) ) ;
#4144 = ORIENTED_EDGE ( 'NONE', *, *, #15033, .T. ) ;
#4145 = CARTESIAN_POINT ( 'NONE',  ( 0.1765658034078008420, -0.4883776638658609004, 0.1544953457633272131 ) ) ;
#4146 = EDGE_CURVE ( 'NONE', #12540, #19277, #12859, .T. ) ;
#4147 = CARTESIAN_POINT ( 'NONE',  ( 0.1876053338355621880, -0.6785855078148245179, 0.1477569985384105666 ) ) ;
#4148 = CARTESIAN_POINT ( 'NONE',  ( 0.7033168319441670535, -1.517879297504465264, 0.5416718245419247513 ) ) ;
#4149 = APPLIED_PERSON_AND_ORGANIZATION_ASSIGNMENT ( #30037, #30438, ( #20515 ) ) ;
#4150 = AXIS2_PLACEMENT_3D ( 'NONE', #39470, #5300, #4912 ) ;
#4151 = CARTESIAN_POINT ( 'NONE',  ( 0.3612474431891336546, -1.736522368699831231, 0.6106949725924829542 ) ) ;
#4152 = LINE ( 'NONE', #7041, #14895 ) ;
#4153 = PLANE ( 'NONE',  #31893 ) ;
#4154 = AXIS2_PLACEMENT_3D ( 'NONE', #34275, #28122, #12666 ) ;
#4155 = CARTESIAN_POINT ( 'NONE',  ( 0.08146015332400738385, -1.318321297778865864, 0.4704503523288164346 ) ) ;
#4156 = CARTESIAN_POINT ( 'NONE',  ( 0.6095253909009431537, -1.478947137852041571, 0.5845166421031070536 ) ) ;
#4157 = CIRCLE ( 'NONE', #11388, 0.1000000000000000194 ) ;
#4158 = CARTESIAN_POINT ( 'NONE',  ( -2.078131108109570059E-05, -0.9329081451665184321, 0.05729297375900673644 ) ) ;
#4159 = CARTESIAN_POINT ( 'NONE',  ( 0.2056584174081136918, -0.8821123478198787948, 0.6984915149204232732 ) ) ;
#4160 = CARTESIAN_POINT ( 'NONE',  ( 0.007872950027890082692, -0.7282374440040403352, -0.007258173132335108725 ) ) ;
#4161 = DIMENSIONAL_EXPONENTS ( 1.000000000000000000, 0.000000000000000000, 0.000000000000000000, 0.000000000000000000, 0.000000000000000000, 0.000000000000000000, 0.000000000000000000 ) ;
#4162 = CARTESIAN_POINT ( 'NONE',  ( 0.04155248107635953203, -0.4416604393009532781, -0.1616214326753676322 ) ) ;
#4163 = CARTESIAN_POINT ( 'NONE',  ( 0.04935217837593552231, -1.087446678362770758, 0.7326706496891072229 ) ) ;
#4164 = CIRCLE ( 'NONE', #21928, 0.01999999999999927530 ) ;
#4165 = CARTESIAN_POINT ( 'NONE',  ( 0.2392493758066867593, -0.9067917679836680067, 0.4646394045636887959 ) ) ;
#4166 = CALENDAR_DATE ( 2026, 13, 10 ) ;
#4167 = AXIS2_PLACEMENT_3D ( 'NONE', #9114, #5626, #18182 ) ;
#4168 = DIRECTION ( 'NONE',  ( 1.000000000000000000, 0.000000000000000000, 0.000000000000000000 ) ) ;
#4169 = CARTESIAN_POINT ( 'NONE',  ( 0.1499999999999994671, -0.5203207976467947304, -0.08861466064782093366 ) ) ;
#4170 = EDGE_CURVE ( 'NONE', #14568, #34195, #18766, .T. ) ;
#4171 = ORIENTED_EDGE ( 'NONE', *, *, #21227, .F. ) ;
#4172 = CARTESIAN_POINT ( 'NONE',  ( 0.4322324054394098281, -1.579800052727432513, 0.5947161825314808414 ) ) ;
#4173 = CARTESIAN_POINT ( 'NONE',  ( 0.002410463536293692022, -0.5295147390142669330, 0.2118009195250746268 ) ) ;
#4174 = VECTOR ( 'NONE', #29719, 39.37007874015748143 ) ;
#4175 = EDGE_CURVE ( 'NONE', #38034, #29444, #24034, .T. ) ;
#4176 = DIRECTION ( 'NONE',  ( -0.9378410757839560352, -0.1072489841977636443, 0.3300784330442384507 ) ) ;
#4177 = EDGE_LOOP ( 'NONE', ( #11866, #31462, #11042, #34917 ) ) ;
#4178 = CARTESIAN_POINT ( 'NONE',  ( 0.3424415908863561175, -1.747937484235674965, 0.4483338674950549940 ) ) ;
#4179 = ADVANCED_FACE ( 'NONE', ( #8975 ), #40028, .T. ) ;
#4180 = CARTESIAN_POINT ( 'NONE',  ( 0.1900797982425219412, -0.5100199057060679220, 0.2041009711615301980 ) ) ;
#4182 = VERTEX_POINT ( 'NONE', #27312 ) ;
#4181 = ORIENTED_EDGE ( 'NONE', *, *, #35299, .F. ) ;
#4183 = DIRECTION ( 'NONE',  ( 0.000000000000000000, 0.000000000000000000, 1.000000000000000000 ) ) ;
#4184 = AXIS2_PLACEMENT_3D ( 'NONE', #6899, #34884, #25232 ) ;
#4185 = CIRCLE ( 'NONE', #38337, 0.1500000000000009936 ) ;
#4186 = ORIENTED_EDGE ( 'NONE', *, *, #13651, .F. ) ;
#4187 = CARTESIAN_POINT ( 'NONE',  ( 0.05634304521267768928, -0.01028123094845369810, -0.4588823192046729837 ) ) ;
#4188 = CARTESIAN_POINT ( 'NONE',  ( 0.1499999999999996336, -0.2450655194479764432, 0.4674710490749318659 ) ) ;
#4189 = CARTESIAN_POINT ( 'NONE',  ( -0.04285534776242039268, 0.4878382857517714610, -0.08280911155782545718 ) ) ;
#4190 = ORIENTED_EDGE ( 'NONE', *, *, #13996, .T. ) ;
#4191 = CARTESIAN_POINT ( 'NONE',  ( 0.008753005055724370764, -0.6364574594817896669, -0.004136954017640373515 ) ) ;
#4192 = CARTESIAN_POINT ( 'NONE',  ( 0.1716834812988722314, -0.8138579001414996128, 0.5861123461217216946 ) ) ;
#4193 = AXIS2_PLACEMENT_3D ( 'NONE', #36801, #8612, #18099 ) ;
#4194 = CARTESIAN_POINT ( 'NONE',  ( 0.05060316692271353556, -0.6842963399715571438, 0.6915224596933228218 ) ) ;
#4195 = CARTESIAN_POINT ( 'NONE',  ( 0.4698952129795286314, -1.558024368996808517, 0.5758555327645124011 ) ) ;
#4196 = AXIS2_PLACEMENT_3D ( 'NONE', #13405, #34042, #21705 ) ;
#4198 = CARTESIAN_POINT ( 'NONE',  ( -0.1062892842221209583, -0.4838739999896601307, 0.3472338291022021850 ) ) ;
#4197 = CARTESIAN_POINT ( 'NONE',  ( 0.01548846960707524721, -0.4638115001430530571, -0.2459753896938768336 ) ) ;
#4199 = EDGE_CURVE ( 'NONE', #3320, #28175, #13504, .T. ) ;
#4200 = CARTESIAN_POINT ( 'NONE',  ( 0.2598333277624153004, -1.180520155007462435, 0.6285950746444651793 ) ) ;
#4201 = ORIENTED_EDGE ( 'NONE', *, *, #31153, .T. ) ;
#4202 = EDGE_CURVE ( 'NONE', #35448, #35420, #8554, .T. ) ;
#4203 = ORIENTED_EDGE ( 'NONE', *, *, #36386, .F. ) ;
#4204 = CARTESIAN_POINT ( 'NONE',  ( 0.3417996877168656411, -1.631766885285335533, 0.5547720684252442913 ) ) ;
#4205 = EDGE_CURVE ( 'NONE', #15646, #13008, #32551, .T. ) ;
#4206 = CARTESIAN_POINT ( 'NONE',  ( 0.1756091917461258811, -0.6487560037695216941, 0.5970464724471860052 ) ) ;
#4207 = CARTESIAN_POINT ( 'NONE',  ( -0.02242905165738677542, 0.2417642932583395632, -0.4517135660370341088 ) ) ;
#4208 = CARTESIAN_POINT ( 'NONE',  ( -0.05281452789367512696, -0.4561340086821544793, -0.1063737436285870225 ) ) ;
#4209 = CIRCLE ( 'NONE', #3542, 0.02999999999999997113 ) ;
#4210 = DIRECTION ( 'NONE',  ( 0.000000000000000000, 1.000000000000000000, -3.330669073875470607E-16 ) ) ;
#4211 = CARTESIAN_POINT ( 'NONE',  ( 0.3599247992643459515, -1.738746112742540095, -0.5101476835507584573 ) ) ;
#4212 = CARTESIAN_POINT ( 'NONE',  ( 0.6714320665202346827, -1.386459733509071368, 0.6790741990638067271 ) ) ;
#4213 = VECTOR ( 'NONE', #30339, 39.37007874015748143 ) ;
#4214 = AXIS2_PLACEMENT_3D ( 'NONE', #18264, #24658, #15590 ) ;
#4215 = CARTESIAN_POINT ( 'NONE',  ( -0.02000000000000000042, -2.320036485105098301, -0.2941690811493925528 ) ) ;
#4216 = DIRECTION ( 'NONE',  ( 0.000000000000000000, 0.8834504764630474183, 0.4685245517976774354 ) ) ;
#4217 = PRODUCT_DEFINITION_FORMATION_WITH_SPECIFIED_SOURCE ( 'ANY', '', #30071, .NOT_KNOWN. ) ;
#4218 = CARTESIAN_POINT ( 'NONE',  ( 0.01899496522502736040, 0.4667215747137400395, -0.2292237458735868205 ) ) ;
#4219 = CARTESIAN_POINT ( 'NONE',  ( 0.3300652619718623670, -1.292236477103671621, 0.5183498055548371175 ) ) ;
#4220 = CARTESIAN_POINT ( 'NONE',  ( 0.3469326936793421523, -1.116650062515026853, 0.7379221599654642860 ) ) ;
#4221 = DIRECTION ( 'NONE',  ( 0.4999551463232372317, -0.8660512985181135770, 0.000000000000000000 ) ) ;
#4222 = AXIS2_PLACEMENT_3D ( 'NONE', #38260, #12983, #10691 ) ;
#4223 = CARTESIAN_POINT ( 'NONE',  ( -0.04285534776242177352, -0.2295064659597282342, -0.4383723578020129463 ) ) ;
#4224 = VECTOR ( 'NONE', #25585, 39.37007874015748143 ) ;
#4225 = VERTEX_POINT ( 'NONE', #5682 ) ;
#4226 = DIRECTION ( 'NONE',  ( 0.000000000000000000, 0.3882559824134205195, -0.9215515678030121727 ) ) ;
#4227 = DIRECTION ( 'NONE',  ( 1.702140497302374535E-12, 0.000000000000000000, 1.000000000000000000 ) ) ;
#4228 = EDGE_CURVE ( 'NONE', #30976, #3992, #7943, .T. ) ;
#4229 = DIRECTION ( 'NONE',  ( -0.8660512985181132439, -0.4999551463232374537, 0.000000000000000000 ) ) ;
#4230 = EDGE_CURVE ( 'NONE', #17567, #4836, #18238, .T. ) ;
#4231 = CARTESIAN_POINT ( 'NONE',  ( 0.2733626960385290849, -1.310524412086364388, 0.6293287939193288327 ) ) ;
#4232 = EDGE_LOOP ( 'NONE', ( #29581, #27118, #25314, #28340 ) ) ;
#4233 = CARTESIAN_POINT ( 'NONE',  ( -0.1710642718812864782, 0.4986889572247779068, 0.3032895567580807250 ) ) ;
#4234 = CARTESIAN_POINT ( 'NONE',  ( -0.1399999999999997358, 1.942890293094021357E-17, 0.05000000000000000971 ) ) ;
#4235 = CARTESIAN_POINT ( 'NONE',  ( 0.1692576441742112137, -1.384930168205611656, 0.4264492190452435771 ) ) ;
#4236 = CARTESIAN_POINT ( 'NONE',  ( 0.1876026560395943066, -1.258984853855668717, -0.7446432427863726167 ) ) ;
#4237 = CIRCLE ( 'NONE', #29861, 0.01499999999999999771 ) ;
#4238 = CARTESIAN_POINT ( 'NONE',  ( 0.4874659257962786763, -1.270923258226311470, 0.6194086313868705229 ) ) ;
#4240 = CARTESIAN_POINT ( 'NONE',  ( 0.3128440348530873716, -1.762786819375506964, 0.5229383029344989442 ) ) ;
#4239 = DIRECTION ( 'NONE',  ( 0.000000000000000000, 0.000000000000000000, 1.000000000000000000 ) ) ;
#4241 = CARTESIAN_POINT ( 'NONE',  ( -0.2399999999999999079, -3.941790907013290823, -0.4709369376873030477 ) ) ;
#4242 = VERTEX_POINT ( 'NONE', #39839 ) ;
#4243 = CIRCLE ( 'NONE', #10151, 0.009999999999999913472 ) ;
#4244 = DIRECTION ( 'NONE',  ( 1.000000000000000000, 6.779273404243070203E-32, 4.314083075427408311E-32 ) ) ;
#4245 = ORIENTED_EDGE ( 'NONE', *, *, #26886, .F. ) ;
#4246 = VERTEX_POINT ( 'NONE', #11662 ) ;
#4247 = CARTESIAN_POINT ( 'NONE',  ( 0.4133098505097531628, -1.589431319560335121, 0.5690080242323289905 ) ) ;
#4249 = CARTESIAN_POINT ( 'NONE',  ( 0.1962081386259882654, -0.6973007354887533760, 0.3322094209430815903 ) ) ;
#4248 = CARTESIAN_POINT ( 'NONE',  ( 0.08559278432067010667, -0.7989444401597723955, 0.09288191320694452746 ) ) ;
#4250 = CARTESIAN_POINT ( 'NONE',  ( 0.4685502202651029569, -1.116536938686066183, 0.5688043585934901003 ) ) ;
#4251 = APPLIED_APPROVAL_ASSIGNMENT ( #40334, ( #37836 ) ) ;
#4252 = ORIENTED_EDGE ( 'NONE', *, *, #22017, .T. ) ;
#4253 = ORIENTED_EDGE ( 'NONE', *, *, #18256, .F. ) ;
#4254 = EDGE_CURVE ( 'NONE', #13571, #31015, #19263, .T. ) ;
#4255 = DIRECTION ( 'NONE',  ( 0.000000000000000000, 0.000000000000000000, -1.000000000000000000 ) ) ;
#4256 = CARTESIAN_POINT ( 'NONE',  ( 0.5732312758898047145, -1.493991244289733400, 0.6439092248849844768 ) ) ;
#4257 = ORIENTED_EDGE ( 'NONE', *, *, #7205, .F. ) ;
#4258 = CONICAL_SURFACE ( 'NONE', #27270, 0.2609684784060898322, 0.1745329251994329756 ) ;
#4259 = CARTESIAN_POINT ( 'NONE',  ( 0.1874424658970250124, -0.6905203129132115869, 0.04637705369058030269 ) ) ;
#4260 = CARTESIAN_POINT ( 'NONE',  ( 0.04285640132274102371, -0.4433417433457782497, 0.2197472875419871907 ) ) ;
#4261 = CARTESIAN_POINT ( 'NONE',  ( 0.4758899578691964116, -1.652635878263318148, -0.6322492986411032412 ) ) ;
#4262 = CARTESIAN_POINT ( 'NONE',  ( 0.4190734387097265756, -1.701429136684833976, 0.4229605459736927586 ) ) ;
#4263 = CARTESIAN_POINT ( 'NONE',  ( -2.112273405726188513E-14, -2.097675824466503691, -0.2588528740066097233 ) ) ;
#4264 = B_SPLINE_CURVE_WITH_KNOTS ( 'NONE', 3,
 ( #15756, #40459, #27708, #12283, #34484, #25447 ),
 .UNSPECIFIED., .F., .F.,
 ( 4, 2, 4 ),
 ( 9.341771812940338307E-18, 0.0005303069012029996239, 0.001060613802405989924 ),
 .UNSPECIFIED. ) ;
#4265 = CARTESIAN_POINT ( 'NONE',  ( 0.3935416462524252146, -1.752073130202867812, -0.5293634714478211434 ) ) ;
#4266 = CARTESIAN_POINT ( 'NONE',  ( -0.2399999999999999079, -2.393162167644017568, -1.003759557197344554 ) ) ;
#4267 = CARTESIAN_POINT ( 'NONE',  ( 0.6699292074404794572, -1.569526485364059143, 0.6071573546319902759 ) ) ;
#4268 = CARTESIAN_POINT ( 'NONE',  ( -0.2399999999999999079, -4.320736256378554963, -0.8145269479932405465 ) ) ;
#4269 = PERSON_AND_ORGANIZATION ( #28500, #32463 ) ;
#4270 = DIRECTION ( 'NONE',  ( 0.8660512985181127998, 0.4999551463232382309, 0.000000000000000000 ) ) ;
#4271 = AXIS2_PLACEMENT_3D ( 'NONE', #11398, #8313, #23969 ) ;
#4272 = CYLINDRICAL_SURFACE ( 'NONE', #16661, 0.01750000000000000513 ) ;
#4273 = CARTESIAN_POINT ( 'NONE',  ( 0.1847812854686134709, -0.6668630515069209341, -0.02837765232073623592 ) ) ;
#4274 = FACE_BOUND ( 'NONE', #22324, .T. ) ;
#4275 = CARTESIAN_POINT ( 'NONE',  ( 0.08146015332400816100, -1.318321297778866086, 0.4704503523288147138 ) ) ;
#4276 = AXIS2_PLACEMENT_3D ( 'NONE', #24188, #36712, #21089 ) ;
#4277 = APPLIED_APPROVAL_ASSIGNMENT ( #22974, ( #39117 ) ) ;
#4278 = CARTESIAN_POINT ( 'NONE',  ( 0.2385638199407473237, -1.468035130309864655, 0.9857930272948494110 ) ) ;
#4279 = CARTESIAN_POINT ( 'NONE',  ( 0.5872889424020651949, -1.566257061117608984, -0.4890099139335282730 ) ) ;
#4280 = CARTESIAN_POINT ( 'NONE',  ( -0.05464101615137763324, -2.183180860297908144, -0.4937760292030871079 ) ) ;
#4281 = EDGE_CURVE ( 'NONE', #15271, #5090, #8462, .T. ) ;
#4282 = CARTESIAN_POINT ( 'NONE',  ( -0.05464101615137796630, -2.183180860297908144, -0.4937760292030871079 ) ) ;
#4283 = CARTESIAN_POINT ( 'NONE',  ( -0.05076541221973634999, -0.3165406372985192784, 0.3525330185552920104 ) ) ;
#4284 = CONICAL_SURFACE ( 'NONE', #37796, 0.1400000000000008182, 1.047197551196601850 ) ;
#4285 = VERTEX_POINT ( 'NONE', #5465 ) ;
#4286 = EDGE_LOOP ( 'NONE', ( #28059, #25268, #36009 ) ) ;
#4287 = CARTESIAN_POINT ( 'NONE',  ( 0.4972320539234349468, -1.080138254241686413, 0.5197417262808780025 ) ) ;
#4288 = ORIENTED_EDGE ( 'NONE', *, *, #7001, .F. ) ;
#4289 = CYLINDRICAL_SURFACE ( 'NONE', #22418, 0.04999999999999998890 ) ;
#4290 = CARTESIAN_POINT ( 'NONE',  ( 0.5853817121637504561, -1.600135414900193620, -0.4500950668952165001 ) ) ;
#4291 = CARTESIAN_POINT ( 'NONE',  ( 0.4869258355362139912, -1.276216671384446943, 0.7509782588010058824 ) ) ;
#4293 = ORIENTED_EDGE ( 'NONE', *, *, #3230, .T. ) ;
#4292 = DIRECTION ( 'NONE',  ( -0.4999551463232372317, 0.8660512985181133550, -0.000000000000000000 ) ) ;
#4294 = CARTESIAN_POINT ( 'NONE',  ( 0.1932042024315755446, -0.7994606748157702114, 0.2910003379690608294 ) ) ;
#4295 = CARTESIAN_POINT ( 'NONE',  ( 0.1610229998878659197, -0.4681091962081970759, 0.1457315164630837434 ) ) ;
#4296 = ORIENTED_EDGE ( 'NONE', *, *, #38099, .F. ) ;
#4297 = B_SPLINE_CURVE_WITH_KNOTS ( 'NONE', 3,
 ( #32149, #16325, #13434, #35434, #7046, #19803, #31745, #16518 ),
 .UNSPECIFIED., .F., .F.,
 ( 4, 2, 2, 4 ),
 ( -7.633036733528553394E-06, 0.0006124121369014247709, 0.0009224347237189015102, 0.001232457310536378466 ),
 .UNSPECIFIED. ) ;
#4298 = DIRECTION ( 'NONE',  ( -0.5196209861461466017, 0.8543968812890798681, 0.000000000000000000 ) ) ;
#4299 = VERTEX_POINT ( 'NONE', #11851 ) ;
#4300 = CARTESIAN_POINT ( 'NONE',  ( 0.02332224506199178857, -0.5411761724791561701, 0.2067749293666701627 ) ) ;
#4302 = CARTESIAN_POINT ( 'NONE',  ( -0.03664605387828073768, -0.4430871221163693585, 0.1871485295462612941 ) ) ;
#4301 = CARTESIAN_POINT ( 'NONE',  ( 0.6263553037110800581, -1.578101984896422616, 0.4270759148754849632 ) ) ;
#4303 = CARTESIAN_POINT ( 'NONE',  ( 0.2318589737339854795, -1.232498520698479982, 0.5197417262808780025 ) ) ;
#4304 = CARTESIAN_POINT ( 'NONE',  ( 0.06643860465239320723, -1.431902482846566516, -0.3407847385126873130 ) ) ;
#4305 = VERTEX_POINT ( 'NONE', #25838 ) ;
#4306 = AXIS2_PLACEMENT_3D ( 'NONE', #3614, #31585, #22161 ) ;
#4307 = PLANE ( 'NONE',  #29003 ) ;
#4308 = CARTESIAN_POINT ( 'NONE',  ( 0.2281093225164023686, -0.8646107249477655854, 0.4403547256474249494 ) ) ;
#4309 = CARTESIAN_POINT ( 'NONE',  ( 0.1778554964483612943, -1.275556741434257679, 0.4182417262808778013 ) ) ;
#4310 = CARTESIAN_POINT ( 'NONE',  ( -0.3000000000000000999, -2.511040369707300268, -0.4948468226404901804 ) ) ;
#4311 = CARTESIAN_POINT ( 'NONE',  ( 0.3213554034218941147, -1.166633905577155739, 0.7304078056503604532 ) ) ;
#4312 = APPLIED_APPROVAL_ASSIGNMENT ( #31503, ( #29284 ) ) ;
#4313 = DIRECTION ( 'NONE',  ( 0.000000000000000000, 0.5877852522924655876, -0.8090169943749527803 ) ) ;
#4314 = CARTESIAN_POINT ( 'NONE',  ( 0.4230904536261725912, -1.143177874484793577, 0.4241467574966739096 ) ) ;
#4315 = AXIS2_PLACEMENT_3D ( 'NONE', #38812, #29378, #19908 ) ;
#4316 = CARTESIAN_POINT ( 'NONE',  ( 0.003668565761957516980, -0.8459993161072223433, 0.1457185332388710730 ) ) ;
#4317 = DIRECTION ( 'NONE',  ( 0.000000000000000000, 0.000000000000000000, -1.000000000000000000 ) ) ;
#4318 =( BOUNDED_SURFACE ( )  B_SPLINE_SURFACE ( 3, 2, ( 
 ( #18539, #14856, #40551 ),
 ( #11762, #24319, #36847 ),
 ( #5359, #30486, #8660 ),
 ( #28017, #31094, #37455 ),
 ( #21232, #9272, #21848 ),
 ( #33770, #34375, #6191 ),
 ( #18760, #31308, #3116 ),
 ( #15659, #28208, #25959 ),
 ( #874, #13168, #7005 ),
 ( #3303, #1083, #38483 ),
 ( #29226, #22064, #679 ),
 ( #22670, #19755, #38265 ),
 ( #16280, #25737, #13381 ),
 ( #25343, #19374, #32104 ),
 ( #25540, #31493, #34774 ),
 ( #10315, #31909, #37880 ),
 ( #29012, #22879, #16673 ),
 ( #9695, #38068, #10096 ) ),
 .UNSPECIFIED., .F., .F., .T. ) 
 B_SPLINE_SURFACE_WITH_KNOTS ( ( 4, 2, 2, 2, 2, 2, 2, 2, 4 ),
 ( 3, 3 ),
 ( -0.001532620576208848159, -0.0007637936630077626476, 5.033250193322864191E-06, 0.0007738601633944083760, 0.001542687076595493888, 0.002311513989796579183, 0.003080340902997664911, 0.003849167816198750640, 0.004617994729399835935 ),
 ( 0.000000000000000000, 1.000000000000000000 ),
 .UNSPECIFIED. ) 
 GEOMETRIC_REPRESENTATION_ITEM ( )  RATIONAL_B_SPLINE_SURFACE ( (
 ( 1.000000000000000000, 0.7283825911960447597, 1.000000000000000000),
 ( 1.000000000000000000, 0.7404385082112692196, 1.000000000000000000),
 ( 1.000000000000000000, 0.7521504257740204702, 1.000000000000000000),
 ( 1.000000000000000000, 0.7744497410759664247, 1.000000000000000000),
 ( 1.000000000000000000, 0.7845654757374723731, 1.000000000000000000),
 ( 1.000000000000000000, 0.8022083990891452077, 1.000000000000000000),
 ( 1.000000000000000000, 0.8094167424699479918, 1.000000000000000000),
 ( 1.000000000000000000, 0.8194491993616462855, 1.000000000000000000),
 ( 1.000000000000000000, 0.8220634900780513510, 1.000000000000000000),
 ( 1.000000000000000000, 0.8220705070823443039, 1.000000000000000000),
 ( 1.000000000000000000, 0.8194468812479829278, 1.000000000000000000),
 ( 1.000000000000000000, 0.8094220769840587693, 1.000000000000000000),
 ( 1.000000000000000000, 0.8022659121986455144, 1.000000000000000000),
 ( 1.000000000000000000, 0.7845681159034547658, 1.000000000000000000),
 ( 1.000000000000000000, 0.7744426415184183510, 1.000000000000000000),
 ( 1.000000000000000000, 0.7522890290929796775, 1.000000000000000000),
 ( 1.000000000000000000, 0.7403540167214540668, 1.000000000000000000),
 ( 1.000000000000000000, 0.7283825911960212229, 1.000000000000000000) ) ) 
 REPRESENTATION_ITEM ( '' )  SURFACE ( )  );
#4319 = CARTESIAN_POINT ( 'NONE',  ( 0.6435666744728262278, -1.544684321070708188, 0.4182417262808778013 ) ) ;
#4320 = CARTESIAN_POINT ( 'NONE',  ( 0.000000000000000000, 0.000000000000000000, 0.000000000000000000 ) ) ;
#4321 = CARTESIAN_POINT ( 'NONE',  ( 0.2797581386905990675, -1.667519014922642873, 0.4662658620133214304 ) ) ;
#4322 = PERSON_AND_ORGANIZATION_ROLE ( 'creator' ) ;
#4323 = CARTESIAN_POINT ( 'NONE',  ( 0.007337869580115062226, -0.9842806402802338761, 0.4958900936016981120 ) ) ;
#4324 = CARTESIAN_POINT ( 'NONE',  ( 0.3511758406044653280, -1.510956930971387724, -0.7187326247832955817 ) ) ;
#4325 = PRODUCT_DEFINITION_CONTEXT ( 'detailed design', #6889, 'design' ) ;
#4326 = CARTESIAN_POINT ( 'NONE',  ( 0.1097570854172637417, -1.412022420605677953, 0.6115137485124468864 ) ) ;
#4327 = DIRECTION ( 'NONE',  ( -8.881784197001246407E-16, 2.361472542561082612E-16, -1.000000000000000000 ) ) ;
#4328 = LINE ( 'NONE', #17676, #31781 ) ;
#4329 = DIRECTION ( 'NONE',  ( 0.000000000000000000, 0.000000000000000000, -1.000000000000000000 ) ) ;
#4330 = AXIS2_PLACEMENT_3D ( 'NONE', #15747, #13485, #765 ) ;
#4331 = CARTESIAN_POINT ( 'NONE',  ( 0.7066102454780193165, -1.509906364535708923, 0.5603690879523279822 ) ) ;
#4332 = EDGE_LOOP ( 'NONE', ( #12134, #19945, #33593, #38616 ) ) ;
#4333 = CARTESIAN_POINT ( 'NONE',  ( 0.1727484476632766552, -0.5194822410394417389, 0.1386055728184389102 ) ) ;
#4334 = ORIENTED_EDGE ( 'NONE', *, *, #32557, .T. ) ;
#4335 = APPROVAL_PERSON_ORGANIZATION ( #38291, #2358, #25770 ) ;
#4336 = DIRECTION ( 'NONE',  ( 0.000000000000000000, 0.000000000000000000, -1.000000000000000000 ) ) ;
#4337 = CARTESIAN_POINT ( 'NONE',  ( 0.1402024954270775225, -0.6142130989947057751, 0.3459447826026630368 ) ) ;
#4339 = ORIENTED_EDGE ( 'NONE', *, *, #3020, .F. ) ;
#4338 = CARTESIAN_POINT ( 'NONE',  ( 0.5074366505258062210, -1.675708488637823068, -0.4286118871247626694 ) ) ;
#4340 = CIRCLE ( 'NONE', #31954, 0.1333070866141731758 ) ;
#4342 = VERTEX_POINT ( 'NONE', #12881 ) ;
#4341 = VERTEX_POINT ( 'NONE', #19257 ) ;
#4343 = DIRECTION ( 'NONE',  ( -1.000000000000000000, -0.000000000000000000, -0.000000000000000000 ) ) ;
#4344 = ORIENTED_EDGE ( 'NONE', *, *, #33135, .T. ) ;
#4345 = CARTESIAN_POINT ( 'NONE',  ( 0.03052257359372401863, -0.7992890816565190182, 0.6712346997200854259 ) ) ;
#4346 = DIRECTION ( 'NONE',  ( -1.000000000000000000, 0.000000000000000000, 0.000000000000000000 ) ) ;
#4347 = CARTESIAN_POINT ( 'NONE',  ( 0.6206746333706361085, -1.620953523311430944, -0.4903377927301240669 ) ) ;
#4348 = CALENDAR_DATE ( 2026, 13, 10 ) ;
#4349 = CARTESIAN_POINT ( 'NONE',  ( -0.1731185243557763487, 0.5373335498847187086, 0.3599999999999993205 ) ) ;
#4351 = ORIENTED_EDGE ( 'NONE', *, *, #40586, .F. ) ;
#4350 = ORIENTED_EDGE ( 'NONE', *, *, #450, .T. ) ;
#4352 = CARTESIAN_POINT ( 'NONE',  ( 0.1991609519065172529, -0.9184688065175017346, 0.6111039586238895538 ) ) ;
#4353 = CARTESIAN_POINT ( 'NONE',  ( 0.09335350967634557795, -0.5942487015407079687, 0.2614486645500827544 ) ) ;
#4354 = CARTESIAN_POINT ( 'NONE',  ( 0.5391681719232660486, -1.519059681939239903, 0.5745203956527785705 ) ) ;
#4355 = ORIENTED_EDGE ( 'NONE', *, *, #26795, .F. ) ;
#4356 = CARTESIAN_POINT ( 'NONE',  ( 0.05545227241544782582, -1.226087868501680056, 0.6599560881964448011 ) ) ;
#4357 = CARTESIAN_POINT ( 'NONE',  ( 0.6045036416640916510, -1.481621646331015008, 0.5979483913144312268 ) ) ;
#4358 = CYLINDRICAL_SURFACE ( 'NONE', #27162, 0.1946589359789742957 ) ;
#4359 = CARTESIAN_POINT ( 'NONE',  ( -0.1743922129835730472, -0.5166151207188712791, 0.08499999999999964528 ) ) ;
#4360 = CARTESIAN_POINT ( 'NONE',  ( 0.3528298061772759953, -1.603578276458837104, -0.7003206377943665961 ) ) ;
#4361 = VECTOR ( 'NONE', #24036, 39.37007874015748143 ) ;
#4362 = CARTESIAN_POINT ( 'NONE',  ( 0.4711420575750281947, -1.592335044512171782, -0.5952420774259647995 ) ) ;
#4363 = EDGE_CURVE ( 'NONE', #35558, #9616, #28296, .T. ) ;
#4364 = DIRECTION ( 'NONE',  ( -0.4999999999999988898, 0.5755298573121169214, -0.6471208413753147815 ) ) ;
#4365 = CYLINDRICAL_SURFACE ( 'NONE', #17334, 0.08000000000000000167 ) ;
#4366 = CARTESIAN_POINT ( 'NONE',  ( 0.01165121832836692878, -0.7716130889810013382, -0.09920548477954149735 ) ) ;
#4367 = CARTESIAN_POINT ( 'NONE',  ( 0.5454855820205488648, -1.408499188346827857, 0.7723196400189406008 ) ) ;
#4368 = LOCAL_TIME ( 0, 53, 7.000000000000000000, #39502 ) ;
#4369 = ADVANCED_FACE ( 'NONE', ( #6482 ), #9780, .T. ) ;
#4370 = DIRECTION ( 'NONE',  ( -0.8315239468457111816, -0.5057278275750267671, -0.2297983686590817365 ) ) ;
#4371 = CARTESIAN_POINT ( 'NONE',  ( 0.5433433239293584682, -1.169038973927291503, 0.5856983068965047057 ) ) ;
#4372 = EDGE_CURVE ( 'NONE', #27821, #20248, #29278, .T. ) ;
#4373 = AXIS2_PLACEMENT_3D ( 'NONE', #7539, #26887, #20115 ) ;
#4374 = CARTESIAN_POINT ( 'NONE',  ( 0.1877024697326355740, -1.541847387273544756, 0.6461194557730155497 ) ) ;
#4375 = CARTESIAN_POINT ( 'NONE',  ( 0.2803482358567763177, -0.9348470554797825294, 0.5439829518127811125 ) ) ;
#4376 = COORDINATED_UNIVERSAL_TIME_OFFSET ( 0, 0, .AHEAD. ) ;
#4377 = CARTESIAN_POINT ( 'NONE',  ( 0.5433433239293584682, -1.169038973927291503, 0.5856983068965047057 ) ) ;
#4378 = DIRECTION ( 'NONE',  ( 8.881784197001246407E-16, -2.361472542561082612E-16, 1.000000000000000000 ) ) ;
#4379 = ADVANCED_FACE ( 'NONE', ( #38569 ), #10390, .T. ) ;
#4380 = ORIENTED_EDGE ( 'NONE', *, *, #32627, .F. ) ;
#4381 = CARTESIAN_POINT ( 'NONE',  ( 0.2999999999999782840, -1.939620212199285598, -0.6711716461755767860 ) ) ;
#4382 = PRODUCT_RELATED_PRODUCT_CATEGORY ( 'detail', '', ( #21216 ) ) ;
#4383 = CARTESIAN_POINT ( 'NONE',  ( 0.01056251376256645870, -0.5300776972628027384, 0.1582814761548828608 ) ) ;
#4384 = CARTESIAN_POINT ( 'NONE',  ( 0.09963077645664282500, -1.298161551546404890, 0.4482597153589827910 ) ) ;
#4385 = VERTEX_POINT ( 'NONE', #31401 ) ;
#4386 = VECTOR ( 'NONE', #2562, 39.37007874015747433 ) ;
#4387 = CARTESIAN_POINT ( 'NONE',  ( 0.5156877488165810819, -1.667601403840327734, -0.4359157956494498776 ) ) ;
#4388 = CARTESIAN_POINT ( 'NONE',  ( 0.4929832608774247782, -1.104425667152665991, 0.8058332650092189242 ) ) ;
#4390 = ORIENTED_EDGE ( 'NONE', *, *, #22787, .T. ) ;
#4389 = ORIENTED_EDGE ( 'NONE', *, *, #17255, .F. ) ;
#4391 = FACE_OUTER_BOUND ( 'NONE', #27343, .T. ) ;
#4392 = EDGE_LOOP ( 'NONE', ( #19976, #21437, #5938, #32322 ) ) ;
#4393 = DIRECTION ( 'NONE',  ( 1.000000000000000000, 1.024442997624095147E-14, 1.138269997360105631E-15 ) ) ;
#4394 = APPLIED_SECURITY_CLASSIFICATION_ASSIGNMENT ( #12929, ( #40666 ) ) ;
#4395 = CARTESIAN_POINT ( 'NONE',  ( -0.02000000000000000042, -2.320036485105098301, -0.2941690811493925528 ) ) ;
#4396 = CARTESIAN_POINT ( 'NONE',  ( -0.05137569054208514924, 0.4554428576828045139, -0.1244487204292454574 ) ) ;
#4397 = ORIENTED_EDGE ( 'NONE', *, *, #39795, .F. ) ;
#4398 = CARTESIAN_POINT ( 'NONE',  ( 0.1875000000000003608, -0.4593131964907913312, 0.1856949347217509150 ) ) ;
#4399 = CARTESIAN_POINT ( 'NONE',  ( 0.08753440268785935008, -0.6845692626716123330, 0.1571571781002649437 ) ) ;
#4400 = CARTESIAN_POINT ( 'NONE',  ( 0.01220488673141941274, -0.4284039384351941426, 0.1457185332388690469 ) ) ;
#4401 = CARTESIAN_POINT ( 'NONE',  ( 0.09266747603540267941, -0.6010366268050462146, 0.3369889307053728911 ) ) ;
#4403 = DIRECTION ( 'NONE',  ( 0.000000000000000000, 0.000000000000000000, -1.000000000000000000 ) ) ;
#4402 = CARTESIAN_POINT ( 'NONE',  ( 0.09285203301658104258, -1.021206517960446369, 0.8557725610849984399 ) ) ;
#4404 = CARTESIAN_POINT ( 'NONE',  ( 0.1443024366174217588, -1.195940908848212691, 0.6505907527369143573 ) ) ;
#4405 = ORIENTED_EDGE ( 'NONE', *, *, #7874, .F. ) ;
#4406 = ORIENTED_EDGE ( 'NONE', *, *, #10456, .T. ) ;
#4407 = CARTESIAN_POINT ( 'NONE',  ( 0.2093596354519730585, -1.281064938727221714, -0.3178472134378123592 ) ) ;
#4408 = CARTESIAN_POINT ( 'NONE',  ( 0.1912291182594794137, -0.6824372825164394252, 0.6358572396827846251 ) ) ;
#4409 = CARTESIAN_POINT ( 'NONE',  ( -0.03674260963082301434, 0.2486114773148996593, -0.4115095709379173461 ) ) ;
#4410 = ADVANCED_FACE ( 'NONE', ( #16564 ), #28902, .F. ) ;
#4411 = CARTESIAN_POINT ( 'NONE',  ( -0.04229883635637964739, -0.4443296166163696603, -0.1489543265340548261 ) ) ;
#4412 = EDGE_CURVE ( 'NONE', #9762, #20650, #25439, .T. ) ;
#4413 = DIRECTION ( 'NONE',  ( 0.000000000000000000, 0.000000000000000000, -1.000000000000000000 ) ) ;
#4414 = ADVANCED_FACE ( 'NONE', ( #29108 ), #10198, .T. ) ;
#4415 = CARTESIAN_POINT ( 'NONE',  ( 0.4209912206648682154, -1.078067379053157193, -0.5155029497116575543 ) ) ;
#4416 = CARTESIAN_POINT ( 'NONE',  ( 0.1912376716460947867, -0.5867422834582064484, 0.1926850933134615362 ) ) ;
#4417 = CARTESIAN_POINT ( 'NONE',  ( -0.1151895542371778602, -0.5267561842548691420, 0.1296992319623858358 ) ) ;
#4418 = CARTESIAN_POINT ( 'NONE',  ( 0.01456394726322781524, -0.9250865771959065897, 0.5675178823144181317 ) ) ;
#4419 = DIRECTION ( 'NONE',  ( 8.881784197001246407E-16, -2.361472542561082612E-16, 1.000000000000000000 ) ) ;
#4420 = CARTESIAN_POINT ( 'NONE',  ( 0.5170632769343359580, -1.646684529498529503, -0.5823716739448009383 ) ) ;
#4421 = CARTESIAN_POINT ( 'NONE',  ( 0.3869860216863779678, -1.170324191591702867, 0.7132054132965995885 ) ) ;
#4422 = CARTESIAN_POINT ( 'NONE',  ( -0.05252049209742690183, -0.2682992380086431927, -0.3847779939372243385 ) ) ;
#4423 = ADVANCED_FACE ( 'NONE', ( #22554, #6682 ), #6288, .T. ) ;
#4424 = ORIENTED_EDGE ( 'NONE', *, *, #36822, .T. ) ;
#4425 = DIRECTION ( 'NONE',  ( 0.8308509739180691689, 0.4796346601509333119, 0.2822007298383447660 ) ) ;
#4426 = ORIENTED_EDGE ( 'NONE', *, *, #34617, .F. ) ;
#4427 = CARTESIAN_POINT ( 'NONE',  ( 0.09014181593920955748, -0.5678796035371341810, 0.1769828697681403995 ) ) ;
#4428 = CARTESIAN_POINT ( 'NONE',  ( 0.3654468122243346162, -1.742897531900985175, -0.4899584472101493060 ) ) ;
#4429 = CARTESIAN_POINT ( 'NONE',  ( 0.4091244934080342510, -1.134466909110688482, 0.4685100012138834202 ) ) ;
#4430 = DIMENSIONAL_EXPONENTS ( 1.000000000000000000, 0.000000000000000000, 0.000000000000000000, 0.000000000000000000, 0.000000000000000000, 0.000000000000000000, 0.000000000000000000 ) ;
#4431 = CARTESIAN_POINT ( 'NONE',  ( 0.03202889392918712580, -0.8409986250695938859, 0.1457185332388704624 ) ) ;
#4432 = EDGE_LOOP ( 'NONE', ( #10663, #11973, #23092, #20506, #8387 ) ) ;
#4433 = CARTESIAN_POINT ( 'NONE',  ( -0.1656893171628753825, 0.4813634391809688551, 0.3338433979331971169 ) ) ;
#4434 = CARTESIAN_POINT ( 'NONE',  ( 0.1499999999999994671, 0.4638115001430989648, -0.2459753896937820483 ) ) ;
#4435 = CARTESIAN_POINT ( 'NONE',  ( 0.1466125325700726734, -1.398062017178772098, 0.4425755552918825830 ) ) ;
#4436 = CARTESIAN_POINT ( 'NONE',  ( 0.4862264814005418656, -1.268791747036731365, 0.6246861129760243880 ) ) ;
#4438 = DIRECTION ( 'NONE',  ( -0.4999551463232372317, 0.8660512985181135770, -0.000000000000000000 ) ) ;
#4437 = DIRECTION ( 'NONE',  ( 1.000000000000000000, 0.000000000000000000, 0.000000000000000000 ) ) ;
#4439 = CARTESIAN_POINT ( 'NONE',  ( 0.5838900649597887904, -1.499867930881839007, -0.4391511121979080889 ) ) ;
#4440 = EDGE_LOOP ( 'NONE', ( #20914, #35779, #3983, #39960 ) ) ;
#4441 = DIRECTION ( 'NONE',  ( 0.000000000000000000, 0.000000000000000000, -1.000000000000000000 ) ) ;
#4442 = ORIENTED_EDGE ( 'NONE', *, *, #8723, .F. ) ;
#4443 = CARTESIAN_POINT ( 'NONE',  ( 0.3467465376597937410, -1.426445918686239489, 0.8672919671349224036 ) ) ;
#4445 = CARTESIAN_POINT ( 'NONE',  ( 0.4739903723793378321, -1.126753373801576252, -0.6501307139337872965 ) ) ;
#4444 = CARTESIAN_POINT ( 'NONE',  ( 0.06705560988554902513, -0.6676997200371664887, -0.0009185627879479015250 ) ) ;
#4446 = CARTESIAN_POINT ( 'NONE',  ( 0.1586456724622636871, -1.275316570454761322, 0.4817113887073902756 ) ) ;
#4447 = ORIENTED_EDGE ( 'NONE', *, *, #17578, .T. ) ;
#4448 = ORIENTED_EDGE ( 'NONE', *, *, #31016, .T. ) ;
#4449 = LINE ( 'NONE', #4636, #35273 ) ;
#4450 = CARTESIAN_POINT ( 'NONE',  ( 0.1307689245043377746, -0.6231473675091006026, 0.3697794014886608416 ) ) ;
#4451 = ORIENTED_EDGE ( 'NONE', *, *, #10258, .T. ) ;
#4452 = DIRECTION ( 'NONE',  ( 0.000000000000000000, 3.330669073875469621E-16, 1.000000000000000000 ) ) ;
#4453 = DIRECTION ( 'NONE',  ( 0.8660512985181135770, 0.4999551463232370652, 0.000000000000000000 ) ) ;
#4454 = EDGE_CURVE ( 'NONE', #31881, #36413, #17470, .T. ) ;
#4455 = CARTESIAN_POINT ( 'NONE',  ( 0.4147930180073937656, -1.739805112484396954, -0.4462242041100615286 ) ) ;
#4456 = CARTESIAN_POINT ( 'NONE',  ( 0.1579832900275356389, -1.275892853358665979, 0.4209669457040660645 ) ) ;
#4457 = ADVANCED_FACE ( 'NONE', ( #19050 ), #19653, .T. ) ;
#4458 = CARTESIAN_POINT ( 'NONE',  ( 0.07197331016010956317, -1.314323866689726339, 0.4956685533872550176 ) ) ;
#4459 = CARTESIAN_POINT ( 'NONE',  ( 0.05562150110511214496, -0.02029635476683555595, 0.4604536315446556283 ) ) ;
#4460 = CARTESIAN_POINT ( 'NONE',  ( 0.1875000000000001943, -0.4593131964907913312, 0.1457185332388694909 ) ) ;
#4461 = CARTESIAN_POINT ( 'NONE',  ( 0.05999999999999990757, 0.07140090991423790612, -0.1319162994607513684 ) ) ;
#4462 = CYLINDRICAL_SURFACE ( 'NONE', #29090, 0.9087847906030127598 ) ;
#4463 = APPROVAL_ROLE ( '' ) ;
#4464 = CARTESIAN_POINT ( 'NONE',  ( 0.6483372838204546351, -1.461228087998845959, -0.6196388347441599276 ) ) ;
#4465 = CARTESIAN_POINT ( 'NONE',  ( 0.05078310099560720547, 0.2374900923169198097, 0.4099167927581913728 ) ) ;
#4466 = CARTESIAN_POINT ( 'NONE',  ( 0.1837736376643801794, -0.5304624996123088465, 0.05163021866974163571 ) ) ;
#4467 = CARTESIAN_POINT ( 'NONE',  ( 0.4687869482605488969, -1.212150898723653114, 0.4951799515542131269 ) ) ;
#4468 = CARTESIAN_POINT ( 'NONE',  ( 0.1398272630092362578, -1.288459453437826419, 0.4193546253734958817 ) ) ;
#4469 = CARTESIAN_POINT ( 'NONE',  ( 3.304294434668030104E-05, -0.6893515101347650331, 0.1975634471597359221 ) ) ;
#4470 = CARTESIAN_POINT ( 'NONE',  ( 0.5835378010919568537, -1.549988096145974215, -0.6077179222230424394 ) ) ;
#4471 = EDGE_CURVE ( 'NONE', #39166, #35163, #35211, .T. ) ;
#4472 = FACE_OUTER_BOUND ( 'NONE', #36633, .T. ) ;
#4473 = APPROVAL ( #1894, 'UNKNOWN' ) ;
#4474 = CARTESIAN_POINT ( 'NONE',  ( 0.5959315179729189893, -1.587052097778458348, 0.4182417262808776903 ) ) ;
#4475 = CARTESIAN_POINT ( 'NONE',  ( -0.05491348488830474078, -0.2511509903618516226, 0.3886212643843945380 ) ) ;
#4476 = ADVANCED_FACE ( 'NONE', ( #12656 ), #3404, .T. ) ;
#4477 = CIRCLE ( 'NONE', #19602, 0.01000000000000002102 ) ;
#4478 = ORIENTED_EDGE ( 'NONE', *, *, #30346, .T. ) ;
#4479 = EDGE_LOOP ( 'NONE', ( #10510, #34855, #301, #24747, #18777, #38044, #15171 ) ) ;
#4480 = CARTESIAN_POINT ( 'NONE',  ( 0.3673730737733172935, -1.765061228214683364, -0.5843795697180308446 ) ) ;
#4481 = VERTEX_POINT ( 'NONE', #28505 ) ;
#4482 = DIRECTION ( 'NONE',  ( 0.8660512985181136880, 0.4999551463232367876, 0.000000000000000000 ) ) ;
#4483 = DIRECTION ( 'NONE',  ( 0.000000000000000000, 0.3090169943749439541, -0.9510565162951547524 ) ) ;
#4484 = CARTESIAN_POINT ( 'NONE',  ( 0.5037817747200005192, -1.302264079412044362, 0.7382972978228007355 ) ) ;
#4486 = EDGE_LOOP ( 'NONE', ( #33811, #23243, #6814, #9007 ) ) ;
#4485 = CARTESIAN_POINT ( 'NONE',  ( -0.04582713223189551627, 0.4389429380065683617, 0.2108029774974878590 ) ) ;
#4487 = CARTESIAN_POINT ( 'NONE',  ( 0.2974794542262550467, -0.9002722561939086043, 0.5860092920552725237 ) ) ;
#4488 = DIRECTION ( 'NONE',  ( 1.000000000000000000, 1.441651681710401470E-15, -8.317221240636930495E-16 ) ) ;
#4489 = ORIENTED_EDGE ( 'NONE', *, *, #14426, .T. ) ;
#4490 = CARTESIAN_POINT ( 'NONE',  ( 0.03113248654051816583, 0.000000000000000000, 0.000000000000000000 ) ) ;
#4491 = ORIENTED_EDGE ( 'NONE', *, *, #16592, .F. ) ;
#4492 = CARTESIAN_POINT ( 'NONE',  ( 0.03244836639777012866, -0.6168844639952264508, 0.3981205770845226977 ) ) ;
#4494 = DIRECTION ( 'NONE',  ( -0.01254811300245605755, -0.8659344938869285579, -0.4999999971568663826 ) ) ;
#4493 = CARTESIAN_POINT ( 'NONE',  ( 0.6503292821894245401, -1.549301679588444891, 0.4221565037074623827 ) ) ;
#4495 = CARTESIAN_POINT ( 'NONE',  ( 0.2316917763911649497, -1.232208891764917880, 0.5707417262808780478 ) ) ;
#4496 = CARTESIAN_POINT ( 'NONE',  ( 0.1153579089856115875, -1.330707596229020462, -0.3224262535835399901 ) ) ;
#4497 = VERTEX_POINT ( 'NONE', #381 ) ;
#4498 = CARTESIAN_POINT ( 'NONE',  ( -0.1684323895664678050, 0.5231977504175356897, 0.1528658435937002014 ) ) ;
#4499 = CARTESIAN_POINT ( 'NONE',  ( 0.1039773195064908201, -1.347850002784139578, -0.6754723133399438417 ) ) ;
#4500 = DIRECTION ( 'NONE',  ( 0.8660512985181134660, 0.4999551463232372317, 0.000000000000000000 ) ) ;
#4501 = CARTESIAN_POINT ( 'NONE',  ( 0.2792484994315600488, -1.098230303849151657, 0.7437165765675377571 ) ) ;
#4502 = CARTESIAN_POINT ( 'NONE',  ( 0.5968691484058664676, -1.478977895573694079, 0.6175733170218915546 ) ) ;
#4503 = EDGE_CURVE ( 'NONE', #15872, #23907, #10969, .T. ) ;
#4504 = CARTESIAN_POINT ( 'NONE',  ( 0.02953079040095687308, 0.09152108205202039160, -0.5223162075576429642 ) ) ;
#4505 = EDGE_CURVE ( 'NONE', #36967, #11216, #35878, .T. ) ;
#4506 = CARTESIAN_POINT ( 'NONE',  ( -0.1524914371963956017, 0.4722463545162183807, 0.3472338286530394225 ) ) ;
#4507 = SPHERICAL_SURFACE ( 'NONE', #22645, 0.01499999999999999944 ) ;
#4508 = LINE ( 'NONE', #10310, #11302 ) ;
#4509 = DIRECTION ( 'NONE',  ( 1.000000000000000000, 0.000000000000000000, 0.000000000000000000 ) ) ;
#4510 = CARTESIAN_POINT ( 'NONE',  ( 0.02953079040095700838, -0.09152108205202422186, -0.5223162075576424090 ) ) ;
#4511 = PERSON_AND_ORGANIZATION ( #28500, #32463 ) ;
#4512 = CARTESIAN_POINT ( 'NONE',  ( 0.03871195898642652844, -1.170490907799284219, 0.6777665691625279765 ) ) ;
#4513 = CARTESIAN_POINT ( 'NONE',  ( 0.1829983673741292505, -0.5078818111421493642, 0.09707803729949140981 ) ) ;
#4514 = CARTESIAN_POINT ( 'NONE',  ( 0.1729876862315062602, -0.5859491089648112272, 0.3201888025045112607 ) ) ;
#4515 = CARTESIAN_POINT ( 'NONE',  ( 0.3699999999999786793, -2.183180860297921466, -0.4437760292030870635 ) ) ;
#4516 = DIRECTION ( 'NONE',  ( 0.000000000000000000, 0.5781348229923758408, -0.8159412518334724362 ) ) ;
#4517 = CARTESIAN_POINT ( 'NONE',  ( -0.1172100234506803368, -0.4874937943216627323, 0.3357378396897046091 ) ) ;
#4518 = CARTESIAN_POINT ( 'NONE',  ( -0.1455608194604309513, -0.5249067277714104529, 0.1528658435937002014 ) ) ;
#4519 = ORIENTED_EDGE ( 'NONE', *, *, #25035, .F. ) ;
#4520 = ORIENTED_EDGE ( 'NONE', *, *, #12984, .T. ) ;
#4521 = CARTESIAN_POINT ( 'NONE',  ( 0.3862110256088818194, -1.731934476144515900, 0.4282538419479027247 ) ) ;
#4522 = ORIENTED_EDGE ( 'NONE', *, *, #247, .T. ) ;
#4523 = LINE ( 'NONE', #33128, #36169 ) ;
#4524 = CARTESIAN_POINT ( 'NONE',  ( 0.1521802402523282638, -0.6543157544505630030, 0.4235539958437135599 ) ) ;
#4525 = EDGE_CURVE ( 'NONE', #16583, #30458, #36521, .T. ) ;
#4527 = ORIENTED_EDGE ( 'NONE', *, *, #21073, .F. ) ;
#4526 = CARTESIAN_POINT ( 'NONE',  ( -0.0004984919465477205157, -0.7422635077827434147, -0.01332428955721734649 ) ) ;
#4529 = ORIENTED_EDGE ( 'NONE', *, *, #2652, .F. ) ;
#4528 = EDGE_LOOP ( 'NONE', ( #4727, #38829, #31927, #17856 ) ) ;
#4530 = CARTESIAN_POINT ( 'NONE',  ( 0.4127911607195844379, -1.067806736826314218, 0.8805981392688931875 ) ) ;
#4531 = ORIENTED_EDGE ( 'NONE', *, *, #20282, .F. ) ;
#4532 = CARTESIAN_POINT ( 'NONE',  ( 0.2075111833072861844, -1.439991211493228285, 0.9346039839131908833 ) ) ;
#4533 = CARTESIAN_POINT ( 'NONE',  ( 0.02872242845529790478, 0.4768947642620333105, 0.2371557650701984765 ) ) ;
#4534 = DIRECTION ( 'NONE',  ( 1.000000000000000000, 0.000000000000000000, 0.000000000000000000 ) ) ;
#4535 = APPROVAL_STATUS ( 'not_yet_approved' ) ;
#4536 = CARTESIAN_POINT ( 'NONE',  ( 0.002842240357859183043, -0.6339827964191877552, 0.04185307883324698719 ) ) ;
#4538 = EDGE_LOOP ( 'NONE', ( #10066, #20400, #34300, #25096, #3219 ) ) ;
#4537 = ORIENTED_EDGE ( 'NONE', *, *, #5199, .F. ) ;
#4539 = CARTESIAN_POINT ( 'NONE',  ( 0.1173537979040395057, -0.8419870544700812642, 0.4212373387996306007 ) ) ;
#4540 =( REPRESENTATION_RELATIONSHIP ('NONE','NONE', #27514, #17542 ) REPRESENTATION_RELATIONSHIP_WITH_TRANSFORMATION ( #28744 )SHAPE_REPRESENTATION_RELATIONSHIP( ) );
#4541 = LINE ( 'NONE', #14412, #15219 ) ;
#4542 = CARTESIAN_POINT ( 'NONE',  ( 0.09200891480963520330, -0.5638355028864769913, 0.2394803638925667999 ) ) ;
#4543 =( BOUNDED_SURFACE ( )  B_SPLINE_SURFACE ( 3, 2, ( 
 ( #15259, #30701, #9084 ),
 ( #28214, #21650, #34384 ),
 ( #27816, #9279, #12574 ),
 ( #18346, #40351, #18767 ),
 ( #36852, #81, #37673 ),
 ( #21243, #31498, #2521 ),
 ( #22072, #28418, #34595 ),
 ( #6398, #15061, #18966 ),
 ( #3308, #15871, #40141 ),
 ( #11969, #8884, #21460 ) ),
 .UNSPECIFIED., .F., .F., .F. ) 
 B_SPLINE_SURFACE_WITH_KNOTS ( ( 4, 2, 2, 2, 4 ),
 ( 3, 3 ),
 ( 0.01609622701100840714, 0.01664468962834504337, 0.01719315224568167960, 0.01774161486301831236, 0.01829007748035494860 ),
 ( 0.000000000000000000, 1.000000000000000000 ),
 .UNSPECIFIED. ) 
 GEOMETRIC_REPRESENTATION_ITEM ( )  RATIONAL_B_SPLINE_SURFACE ( (
 ( 1.000000000000000000, 0.7348357107202583283, 1.000000000000000000),
 ( 1.000000000000000000, 0.7390003998219781822, 1.000000000000000000),
 ( 1.000000000000000000, 0.7469310527984605041, 1.000000000000000000),
 ( 1.000000000000000000, 0.7680671187860059757, 1.000000000000000000),
 ( 1.000000000000000000, 0.7813269647889241609, 1.000000000000000000),
 ( 1.000000000000000000, 0.8093722468179129770, 1.000000000000000000),
 ( 1.000000000000000000, 0.8244642440797537164, 1.000000000000000000),
 ( 1.000000000000000000, 0.8536748302854195725, 1.000000000000000000),
 ( 1.000000000000000000, 0.8677611553907019770, 1.000000000000000000),
 ( 1.000000000000000000, 0.8808937523906948952, 1.000000000000000000) ) ) 
 REPRESENTATION_ITEM ( '' )  SURFACE ( )  );
#4544 = CARTESIAN_POINT ( 'NONE',  ( 0.5391088926460998465, -1.519050063081437418, 0.5735442466919873361 ) ) ;
#4545 = CARTESIAN_POINT ( 'NONE',  ( -0.3000000000000000999, -2.845511416290244622, -0.3415338532332813926 ) ) ;
#4546 = LINE ( 'NONE', #23313, #6056 ) ;
#4547 = CARTESIAN_POINT ( 'NONE',  ( 0.6633872118601743528, -1.508244317614790386, 0.3999406418104182737 ) ) ;
#4548 = CARTESIAN_POINT ( 'NONE',  ( 0.3304297980271364010, -1.754259251785285301, 0.5825477521894050215 ) ) ;
#4549 = CARTESIAN_POINT ( 'NONE',  ( -0.3000000000000000999, -2.183180860297908144, -0.4937760292030871079 ) ) ;
#4550 = DIRECTION ( 'NONE',  ( -8.881784197001245421E-16, 2.361472542561082612E-16, -1.000000000000000000 ) ) ;
#4551 = CARTESIAN_POINT ( 'NONE',  ( 0.01161354615076396445, -0.8030843809549637058, -0.08599057514136099201 ) ) ;
#4552 = CARTESIAN_POINT ( 'NONE',  ( 0.5848508152300195828, -1.486263022089187036, 0.6467108361231791447 ) ) ;
#4553 = CARTESIAN_POINT ( 'NONE',  ( -0.01548846960707524721, 0.000000000000000000, 0.000000000000000000 ) ) ;
#4554 = DIRECTION ( 'NONE',  ( 1.000000000000000000, 0.000000000000000000, 0.000000000000000000 ) ) ;
#4555 = CARTESIAN_POINT ( 'NONE',  ( -0.001215370517532385992, -0.9049306443239834019, 0.2850616817831099770 ) ) ;
#4556 = CARTESIAN_POINT ( 'NONE',  ( 0.2007793764868952557, -0.8804627652107338553, 0.3298308470297674488 ) ) ;
#4557 = APPROVAL_STATUS ( 'not_yet_approved' ) ;
#4558 = CARTESIAN_POINT ( 'NONE',  ( 0.2170862770790429608, -0.5809856703168675418, 0.4747658466717744608 ) ) ;
#4559 = CARTESIAN_POINT ( 'NONE',  ( 0.3971737171416530598, -1.599718167121974677, -0.6188829515567775275 ) ) ;
#4560 = CARTESIAN_POINT ( 'NONE',  ( 0.3084490738248236719, -1.760918681657249518, 0.5685408905292573811 ) ) ;
#4561 = ORIENTED_EDGE ( 'NONE', *, *, #27044, .T. ) ;
#4562 = CARTESIAN_POINT ( 'NONE',  ( 0.3222894045021684195, -1.758215778056678724, 0.5682417262808792113 ) ) ;
#4563 = CARTESIAN_POINT ( 'NONE',  ( 0.004162127911717961384, -0.5769282519883277560, 0.3208275921695811217 ) ) ;
#4564 = DIRECTION ( 'NONE',  ( -0.4261641068392694742, -0.9046458721742379749, 0.000000000000000000 ) ) ;
#4565 = ORIENTED_EDGE ( 'NONE', *, *, #495, .F. ) ;
#4566 = DIRECTION ( 'NONE',  ( -8.881784197001245421E-16, 2.361472542561082612E-16, -1.000000000000000000 ) ) ;
#4567 = CARTESIAN_POINT ( 'NONE',  ( 0.2073655362268157221, -0.5791461380176760043, 0.4026997059449013427 ) ) ;
#4569 = ORIENTED_EDGE ( 'NONE', *, *, #20237, .F. ) ;
#4568 = ORIENTED_EDGE ( 'NONE', *, *, #29268, .F. ) ;
#4570 = CARTESIAN_POINT ( 'NONE',  ( 0.004755934575889525159, -1.810517711902423166, -0.6424739212913328501 ) ) ;
#4571 = VERTEX_POINT ( 'NONE', #10802 ) ;
#4572 = ORIENTED_EDGE ( 'NONE', *, *, #37391, .T. ) ;
#4573 = DIRECTION ( 'NONE',  ( 1.000000000000000000, 2.280301054154495132E-31, -1.664003471950577689E-31 ) ) ;
#4574 = CARTESIAN_POINT ( 'NONE',  ( -0.2746410161513779258, -3.941790907013290823, -0.4709369376873030477 ) ) ;
#4575 = CIRCLE ( 'NONE', #20463, 0.01499999999999994220 ) ;
#4576 = DIRECTION ( 'NONE',  ( 0.000000000000000000, 0.000000000000000000, 1.000000000000000000 ) ) ;
#4577 = EDGE_LOOP ( 'NONE', ( #19787, #4718, #24103, #39699 ) ) ;
#4578 = CARTESIAN_POINT ( 'NONE',  ( 0.4259907721281001036, -1.086727892038337417, -0.5155029497116575543 ) ) ;
#4579 = EDGE_CURVE ( 'NONE', #19668, #4809, #20125, .T. ) ;
#4580 = CARTESIAN_POINT ( 'NONE',  ( 0.09767013716984308813, -0.7037575184182598420, 0.3163885053921727808 ) ) ;
#4581 = CARTESIAN_POINT ( 'NONE',  ( 0.2062639539987025650, -1.309334957533395016, 1.035302674386483712 ) ) ;
#4582 = CARTESIAN_POINT ( 'NONE',  ( 0.2191569312961403060, -0.9640130920718992247, 0.7596813669479296482 ) ) ;
#4584 = CARTESIAN_POINT ( 'NONE',  ( 0.6540709664215760277, -1.593060928864740156, 0.5182417262812423209 ) ) ;
#4583 = CARTESIAN_POINT ( 'NONE',  ( 0.2486902987866957404, -1.562349929515986613, 0.8878345574556952835 ) ) ;
#4585 = CARTESIAN_POINT ( 'NONE',  ( 0.1283426906650361188, -1.153757123153984487, 0.6565515665500586406 ) ) ;
#4586 = ORIENTED_EDGE ( 'NONE', *, *, #32264, .T. ) ;
#4587 = CARTESIAN_POINT ( 'NONE',  ( -0.1399999999999997358, 0.000000000000000000, 0.000000000000000000 ) ) ;
#4588 = CARTESIAN_POINT ( 'NONE',  ( 0.1899592773905523502, -0.4742143251099648626, 0.2358144428592672259 ) ) ;
#4589 = CARTESIAN_POINT ( 'NONE',  ( 0.000000000000000000, -0.6872203660140440151, -0.1152499451672195641 ) ) ;
#4590 = ADVANCED_FACE ( 'NONE', ( #35896 ), #1352, .T. ) ;
#4591 = APPLIED_PERSON_AND_ORGANIZATION_ASSIGNMENT ( #12486, #33913, ( #17475 ) ) ;
#4592 = CARTESIAN_POINT ( 'NONE',  ( -0.04085667396267319423, -0.4416859672262361536, -0.1657724178830653206 ) ) ;
#4593 = CARTESIAN_POINT ( 'NONE',  ( 0.1999999999999789724, -2.183180860297921466, -0.4937760292030871079 ) ) ;
#4594 = DIRECTION ( 'NONE',  ( 0.000000000000000000, 8.195543980992787683E-15, -1.000000000000000000 ) ) ;
#4595 = CARTESIAN_POINT ( 'NONE',  ( 0.4660228360541302517, -1.069033551699853479, 0.7465831672886248382 ) ) ;
#4596 = DIRECTION ( 'NONE',  ( 1.000000000000000000, 2.341930812374887555E-31, -1.664003471950578127E-31 ) ) ;
#4597 = AXIS2_PLACEMENT_3D ( 'NONE', #7516, #32812, #1376 ) ;
#4598 = CARTESIAN_POINT ( 'NONE',  ( 0.01896931156525897069, 0.5123785568735239604, -0.08888416637129735454 ) ) ;
#4599 = CARTESIAN_POINT ( 'NONE',  ( 0.3267512268740185855, -1.294129692828816847, 0.5558767983972462412 ) ) ;
#4600 = ORIENTED_EDGE ( 'NONE', *, *, #32849, .T. ) ;
#4601 = CARTESIAN_POINT ( 'NONE',  ( 0.2396306281060514576, -0.9727409984848369717, 0.6921125950347779554 ) ) ;
#4602 = CARTESIAN_POINT ( 'NONE',  ( -0.2666757540196697529, 0.4921670437878978843, 0.08499999999999936773 ) ) ;
#4603 = CARTESIAN_POINT ( 'NONE',  ( -0.05616044724337304617, -0.2782405634116419391, -0.3655497896892178078 ) ) ;
#4604 = AXIS2_PLACEMENT_3D ( 'NONE', #2481, #8843, #244 ) ;
#4605 = ORIENTED_EDGE ( 'NONE', *, *, #25393, .F. ) ;
#4606 = DIRECTION ( 'NONE',  ( -8.881784197001246407E-16, 2.361472542561082612E-16, -1.000000000000000000 ) ) ;
#4607 = CARTESIAN_POINT ( 'NONE',  ( -0.04582705327698308878, 0.06484491888963164752, -0.4826014279685446606 ) ) ;
#4608 = AXIS2_PLACEMENT_3D ( 'NONE', #21383, #24670, #8586 ) ;
#4609 = CARTESIAN_POINT ( 'NONE',  ( 0.4218330423680932695, -1.124294433920346670, 0.5332777205563549172 ) ) ;
#4610 = EDGE_CURVE ( 'NONE', #1885, #32432, #16160, .T. ) ;
#4611 = CARTESIAN_POINT ( 'NONE',  ( 0.03596510069126712672, -0.8490400747553025207, 0.3220406306505974592 ) ) ;
#4612 = ORIENTED_EDGE ( 'NONE', *, *, #15432, .T. ) ;
#4613 = EDGE_CURVE ( 'NONE', #30897, #25550, #29952, .T. ) ;
#4614 = CARTESIAN_POINT ( 'NONE',  ( 0.05082303569918651676, 0.3162776479886627023, 0.3525632866555266642 ) ) ;
#4615 = CARTESIAN_POINT ( 'NONE',  ( 0.01548846960703785525, -0.3772621329472687357, 0.3651003739303496087 ) ) ;
#4616 = DIRECTION ( 'NONE',  ( 0.000000000000000000, 0.000000000000000000, -1.000000000000000000 ) ) ;
#4617 = CARTESIAN_POINT ( 'NONE',  ( -0.09579104668929040722, -0.04310840302197994911, 0.08500000000000008937 ) ) ;
#4618 = EDGE_CURVE ( 'NONE', #7904, #13794, #27136, .T. ) ;
#4619 = CARTESIAN_POINT ( 'NONE',  ( 0.4791019448734263886, -1.257055108044207170, 0.5997288661970070489 ) ) ;
#4621 = CARTESIAN_POINT ( 'NONE',  ( 0.5148961277138980330, -1.134264126613404366, 0.5683444520426285118 ) ) ;
#4620 = DIRECTION ( 'NONE',  ( 0.4999551463232372317, -0.8660512985181134660, 0.000000000000000000 ) ) ;
#4622 = EDGE_CURVE ( 'NONE', #26774, #23647, #10583, .T. ) ;
#4623 = CARTESIAN_POINT ( 'NONE',  ( 0.1877336102437491272, -0.9152557094465934018, 0.1737200839639440053 ) ) ;
#4624 = VERTEX_POINT ( 'NONE', #32599 ) ;
#4625 = EDGE_CURVE ( 'NONE', #23421, #37075, #38415, .T. ) ;
#4626 = DIRECTION ( 'NONE',  ( 0.000000000000000000, 0.7071067811865465735, 0.7071067811865484609 ) ) ;
#4627 = ORIENTED_EDGE ( 'NONE', *, *, #24402, .F. ) ;
#4628 = CARTESIAN_POINT ( 'NONE',  ( 0.1846367493580330643, -0.4547550531002670371, -0.08446770797961487831 ) ) ;
#4629 = CARTESIAN_POINT ( 'NONE',  ( 0.06534675320629550199, -0.6525200402172089964, 0.4542822255817380306 ) ) ;
#4631 = CARTESIAN_POINT ( 'NONE',  ( 0.08632066630984121247, -0.7257482948602275163, 0.1454106388476009426 ) ) ;
#4630 = CARTESIAN_POINT ( 'NONE',  ( 0.08979932128046543005, -0.5650858933015915353, 0.1321911050941584620 ) ) ;
#4632 = FACE_OUTER_BOUND ( 'NONE', #28325, .T. ) ;
#4633 = ORIENTED_EDGE ( 'NONE', *, *, #17472, .T. ) ;
#4634 = AXIS2_PLACEMENT_3D ( 'NONE', #40616, #18615, #37944 ) ;
#4635 = VERTEX_POINT ( 'NONE', #1559 ) ;
#4636 = CARTESIAN_POINT ( 'NONE',  ( -0.2399999999999999079, -3.745280840418592661, 0.04438736989695814261 ) ) ;
#4637 = CARTESIAN_POINT ( 'NONE',  ( 0.4578914926014877040, -1.316819426484251876, 0.8252663181933341807 ) ) ;
#4638 = ORIENTED_EDGE ( 'NONE', *, *, #791, .T. ) ;
#4639 = LINE ( 'NONE', #39420, #22456 ) ;
#4640 = CARTESIAN_POINT ( 'NONE',  ( 0.04157143636675179887, -0.4416880288200910609, 0.1614235308635223742 ) ) ;
#4641 = AXIS2_PLACEMENT_3D ( 'NONE', #3879, #840, #10280 ) ;
#4642 = EDGE_CURVE ( 'NONE', #18399, #25808, #21425, .T. ) ;
#4643 = CARTESIAN_POINT ( 'NONE',  ( 0.3839366250755201215, -1.757617928503105720, -0.4411224224773397373 ) ) ;
#4644 = VECTOR ( 'NONE', #33988, 39.37007874015748143 ) ;
#4645 = CARTESIAN_POINT ( 'NONE',  ( 0.2178456820578618947, -1.229745583036154111, 0.4925753654759648659 ) ) ;
#4646 = AXIS2_PLACEMENT_3D ( 'NONE', #12104, #27947, #22592 ) ;
#4647 = DIRECTION ( 'NONE',  ( 0.5209632322108713742, -0.8535791179992641142, 0.000000000000000000 ) ) ;
#4648 = DIRECTION ( 'NONE',  ( -1.000000000000000000, -2.403560570595279103E-31, 1.725633230170969455E-31 ) ) ;
#4649 = CARTESIAN_POINT ( 'NONE',  ( 0.7228851465660607323, -1.479175389011975428, 0.5919814340071456460 ) ) ;
#4650 = CARTESIAN_POINT ( 'NONE',  ( 0.3731036225605881551, -1.710599156003107968, -0.6119997028479188250 ) ) ;
#4651 = CARTESIAN_POINT ( 'NONE',  ( 0.03868264068766632396, -0.3066108573455326725, -0.3648330973802358379 ) ) ;
#4652 = CARTESIAN_POINT ( 'NONE',  ( 0.6165640848131422880, -1.623198970764877735, -0.5229364404254283061 ) ) ;
#4653 = CARTESIAN_POINT ( 'NONE',  ( 0.05269111014005566779, 0.2680748163012560137, 0.3844616952934046816 ) ) ;
#4654 = CARTESIAN_POINT ( 'NONE',  ( -0.1127677449505065793, -0.5183788106020520425, 0.3108513529155225164 ) ) ;
#4655 = DIRECTION ( 'NONE',  ( -0.4999551463232372317, 0.8660512985181135770, -0.000000000000000000 ) ) ;
#4656 = CARTESIAN_POINT ( 'NONE',  ( -0.02000000000000000042, -2.698373762442814350, -0.2370085142459261163 ) ) ;
#4657 = CARTESIAN_POINT ( 'NONE',  ( 0.002391669266185704034, -0.4944279760261894308, 0.2539263035736906149 ) ) ;
#4658 = CARTESIAN_POINT ( 'NONE',  ( 0.5735563720977525648, -1.542970242066289188, -0.5407299351178547209 ) ) ;
#4659 = DIRECTION ( 'NONE',  ( 1.000000000000000000, 6.779273404243070203E-32, 4.314083075427408311E-32 ) ) ;
#4660 = VECTOR ( 'NONE', #6104, 39.37007874015748143 ) ;
#4661 = CARTESIAN_POINT ( 'NONE',  ( -0.02000000000000000042, -2.379949255320110257, -0.6346823614705312533 ) ) ;
#4662 = CARTESIAN_POINT ( 'NONE',  ( -0.01548846960707415434, -0.3688619771572919093, 0.3775276577327012495 ) ) ;
#4663 = AXIS2_PLACEMENT_3D ( 'NONE', #23891, #33517, #36420 ) ;
#4664 = ORIENTED_EDGE ( 'NONE', *, *, #19793, .F. ) ;
#4665 = ORIENTED_EDGE ( 'NONE', *, *, #6869, .F. ) ;
#4666 = EDGE_CURVE ( 'NONE', #27138, #2769, #39143, .T. ) ;
#4667 = CARTESIAN_POINT ( 'NONE',  ( 0.4598690013600978954, -1.115092733745942422, 0.5813559894972742947 ) ) ;
#4668 = AXIS2_PLACEMENT_3D ( 'NONE', #6502, #22973, #35314 ) ;
#4669 = DIRECTION ( 'NONE',  ( -0.4999551463232372317, 0.8660512985181135770, -0.000000000000000000 ) ) ;
#4670 = VERTEX_POINT ( 'NONE', #20271 ) ;
#4671 = VECTOR ( 'NONE', #21414, 39.37007874015748143 ) ;
#4672 = CARTESIAN_POINT ( 'NONE',  ( -0.1212602504878780296, -0.5073146173917506552, 0.3749999999999999445 ) ) ;
#4673 = CIRCLE ( 'NONE', #27699, 0.05000000000000000971 ) ;
#4674 = ADVANCED_FACE ( 'NONE', ( #20070 ), #30263, .F. ) ;
#4675 = CARTESIAN_POINT ( 'NONE',  ( 0.3921016979062637575, -1.134099238832534162, 0.7924938403547856502 ) ) ;
#4677 = ORIENTED_EDGE ( 'NONE', *, *, #36554, .F. ) ;
#4676 = CARTESIAN_POINT ( 'NONE',  ( -0.1668451997768051753, 0.4851271022253541565, 0.1251051315678503029 ) ) ;
#4678 = CARTESIAN_POINT ( 'NONE',  ( 0.1851443459949622949, -0.7907988577364570837, 0.1906562862421710969 ) ) ;
#4679 = B_SPLINE_CURVE_WITH_KNOTS ( 'NONE', 3,
 ( #30725, #34008, #40168, #5812, #18371, #30918, #2742, #27846, #24770, #6013, #18795, #28441, #34621, #28659, #37485, #3763, #31136, #13210 ),
 .UNSPECIFIED., .F., .F.,
 ( 4, 2, 2, 2, 2, 2, 2, 2, 4 ),
 ( 0.000000000000000000, 0.0007746617437634289397, 0.001549323487526857879, 0.002323985231290287036, 0.003098646975053715759, 0.003873308718817144482, 0.004647970462580574072, 0.005422632206344002795, 0.006197293950107431518 ),
 .UNSPECIFIED. ) ;
#4680 = ADVANCED_FACE ( 'NONE', ( #11404 ), #32386, .T. ) ;
#4681 = CARTESIAN_POINT ( 'NONE',  ( 0.1766140053765036799, -0.4884607529735562892, 0.1457336358543773192 ) ) ;
#4682 = VERTEX_POINT ( 'NONE', #5410 ) ;
#4683 = CARTESIAN_POINT ( 'NONE',  ( 0.5959725435374871871, -1.484955338987114182, -0.6097788050097984192 ) ) ;
#4684 = EDGE_LOOP ( 'NONE', ( #4344, #37175, #16696, #20191, #9025 ) ) ;
#4685 = CARTESIAN_POINT ( 'NONE',  ( 0.03470550179739362306, -0.6286058976697491696, 0.4199817593366443336 ) ) ;
#4687 = FACE_OUTER_BOUND ( 'NONE', #19989, .T. ) ;
#4686 = CARTESIAN_POINT ( 'NONE',  ( 0.6822549037112248804, -1.506992060536815448, 0.4516695578178590020 ) ) ;
#4688 = CARTESIAN_POINT ( 'NONE',  ( 0.4972320539234349468, -1.080138254241686413, 0.5197417262808780025 ) ) ;
#4689 = CARTESIAN_POINT ( 'NONE',  ( 0.1308074600572272372, -1.309647876697553004, -0.3434689383624984771 ) ) ;
#4690 = ORIENTED_EDGE ( 'NONE', *, *, #7717, .T. ) ;
#4691 = CARTESIAN_POINT ( 'NONE',  ( -0.2343922129835731560, -0.5166151207188712791, 0.3599999999999990985 ) ) ;
#4692 = CARTESIAN_POINT ( 'NONE',  ( 0.1630093775333145978, -1.283014495054401793, 0.4182417262808778013 ) ) ;
#4693 = CARTESIAN_POINT ( 'NONE',  ( 0.3624061103390691096, -1.968824918581854932, -0.4968426515055719972 ) ) ;
#4694 = EDGE_CURVE ( 'NONE', #13346, #28462, #7511, .T. ) ;
#4695 = CARTESIAN_POINT ( 'NONE',  ( 0.4384185415325656532, -1.229513547616574609, 0.5866921512824373464 ) ) ;
#4696 = CARTESIAN_POINT ( 'NONE',  ( -0.3000000000000000999, -1.835749455202394298, -0.3938319975228649072 ) ) ;
#4697 = EDGE_CURVE ( 'NONE', #3787, #24651, #10897, .T. ) ;
#4698 = AXIS2_PLACEMENT_3D ( 'NONE', #21019, #36833, #8648 ) ;
#4699 = CARTESIAN_POINT ( 'NONE',  ( -0.1664683893528022818, 0.5171715631282262082, 0.3299773601679611978 ) ) ;
#4700 = ADVANCED_FACE ( 'NONE', ( #21498, #30926 ), #12220, .F. ) ;
#4701 = CARTESIAN_POINT ( 'NONE',  ( 0.2565305817069650218, -1.011710961920390339, 0.5944358237650989585 ) ) ;
#4702 = CIRCLE ( 'NONE', #11948, 0.01000000000000002970 ) ;
#4703 = DIRECTION ( 'NONE',  ( -1.000000000000000000, -0.000000000000000000, -0.000000000000000000 ) ) ;
#4704 = EDGE_CURVE ( 'NONE', #27529, #2400, #27987, .T. ) ;
#4705 = AXIS2_PLACEMENT_3D ( 'NONE', #1777, #35472, #17587 ) ;
#4706 = DIRECTION ( 'NONE',  ( -1.000000000000000000, -2.280301054154495132E-31, 1.664003471950577689E-31 ) ) ;
#4707 = DIRECTION ( 'NONE',  ( 1.000000000000000000, 0.000000000000000000, 0.000000000000000000 ) ) ;
#4708 = DIRECTION ( 'NONE',  ( 0.7956551220374312727, 0.4593167559955310120, -0.3949190352937456128 ) ) ;
#4709 = CIRCLE ( 'NONE', #804, 0.03999999999999933470 ) ;
#4710 = CARTESIAN_POINT ( 'NONE',  ( 0.3959476892382831625, -1.138264379635865353, 0.4306935340366444542 ) ) ;
#4711 = CARTESIAN_POINT ( 'NONE',  ( 0.03113248654051816583, 0.000000000000000000, 0.000000000000000000 ) ) ;
#4712 = DIRECTION ( 'NONE',  ( 1.000000000000000000, 0.000000000000000000, 0.000000000000000000 ) ) ;
#4713 = ORIENTED_EDGE ( 'NONE', *, *, #28764, .F. ) ;
#4714 = CARTESIAN_POINT ( 'NONE',  ( 0.0003960311365576736739, -0.4455394904127599198, 0.08489233873622216431 ) ) ;
#4715 = CARTESIAN_POINT ( 'NONE',  ( 0.4080762053856966109, -1.743682602239191137, -0.5952039892428494516 ) ) ;
#4716 = CARTESIAN_POINT ( 'NONE',  ( 0.2503797518491029939, -1.479909065722671002, 1.008170915534915446 ) ) ;
#4717 = DIRECTION ( 'NONE',  ( -9.106159978880870295E-15, 1.000000000000000000, -2.845674993400271967E-15 ) ) ;
#4718 = ORIENTED_EDGE ( 'NONE', *, *, #30275, .F. ) ;
#4719 = ORIENTED_EDGE ( 'NONE', *, *, #17641, .F. ) ;
#4720 = CARTESIAN_POINT ( 'NONE',  ( 0.1872789457748890163, -0.5068293638037115745, 0.1231878790029107551 ) ) ;
#4721 = VERTEX_POINT ( 'NONE', #33822 ) ;
#4722 = CARTESIAN_POINT ( 'NONE',  ( 0.4514031511399141383, -1.667537665946740466, -0.4121731472126302642 ) ) ;
#4723 = AXIS2_PLACEMENT_3D ( 'NONE', #2408, #30780, #30977 ) ;
#4724 = ADVANCED_FACE ( 'NONE', ( #8509 ), #37122, .T. ) ;
#4725 = CARTESIAN_POINT ( 'NONE',  ( 0.1348549594756915104, -0.5515731166344398639, 0.1532284265886467711 ) ) ;
#4727 = ORIENTED_EDGE ( 'NONE', *, *, #28356, .T. ) ;
#4726 = CARTESIAN_POINT ( 'NONE',  ( 0.006625058703027312222, -0.8256683006665239688, 0.06834504167984893630 ) ) ;
#4728 = EDGE_CURVE ( 'NONE', #13190, #17955, #27351, .T. ) ;
#4729 = ORIENTED_EDGE ( 'NONE', *, *, #35628, .T. ) ;
#4730 = CARTESIAN_POINT ( 'NONE',  ( 0.3097869260829022031, -1.188640176377027791, 0.4996798932217296763 ) ) ;
#4731 = AXIS2_PLACEMENT_3D ( 'NONE', #34364, #18951, #34156 ) ;
#4732 = CARTESIAN_POINT ( 'NONE',  ( 0.08271634070018635265, -1.004823404736711501, 0.8361326721138350182 ) ) ;
#4734 = CARTESIAN_POINT ( 'NONE',  ( 0.1922398268636369700, -1.242606702096344051, 0.6043157665294947023 ) ) ;
#4733 = CARTESIAN_POINT ( 'NONE',  ( -0.01548846960712817709, -0.4730347584885852830, -0.2341461249029094249 ) ) ;
#4735 = CARTESIAN_POINT ( 'NONE',  ( 7.512581982576723358E-16, 0.3059742766594581997, -3.756290991288361679E-16 ) ) ;
#4736 = AXIS2_PLACEMENT_3D ( 'NONE', #26213, #38736, #10560 ) ;
#4737 = DIRECTION ( 'NONE',  ( 0.8660512985181132439, 0.4999551463232376758, 0.000000000000000000 ) ) ;
#4739 = ORIENTED_EDGE ( 'NONE', *, *, #35065, .T. ) ;
#4738 = ORIENTED_EDGE ( 'NONE', *, *, #5886, .F. ) ;
#4740 = CARTESIAN_POINT ( 'NONE',  ( 0.08647094942830720055, -0.8134528749729150743, 0.2066784198371740267 ) ) ;
#4741 = FACE_OUTER_BOUND ( 'NONE', #9197, .T. ) ;
#4742 = CARTESIAN_POINT ( 'NONE',  ( 0.09091041988698707332, -0.5766203509326254251, 0.2109086659841546418 ) ) ;
#4743 = CARTESIAN_POINT ( 'NONE',  ( 0.1978543033782794447, -0.8340884217837519765, 0.6564551516366390338 ) ) ;
#4744 = DIRECTION ( 'NONE',  ( 0.000000000000000000, 0.000000000000000000, -1.000000000000000000 ) ) ;
#4745 = DIRECTION ( 'NONE',  ( 0.000000000000000000, 0.000000000000000000, -1.000000000000000000 ) ) ;
#4746 = CARTESIAN_POINT ( 'NONE',  ( -0.02000000000000000042, -1.906060000575976021, -0.2916525572568466340 ) ) ;
#4747 = CARTESIAN_POINT ( 'NONE',  ( 0.4203826191882746866, -1.700944664958486507, -0.4172566670736500560 ) ) ;
#4748 = CARTESIAN_POINT ( 'NONE',  ( 0.4342601836552755223, -1.675175375883231954, -0.4163388096883527956 ) ) ;
#4749 = CARTESIAN_POINT ( 'NONE',  ( 0.5437751503972781952, -1.596066189530210178, -0.5599633018817742336 ) ) ;
#4750 = FACE_BOUND ( 'NONE', #27004, .T. ) ;
#4751 = CARTESIAN_POINT ( 'NONE',  ( 0.1997919287435963309, -2.061796588699760235, -0.2711072614840514539 ) ) ;
#4752 = CARTESIAN_POINT ( 'NONE',  ( -7.828841584765314999E-06, -0.8039854292597425900, -0.08783247702100009657 ) ) ;
#4753 = CARTESIAN_POINT ( 'NONE',  ( 0.06995977277154606655, -0.5495845434848062316, 0.2074071626960130033 ) ) ;
#4754 = CIRCLE ( 'NONE', #34342, 0.009999999999999995004 ) ;
#4755 = CARTESIAN_POINT ( 'NONE',  ( 0.4090604450045443596, -1.131420581850358653, 0.3667417262808778666 ) ) ;
#4756 = CARTESIAN_POINT ( 'NONE',  ( 0.4511668698691139179, -1.684167190675012415, -0.3144976166544468099 ) ) ;
#4757 = CARTESIAN_POINT ( 'NONE',  ( 0.1872829031602858685, -1.532932250049839906, 0.6789365607098191147 ) ) ;
#4758 = CARTESIAN_POINT ( 'NONE',  ( 0.1920143701880955289, -0.8743002769911518701, 0.2704752137325454608 ) ) ;
#4759 = CALENDAR_DATE ( 2026, 13, 10 ) ;
#4760 = AXIS2_PLACEMENT_3D ( 'NONE', #29379, #17222, #29773 ) ;
#4761 = CARTESIAN_POINT ( 'NONE',  ( 0.1927581100858387075, -0.5042345029781482024, 0.3213135115051561908 ) ) ;
#4762 = AXIS2_PLACEMENT_3D ( 'NONE', #13083, #4221, #13282 ) ;
#4763 = AXIS2_PLACEMENT_3D ( 'NONE', #1647, #7784, #20353 ) ;
#4764 = CARTESIAN_POINT ( 'NONE',  ( 0.4139909421053795113, -1.650376109496379140, -0.6250900372738893429 ) ) ;
#4765 = CARTESIAN_POINT ( 'NONE',  ( -0.2746410161513782033, -2.461298705151934829, -0.7594706439553173816 ) ) ;
#4766 = AXIS2_PLACEMENT_3D ( 'NONE', #8258, #37047, #14627 ) ;
#4767 = VERTEX_POINT ( 'NONE', #15090 ) ;
#4768 = FACE_OUTER_BOUND ( 'NONE', #10949, .T. ) ;
#4769 = CARTESIAN_POINT ( 'NONE',  ( 0.1098459896970112454, -1.084708748088091923, 0.8887398936019613727 ) ) ;
#4770 = CARTESIAN_POINT ( 'NONE',  ( 0.1810483112700702890, -1.250999180832525148, 0.4405424963560370943 ) ) ;
#4772 = ORIENTED_EDGE ( 'NONE', *, *, #31535, .F. ) ;
#4771 = CARTESIAN_POINT ( 'NONE',  ( 0.1316017208954911588, -1.248059642665102942, 0.5182417262812423209 ) ) ;
#4773 = CARTESIAN_POINT ( 'NONE',  ( 0.3853411735687863326, -1.756807109041631509, -0.4499573014711771846 ) ) ;
#4774 = CARTESIAN_POINT ( 'NONE',  ( 0.5536319580448211264, -1.193555294463456873, 0.7337749688435845075 ) ) ;
#4776 = ORIENTED_EDGE ( 'NONE', *, *, #5769, .F. ) ;
#4775 = EDGE_LOOP ( 'NONE', ( #22036, #2139, #9198, #29754 ) ) ;
#4777 = CARTESIAN_POINT ( 'NONE',  ( 0.1263619274532199466, -1.314871306717832367, -0.7136791684005103775 ) ) ;
#4778 =( BOUNDED_SURFACE ( )  B_SPLINE_SURFACE ( 3, 2, ( 
 ( #36647, #23912, #11950 ),
 ( #1903, #27592, #27798 ),
 ( #11750, #33347, #8255 ),
 ( #33154, #24514, #14415 ) ),
 .UNSPECIFIED., .F., .F., .T. ) 
 B_SPLINE_SURFACE_WITH_KNOTS ( ( 4, 4 ),
 ( 3, 3 ),
 ( 0.000000000000000000, 0.0002728543041759452824 ),
 ( 0.000000000000000000, 1.000000000000000000 ),
 .UNSPECIFIED. ) 
 GEOMETRIC_REPRESENTATION_ITEM ( )  RATIONAL_B_SPLINE_SURFACE ( (
 ( 1.000000000000000000, 0.7071067811865477948, 1.000000000000000000),
 ( 1.000000000000000000, 0.7071067862473439103, 1.000000000000000000),
 ( 1.000000000000000000, 0.7071227907078153629, 1.000000000000000000),
 ( 1.000000000000000000, 0.7071530416912256145, 1.000000000000000000) ) ) 
 REPRESENTATION_ITEM ( '' )  SURFACE ( )  );
#4779 = CARTESIAN_POINT ( 'NONE',  ( 0.05561170715395058473, -0.02038383341412211558, -0.4604752114371308824 ) ) ;
#4780 = DIRECTION ( 'NONE',  ( 0.2828184691483945357, -0.9591734532964090176, 3.801289047037795017E-15 ) ) ;
#4781 = CALENDAR_DATE ( 2026, 13, 10 ) ;
#4782 = CIRCLE ( 'NONE', #9373, 0.06819284191469469902 ) ;
#4783 = CARTESIAN_POINT ( 'NONE',  ( -0.05281452789367998418, 0.4315450824722493750, -0.1820506770215899739 ) ) ;
#4784 = EDGE_LOOP ( 'NONE', ( #32565, #38993, #28436, #17890, #26695, #27473 ) ) ;
#4785 = CARTESIAN_POINT ( 'NONE',  ( 0.08016251834805442067, -1.309203902574839207, 0.5631135398343307674 ) ) ;
#4786 = CARTESIAN_POINT ( 'NONE',  ( 0.1623264987558849792, -0.8004081683446899742, 0.5646416967012523047 ) ) ;
#4787 = CIRCLE ( 'NONE', #23885, 0.1749999999999999889 ) ;
#4788 = CARTESIAN_POINT ( 'NONE',  ( 0.2663090763754291657, -1.538339113173472716, 0.9867693543954003665 ) ) ;
#4789 = AXIS2_PLACEMENT_3D ( 'NONE', #8567, #5272, #40042 ) ;
#4790 = CARTESIAN_POINT ( 'NONE',  ( 0.09796691250624214864, -0.5532864700090758259, 0.2008629083371975543 ) ) ;
#4792 = DIRECTION ( 'NONE',  ( -0.4686504021719342661, -0.2705430738262412649, -0.8409359343902087502 ) ) ;
#4791 = CARTESIAN_POINT ( 'NONE',  ( 0.1133176935271576757, -0.6554924552526250059, -0.09368704978610124801 ) ) ;
#4793 = CARTESIAN_POINT ( 'NONE',  ( 0.1596048412419493190, -1.234437691115734870, 0.6299358457907016096 ) ) ;
#4794 = ORIENTED_EDGE ( 'NONE', *, *, #22222, .F. ) ;
#4795 = ORIENTED_EDGE ( 'NONE', *, *, #35631, .T. ) ;
#4796 = CARTESIAN_POINT ( 'NONE',  ( -0.02000000000000000042, -2.183180860297908144, -0.4937760292030871079 ) ) ;
#4797 = CARTESIAN_POINT ( 'NONE',  ( 0.1541907618229372834, -0.5976806583976911336, 0.5269747745306871956 ) ) ;
#4798 = CIRCLE ( 'NONE', #348, 0.03749999999977545601 ) ;
#4799 = CARTESIAN_POINT ( 'NONE',  ( -2.359223927328458141E-16, 1.120325691531921079E-16, -0.1699999999999995404 ) ) ;
#4800 = CARTESIAN_POINT ( 'NONE',  ( -0.05252359774140240994, -0.4488292542424489051, -0.1363200544095012345 ) ) ;
#4801 = CARTESIAN_POINT ( 'NONE',  ( 0.07006815180907459417, -1.315301596572421294, 0.5080907171457548221 ) ) ;
#4802 = CARTESIAN_POINT ( 'NONE',  ( 0.1716982692503948582, -1.801629902383738324, -0.6814167475625579895 ) ) ;
#4803 = CARTESIAN_POINT ( 'NONE',  ( -0.2900000000000005351, 0.5182417262804733804, 0.3750000000000000555 ) ) ;
#4804 = CARTESIAN_POINT ( 'NONE',  ( 0.5675876754196318430, -1.214623637701154335, 0.7236292717493534310 ) ) ;
#4805 = CARTESIAN_POINT ( 'NONE',  ( 0.3699999999999786793, -2.097675824466503691, -0.5027161252448985040 ) ) ;
#4806 = CIRCLE ( 'NONE', #1563, 0.05000000000000000971 ) ;
#4807 = CARTESIAN_POINT ( 'NONE',  ( 0.1308641205180471057, -1.355064818086789025, -0.3217643887045131268 ) ) ;
#4808 = CARTESIAN_POINT ( 'NONE',  ( 0.4853385542066005476, -1.649621470899823583, -0.6309284955820858576 ) ) ;
#4809 = VERTEX_POINT ( 'NONE', #31146 ) ;
#4810 = CARTESIAN_POINT ( 'NONE',  ( 0.4534739523000680950, -1.220957794426671406, -0.5155029497116575543 ) ) ;
#4811 = DIRECTION ( 'NONE',  ( -0.4999551463232373427, 0.8660512985181134660, -0.000000000000000000 ) ) ;
#4812 = DIRECTION ( 'NONE',  ( -1.000000000000000000, -0.000000000000000000, -0.000000000000000000 ) ) ;
#4813 = CIRCLE ( 'NONE', #19332, 0.009999999999999995004 ) ;
#4814 = AXIS2_PLACEMENT_3D ( 'NONE', #11873, #39866, #9190 ) ;
#4815 = EDGE_LOOP ( 'NONE', ( #40479, #39370, #37854, #24595, #6464 ) ) ;
#4816 = CARTESIAN_POINT ( 'NONE',  ( 0.5005350806643109607, -1.112410049453316008, 0.6916867713706035259 ) ) ;
#4817 = CARTESIAN_POINT ( 'NONE',  ( 0.5106109609909708080, -1.176845144576392332, 0.4435443120481467050 ) ) ;
#4818 = CYLINDRICAL_SURFACE ( 'NONE', #18672, 0.02999999999999998848 ) ;
#4819 = MANIFOLD_SOLID_BREP ( 'Chamfer1', #31915 ) ;
#4820 = CONICAL_SURFACE ( 'NONE', #19948, 0.3698489655878005045, 1.211529128687673262 ) ;
#4821 = CARTESIAN_POINT ( 'NONE',  ( 0.04038401875063166863, -0.8587749605274695996, 0.3937922782597925164 ) ) ;
#4822 = ORIENTED_EDGE ( 'NONE', *, *, #27778, .F. ) ;
#4823 = CARTESIAN_POINT ( 'NONE',  ( -0.01548846960712763066, 0.2450655194479529619, 0.4674710490748108516 ) ) ;
#4824 = CIRCLE ( 'NONE', #22614, 0.04999999999999998890 ) ;
#4825 = CARTESIAN_POINT ( 'NONE',  ( 0.02872242845530406652, 0.07817994906157187118, 0.5268390348591149852 ) ) ;
#4826 = CARTESIAN_POINT ( 'NONE',  ( 0.1443375672974070711, 0.05141091571461162829, 0.000000000000000000 ) ) ;
#4827 = APPROVAL ( #38190, 'UNSPECIFIED' ) ;
#4828 = CARTESIAN_POINT ( 'NONE',  ( 0.1993125180077263137, -2.032910743388167685, -0.2793764414722799683 ) ) ;
#4829 = CARTESIAN_POINT ( 'NONE',  ( 0.4321750792481709458, -1.187405343333139296, 0.6822186175578013323 ) ) ;
#4831 = CARTESIAN_POINT ( 'NONE',  ( 0.4964355788048083751, -1.123423484656395299, 0.5685061009866244630 ) ) ;
#4830 = CARTESIAN_POINT ( 'NONE',  ( 0.000000000000000000, 0.8492681979939306069, -0.2138253033704805295 ) ) ;
#4832 = B_SPLINE_CURVE_WITH_KNOTS ( 'NONE', 3,
 ( #5714, #12858, #2031, #37951, #15172, #40266, #24061, #30815, #2636, #27731, #10785, #32172, #35877, #4191, #22531, #38342, #29088, #563 ),
 .UNSPECIFIED., .F., .F.,
 ( 4, 2, 2, 2, 2, 2, 2, 2, 4 ),
 ( 0.000000000000000000, 0.0007927102992442323307, 0.001585420598488464661, 0.002378130897732695908, 0.003170841196976927588, 0.003963551496221159702, 0.004756261795465391816, 0.005548972094709624797, 0.006341682393953856911 ),
 .UNSPECIFIED. ) ;
#4833 = CARTESIAN_POINT ( 'NONE',  ( 0.5816004637761955642, -1.517907389782662042, -0.4510474287064656918 ) ) ;
#4834 = ORIENTED_EDGE ( 'NONE', *, *, #5360, .F. ) ;
#4835 = FACE_OUTER_BOUND ( 'NONE', #14296, .T. ) ;
#4836 = VERTEX_POINT ( 'NONE', #33408 ) ;
#4837 = CYLINDRICAL_SURFACE ( 'NONE', #14106, 0.1033070866141732880 ) ;
#4838 = CARTESIAN_POINT ( 'NONE',  ( 0.07344452620781788399, -0.6304810646442478017, 0.4078118883576473674 ) ) ;
#4840 = FACE_OUTER_BOUND ( 'NONE', #17506, .T. ) ;
#4839 = CARTESIAN_POINT ( 'NONE',  ( 0.08956013910934083888, -0.5501150684396665103, 0.1018409378312434832 ) ) ;
#4841 = CARTESIAN_POINT ( 'NONE',  ( 0.2611244543265801576, -0.7808929225949666764, 0.1477649966949237115 ) ) ;
#4842 = ORIENTED_EDGE ( 'NONE', *, *, #37818, .T. ) ;
#4843 = AXIS2_PLACEMENT_3D ( 'NONE', #35315, #20098, #6707 ) ;
#4844 = CARTESIAN_POINT ( 'NONE',  ( -0.01548846960707545191, -0.5198120922912057296, -0.07362328916749273644 ) ) ;
#4845 = CARTESIAN_POINT ( 'NONE',  ( 0.3863603026027747078, -1.188791174525776650, 0.8283360454836284914 ) ) ;
#4846 = ORIENTED_EDGE ( 'NONE', *, *, #10472, .T. ) ;
#4847 = CARTESIAN_POINT ( 'NONE',  ( -0.2746410161513782033, -2.407646569606659792, -0.8438593182631384249 ) ) ;
#4848 = CARTESIAN_POINT ( 'NONE',  ( -0.08000000000000000167, -2.183180860297908144, -0.4937760292030871079 ) ) ;
#4849 = CIRCLE ( 'NONE', #29184, 0.08249999999977548903 ) ;
#4850 = AXIS2_PLACEMENT_3D ( 'NONE', #14312, #32630, #17607 ) ;
#4851 = EDGE_CURVE ( 'NONE', #858, #29150, #8983, .T. ) ;
#4852 = CARTESIAN_POINT ( 'NONE',  ( 0.3720910755108596812, -1.764456141754468188, -0.4343423851154138982 ) ) ;
#4853 = PRODUCT ( 'Parallelogram front_FRONT', 'Parallelogram front_FRONT', '', ( #18344 ) ) ;
#4854 = CARTESIAN_POINT ( 'NONE',  ( 0.1847208729320930221, -1.260429531918160206, 0.4290398900403852855 ) ) ;
#4855 = CARTESIAN_POINT ( 'NONE',  ( 0.3957353887311833018, -1.753985813695325247, -0.5139772769213331038 ) ) ;
#4856 = CARTESIAN_POINT ( 'NONE',  ( 2.048885995248197414E-16, 0.2900000000000004796, -5.122214988120493288E-16 ) ) ;
#4857 = AXIS2_PLACEMENT_3D ( 'NONE', #2796, #29815, #1655 ) ;
#4858 = CARTESIAN_POINT ( 'NONE',  ( 0.2506904587504640847, -0.6594178163634784040, 0.5852584525479398447 ) ) ;
#4859 = EDGE_CURVE ( 'NONE', #32251, #39497, #10439, .T. ) ;
#4860 = AXIS2_PLACEMENT_3D ( 'NONE', #26335, #17272, #13973 ) ;
#4861 = CARTESIAN_POINT ( 'NONE',  ( 0.07670268886588108015, -1.321079536449508485, 0.4808101794164899578 ) ) ;
#4862 = DIRECTION ( 'NONE',  ( 0.000000000000000000, 0.000000000000000000, -1.000000000000000000 ) ) ;
#4863 = ADVANCED_FACE ( 'NONE', ( #2153 ), #36701, .T. ) ;
#4864 = EDGE_CURVE ( 'NONE', #5616, #25917, #11572, .T. ) ;
#4865 = CARTESIAN_POINT ( 'NONE',  ( 0.5839561686609843205, -1.602591383399306624, -0.5767004275490535958 ) ) ;
#4866 = CARTESIAN_POINT ( 'NONE',  ( -2.070754768975505034, -0.09959325338431362917, 0.08499999999999909017 ) ) ;
#4867 = CARTESIAN_POINT ( 'NONE',  ( 0.5832107232896035498, -1.609297431860164496, 0.5795114931753430065 ) ) ;
#4868 = EDGE_CURVE ( 'NONE', #36928, #2775, #20287, .T. ) ;
#4869 = CARTESIAN_POINT ( 'NONE',  ( -0.2789010053595599725, 0.4834754829570387935, 0.1000000000000000194 ) ) ;
#4870 = CARTESIAN_POINT ( 'NONE',  ( -0.1044460467970230316, -0.4741855622371820567, 0.3602693341844401265 ) ) ;
#4871 = CARTESIAN_POINT ( 'NONE',  ( 0.02385183771220368218, -0.6100559285722760849, 0.5958381505304063408 ) ) ;
#4872 = CARTESIAN_POINT ( 'NONE',  ( 0.5856933011632973196, -1.570058762653790518, -0.5108706408130125887 ) ) ;
#4873 = CARTESIAN_POINT ( 'NONE',  ( -1.496393162519624559E-15, 3.328006943901148699E-32, -0.05000000000000002359 ) ) ;
#4874 = DIRECTION ( 'NONE',  ( 0.8660512985181135770, 0.4999551463232371762, 0.000000000000000000 ) ) ;
#4875 = CARTESIAN_POINT ( 'NONE',  ( -0.04211471441534175852, -0.2826022563026960310, 0.3743350969764960845 ) ) ;
#4876 = AXIS2_PLACEMENT_3D ( 'NONE', #40067, #11896, #33928 ) ;
#4877 = ORIENTED_EDGE ( 'NONE', *, *, #21085, .T. ) ;
#4878 = CIRCLE ( 'NONE', #27906, 0.01500000000000000291 ) ;
#4879 = VERTEX_POINT ( 'NONE', #12412 ) ;
#4880 = DIRECTION ( 'NONE',  ( 1.000000000000000000, 0.000000000000000000, 0.000000000000000000 ) ) ;
#4881 = AXIS2_PLACEMENT_3D ( 'NONE', #37993, #22185, #19490 ) ;
#4882 = ADVANCED_FACE ( 'NONE', ( #34632 ), #111, .T. ) ;
#4883 = CARTESIAN_POINT ( 'NONE',  ( 0.05563540667800927902, -1.335270441939011121, 0.5197417262808780025 ) ) ;
#4884 = VERTEX_POINT ( 'NONE', #16130 ) ;
#4885 = AXIS2_PLACEMENT_3D ( 'NONE', #6789, #28623, #3726 ) ;
#4886 = DIRECTION ( 'NONE',  ( 8.881784197001246407E-16, -2.361472542561082612E-16, 1.000000000000000000 ) ) ;
#4887 = APPLIED_PERSON_AND_ORGANIZATION_ASSIGNMENT ( #1082, #873, ( #4217 ) ) ;
#4888 = CARTESIAN_POINT ( 'NONE',  ( -0.05634301242525835418, 0.2614060064472178424, -0.3772872482281192652 ) ) ;
#4889 = CARTESIAN_POINT ( 'NONE',  ( 0.4377275372045464352, -1.201128267441582187, 0.7458237077910447876 ) ) ;
#4891 = VERTEX_POINT ( 'NONE', #6624 ) ;
#4890 = CARTESIAN_POINT ( 'NONE',  ( -0.1659602879904918671, 0.5155992160893299037, 0.1238948718127771270 ) ) ;
#4892 = CARTESIAN_POINT ( 'NONE',  ( 0.1845475678902450123, -0.7902170579836453879, 0.1696330687313138408 ) ) ;
#4893 = CIRCLE ( 'NONE', #27912, 0.03000000000000029379 ) ;
#4894 = DIRECTION ( 'NONE',  ( 0.000000000000000000, 0.000000000000000000, 1.000000000000000000 ) ) ;
#4895 = ORIENTED_EDGE ( 'NONE', *, *, #10016, .F. ) ;
#4896 = DIRECTION ( 'NONE',  ( 1.000000000000000000, 0.000000000000000000, 0.000000000000000000 ) ) ;
#4897 = CARTESIAN_POINT ( 'NONE',  ( 0.02354069309169367838, -0.5479244848632992548, 0.2301531253923031484 ) ) ;
#4899 = CARTESIAN_POINT ( 'NONE',  ( 0.1877532238556526289, -0.5410535477826009521, 0.06280118956074845493 ) ) ;
#4898 = CARTESIAN_POINT ( 'NONE',  ( 0.6910729260980184030, -1.496094287350760332, 0.4693483012025433943 ) ) ;
#4900 = CARTESIAN_POINT ( 'NONE',  ( 0.4094665197507286747, -1.132124008075320098, 0.5707417262808780478 ) ) ;
#4901 = DIRECTION ( 'NONE',  ( 0.8660512985181133550, 0.4999551463232372317, 0.000000000000000000 ) ) ;
#4902 = VERTEX_POINT ( 'NONE', #15700 ) ;
#4903 = MANIFOLD_SOLID_BREP ( 'Fillet7', #15507 ) ;
#4904 = CARTESIAN_POINT ( 'NONE',  ( 0.1636912256974782376, -1.272012149535565850, 0.4251003766563813402 ) ) ;
#4905 = DIRECTION ( 'NONE',  ( 1.000000000000000000, 0.000000000000000000, 0.000000000000000000 ) ) ;
#4906 = CARTESIAN_POINT ( 'NONE',  ( 0.2747206457212271746, -1.194764396915172444, 0.7305384998433399613 ) ) ;
#4907 = CARTESIAN_POINT ( 'NONE',  ( 0.1870397359536237203, -0.7179515242747687154, 0.07956602225022149644 ) ) ;
#4908 = VECTOR ( 'NONE', #2189, 39.37007874015748854 ) ;
#4909 = CARTESIAN_POINT ( 'NONE',  ( 0.01548846960721238578, 0.5203207976464816475, -0.08861466064783077301 ) ) ;
#4910 = VECTOR ( 'NONE', #32991, 39.37007874015748143 ) ;
#4911 = CIRCLE ( 'NONE', #15452, 0.02999999999999997460 ) ;
#4912 = DIRECTION ( 'NONE',  ( 0.000000000000000000, 0.000000000000000000, 1.000000000000000000 ) ) ;
#4913 = EDGE_CURVE ( 'NONE', #12108, #11891, #3026, .T. ) ;
#4914 = CARTESIAN_POINT ( 'NONE',  ( -0.3000000000000000999, -3.941790907013290823, -0.4709369376873030477 ) ) ;
#4915 = CARTESIAN_POINT ( 'NONE',  ( 0.02953079040095728247, 0.000000000000000000, 0.000000000000000000 ) ) ;
#4916 = DIRECTION ( 'NONE',  ( -1.000000000000000000, 0.000000000000000000, 0.000000000000000000 ) ) ;
#4917 = CARTESIAN_POINT ( 'NONE',  ( 0.3186320389496528627, -1.760431904683431359, 0.5682417262808792113 ) ) ;
#4918 = DATE_AND_TIME ( #20579, #18057 ) ;
#4919 = APPROVAL_PERSON_ORGANIZATION ( #26112, #31795, #13920 ) ;
#4920 = EDGE_CURVE ( 'NONE', #9996, #11394, #31916, .T. ) ;
#4921 = CARTESIAN_POINT ( 'NONE',  ( 0.3880322814406260701, -1.147921704116221298, 0.4309387522554056216 ) ) ;
#4922 = EDGE_CURVE ( 'NONE', #24814, #26475, #28247, .T. ) ;
#4923 = CARTESIAN_POINT ( 'NONE',  ( 0.03159140494779937719, -0.4482517543799813264, 0.2030416442520436293 ) ) ;
#4924 = VECTOR ( 'NONE', #24027, 39.37007874015748854 ) ;
#4925 = CARTESIAN_POINT ( 'NONE',  ( 0.6430098986722891929, -1.590739804012314185, -0.4546931408925402041 ) ) ;
#4926 = CARTESIAN_POINT ( 'NONE',  ( 0.01217710773476333823, -0.4281249367976072140, 0.1335689301494157322 ) ) ;
#4927 = CARTESIAN_POINT ( 'NONE',  ( 0.3576546886276804615, -1.772789996722293537, -0.5848438031758242950 ) ) ;
#4928 = CARTESIAN_POINT ( 'NONE',  ( 0.2559395560537573444, -1.500125191510220279, 1.001930765150525593 ) ) ;
#4929 = CARTESIAN_POINT ( 'NONE',  ( 0.04155248107635944876, 0.01723053523177107277, -0.4699878081388669804 ) ) ;
#4930 = ORIENTED_EDGE ( 'NONE', *, *, #36054, .T. ) ;
#4931 = VERTEX_POINT ( 'NONE', #3955 ) ;
#4932 = EDGE_CURVE ( 'NONE', #4246, #18554, #24962, .T. ) ;
#4933 = DIRECTION ( 'NONE',  ( -1.000000000000000000, -2.280301054154495132E-31, 1.664003471950577689E-31 ) ) ;
#4934 = ORIENTED_EDGE ( 'NONE', *, *, #18563, .T. ) ;
#4935 = CARTESIAN_POINT ( 'NONE',  ( -0.2399999999999999079, -3.061672939615505573, -1.351054905085088409 ) ) ;
#4936 = AXIS2_PLACEMENT_3D ( 'NONE', #6271, #6466, #24608 ) ;
#4938 = ORIENTED_EDGE ( 'NONE', *, *, #18179, .T. ) ;
#4937 = CARTESIAN_POINT ( 'NONE',  ( 0.4380679180091197611, -1.234484979903685664, 0.8225911399008282165 ) ) ;
#4940 = VERTEX_POINT ( 'NONE', #28450 ) ;
#4939 = CARTESIAN_POINT ( 'NONE',  ( 9.509834983668487914E-05, -0.6764735018835020819, -0.02209724360191241826 ) ) ;
#4941 = AXIS2_PLACEMENT_3D ( 'NONE', #2805, #8766, #33880 ) ;
#4942 = EDGE_LOOP ( 'NONE', ( #14318, #27837, #27032, #28634 ) ) ;
#4943 = CARTESIAN_POINT ( 'NONE',  ( 0.4411887824651631873, -1.114744685954409009, 0.8907908412112590657 ) ) ;
#4944 = ORIENTED_EDGE ( 'NONE', *, *, #32611, .F. ) ;
#4945 = CARTESIAN_POINT ( 'NONE',  ( -0.01402042477169951340, -0.5319719165593393972, 0.1980928424870210536 ) ) ;
#4947 = CARTESIAN_POINT ( 'NONE',  ( 0.2151567955658992837, -1.242576477413985137, 0.5631370738156890043 ) ) ;
#4946 = CARTESIAN_POINT ( 'NONE',  ( -0.2746410161513782033, -1.906460133321048911, -0.3231213194042100723 ) ) ;
#4948 = APPROVAL_PERSON_ORGANIZATION ( #28251, #33271, #22922 ) ;
#4949 = CARTESIAN_POINT ( 'NONE',  ( 0.6353491899451704228, -1.612482177454656496, -0.4775148252911664004 ) ) ;
#4950 = COORDINATED_UNIVERSAL_TIME_OFFSET ( 0, 0, .AHEAD. ) ;
#4951 = CARTESIAN_POINT ( 'NONE',  ( -0.1655857493438344097, 0.4810233835288787452, 0.3340284351899789894 ) ) ;
#4953 = ORIENTED_EDGE ( 'NONE', *, *, #201, .F. ) ;
#4952 = VERTEX_POINT ( 'NONE', #19417 ) ;
#4954 = CARTESIAN_POINT ( 'NONE',  ( 0.01135461203890102133, -0.9395716130340400207, 0.08695101789951617532 ) ) ;
#4955 = AXIS2_PLACEMENT_3D ( 'NONE', #7603, #35586, #10093 ) ;
#4956 = CARTESIAN_POINT ( 'NONE',  ( 0.1008930477423943123, -1.308833506382407474, 0.7266393657083966007 ) ) ;
#4957 = CARTESIAN_POINT ( 'NONE',  ( 0.1493143905638315838, -0.7774743300093324150, 0.6049429375722679136 ) ) ;
#4958 = CARTESIAN_POINT ( 'NONE',  ( 0.1171945479475617752, -0.6032665890832976663, 0.3311638906348050582 ) ) ;
#4959 = CARTESIAN_POINT ( 'NONE',  ( 0.1824040550974478092, -0.5173104186764061474, 0.2535968541610654214 ) ) ;
#4960 = CARTESIAN_POINT ( 'NONE',  ( -0.05464101615137761936, -2.058305985490972212, -0.5970033804171128722 ) ) ;
#4961 = CARTESIAN_POINT ( 'NONE',  ( 0.06874771606299766302, -1.327481140994086317, 0.5533907816784044975 ) ) ;
#4962 = CARTESIAN_POINT ( 'NONE',  ( 0.3713793989799819562, -1.734397752681366534, -0.4210101696510674119 ) ) ;
#4963 = CARTESIAN_POINT ( 'NONE',  ( 0.1876053338355621880, -0.6785855078148245179, 0.1477569985384105666 ) ) ;
#4964 = CARTESIAN_POINT ( 'NONE',  ( 0.3766924275363039976, -1.659541107949447980, -0.6295622186357943129 ) ) ;
#4965 = CARTESIAN_POINT ( 'NONE',  ( 0.3699999999982759302, -2.089770822019046292, -0.2936553927183578883 ) ) ;
#4966 = CARTESIAN_POINT ( 'NONE',  ( -0.01548846960707517956, -0.09061086148575756005, -0.5171215251571035232 ) ) ;
#4967 = CARTESIAN_POINT ( 'NONE',  ( 0.4599911587916594713, -1.116015572881478679, 0.5707053994389698071 ) ) ;
#4968 = CARTESIAN_POINT ( 'NONE',  ( 0.3569552165733603233, -1.627031886803703919, -0.3705999156339398470 ) ) ;
#4969 = EDGE_CURVE ( 'NONE', #30248, #26219, #12608, .T. ) ;
#4970 = TOROIDAL_SURFACE ( 'NONE', #33886, 0.04500000000000032446, 0.01499999999999999944 ) ;
#4971 = AXIS2_PLACEMENT_3D ( 'NONE', #6022, #24573, #8316 ) ;
#4972 = CARTESIAN_POINT ( 'NONE',  ( 0.6301045230376582928, -1.599306761647289354, -0.4491897841421867987 ) ) ;
#4973 = CARTESIAN_POINT ( 'NONE',  ( 0.1721302213443809126, -1.453494483496651890, 0.7931418093652549128 ) ) ;
#4974 = CARTESIAN_POINT ( 'NONE',  ( 0.3877041582795131003, -1.010062466692070560, 0.6423187497268529889 ) ) ;
#4975 = COORDINATED_UNIVERSAL_TIME_OFFSET ( 0, 0, .AHEAD. ) ;
#4976 = CARTESIAN_POINT ( 'NONE',  ( 0.7110566119663160878, -1.453354452021889731, 0.7718588955819412067 ) ) ;
#4977 = LOCAL_TIME ( 0, 53, 7.000000000000000000, #6509 ) ;
#4978 = FACE_OUTER_BOUND ( 'NONE', #39219, .T. ) ;
#4979 = VECTOR ( 'NONE', #29168, 39.37007874015748854 ) ;
#4980 = CARTESIAN_POINT ( 'NONE',  ( 0.02242828275838999394, 0.06992002095335812795, -0.5075510395145109710 ) ) ;
#4981 = VERTEX_POINT ( 'NONE', #22500 ) ;
#4982 = CARTESIAN_POINT ( 'NONE',  ( 0.4184753273149497965, -1.633759443312357007, -0.5155029497116575543 ) ) ;
#4983 = CARTESIAN_POINT ( 'NONE',  ( 0.02977258242336560182, -0.7570884278691590863, 0.6213445499472508571 ) ) ;
#4984 = ADVANCED_FACE ( 'NONE', ( #35026 ), #836, .T. ) ;
#4985 = APPLIED_DATE_AND_TIME_ASSIGNMENT ( #28230, #22092, ( #14861 ) ) ;
#4986 = CARTESIAN_POINT ( 'NONE',  ( -0.09579104668929040722, -0.04310840302197994911, 0.3600000000000000422 ) ) ;
#4988 = ORIENTED_EDGE ( 'NONE', *, *, #15696, .T. ) ;
#4987 = CARTESIAN_POINT ( 'NONE',  ( 0.3885726445799232431, -1.811795032242741632, -0.5028984591946519256 ) ) ;
#4989 = EDGE_CURVE ( 'NONE', #19731, #26082, #24708, .T. ) ;
#4990 = CARTESIAN_POINT ( 'NONE',  ( 0.4961012839380697370, -1.676527870641093987, -0.4225323133350444849 ) ) ;
#4991 = CARTESIAN_POINT ( 'NONE',  ( 0.3319931610750171957, -0.8547376211461308326, 0.6892644829257473793 ) ) ;
#4993 = ORIENTED_EDGE ( 'NONE', *, *, #28289, .T. ) ;
#4992 = ORIENTED_EDGE ( 'NONE', *, *, #35400, .F. ) ;
#4994 = CARTESIAN_POINT ( 'NONE',  ( 0.09602014362969647776, -1.423132328501501620, -0.6903307521141727188 ) ) ;
#4995 = EDGE_CURVE ( 'NONE', #591, #36967, #23526, .T. ) ;
#4996 = CARTESIAN_POINT ( 'NONE',  ( -0.2399999999999999079, -3.985676108854518507, -0.7623095129438225426 ) ) ;
#4997 = CARTESIAN_POINT ( 'NONE',  ( 0.4670213778778394831, -1.236191465557153757, 0.6057417262809817737 ) ) ;
#4998 = COORDINATED_UNIVERSAL_TIME_OFFSET ( 0, 0, .AHEAD. ) ;
#4999 = DIRECTION ( 'NONE',  ( -0.4999551463232371762, 0.8660512985181134660, -0.000000000000000000 ) ) ;
#5000 = ORIENTED_EDGE ( 'NONE', *, *, #11727, .F. ) ;
#5001 = CARTESIAN_POINT ( 'NONE',  ( 0.1995529058109158649, -2.050896138459939344, -0.3054326997595754878 ) ) ;
#5002 = VECTOR ( 'NONE', #16868, 39.37007874015748143 ) ;
#5003 = CARTESIAN_POINT ( 'NONE',  ( 0.1740021755340503407, -0.8283876604043171055, 0.5873707361312400232 ) ) ;
#5004 = CARTESIAN_POINT ( 'NONE',  ( 0.3018042201724753237, -1.665203873072418794, 0.9047098497351133695 ) ) ;
#5005 = CARTESIAN_POINT ( 'NONE',  ( 0.1247534215796342189, -0.6769942796222839787, 0.4736701887020580704 ) ) ;
#5007 = CYLINDRICAL_SURFACE ( 'NONE', #14457, 0.06000000000000038636 ) ;
#5006 = CARTESIAN_POINT ( 'NONE',  ( 0.1150778763548105377, -0.4543190241136206842, 0.08302619808872485629 ) ) ;
#5008 = CARTESIAN_POINT ( 'NONE',  ( 0.09285408974215507427, -1.054165622298770089, 0.6121834013375294647 ) ) ;
#5009 = CARTESIAN_POINT ( 'NONE',  ( 0.3313632526110646959, -1.291506781903942302, 0.5682210202584868641 ) ) ;
#5010 = ORIENTED_EDGE ( 'NONE', *, *, #18967, .T. ) ;
#5011 = VERTEX_POINT ( 'NONE', #22918 ) ;
#5012 = DIRECTION ( 'NONE',  ( -1.000000000000000000, 7.000205099780406914E-17, 1.387778780781449620E-15 ) ) ;
#5013 = CARTESIAN_POINT ( 'NONE',  ( 0.1913351458898694402, -0.4849373758447458882, 0.2686262507137537336 ) ) ;
#5014 = AXIS2_PLACEMENT_3D ( 'NONE', #17772, #5222, #11203 ) ;
#5015 = DIRECTION ( 'NONE',  ( -1.000000000000000000, -2.280301054154495132E-31, 1.664003471950577689E-31 ) ) ;
#5016 = CARTESIAN_POINT ( 'NONE',  ( 0.03650581953630420429, -0.4542932396444889220, 0.2355374485430444531 ) ) ;
#5017 = CARTESIAN_POINT ( 'NONE',  ( -0.03647137243075312951, -0.5060707921514409069, -0.07645882641830938076 ) ) ;
#5018 = EDGE_CURVE ( 'NONE', #25046, #31057, #20773, .T. ) ;
#5019 = EDGE_CURVE ( 'NONE', #23130, #4242, #9590, .T. ) ;
#5020 = CARTESIAN_POINT ( 'NONE',  ( 0.07776798027987287532, -1.310857805500537543, 0.4781333465564954754 ) ) ;
#5021 = CARTESIAN_POINT ( 'NONE',  ( 0.1729041008443502614, -1.754908398349515952, -0.6809640004795894930 ) ) ;
#5022 = CARTESIAN_POINT ( 'NONE',  ( 0.1186006463096753172, -1.414144484500942989, 0.5682508211975187962 ) ) ;
#5023 = CARTESIAN_POINT ( 'NONE',  ( 0.6169573538504090626, -1.299218888095586388, 0.5469722621913530869 ) ) ;
#5024 = DIRECTION ( 'NONE',  ( -1.000000000000000000, -6.779273404243070203E-32, -4.314083075427408311E-32 ) ) ;
#5025 = CARTESIAN_POINT ( 'NONE',  ( 0.1815643315344221131, -1.297094087716649025, -0.2985759631856487739 ) ) ;
#5026 = CIRCLE ( 'NONE', #3727, 0.6115209409081865388 ) ;
#5027 = CARTESIAN_POINT ( 'NONE',  ( -0.02000000000000000042, -1.951160786456441754, -0.2520808614002822412 ) ) ;
#5028 = ORIENTED_EDGE ( 'NONE', *, *, #11433, .F. ) ;
#5029 = DIRECTION ( 'NONE',  ( -1.416619696839553536E-11, 0.9510565162951574170, 0.3090169943749355719 ) ) ;
#5030 = LINE ( 'NONE', #20691, #27781 ) ;
#5031 = CARTESIAN_POINT ( 'NONE',  ( -0.03874953289575396032, -0.2523958943867713467, -0.4040664878102112056 ) ) ;
#5032 =( BOUNDED_SURFACE ( )  B_SPLINE_SURFACE ( 3, 2, ( 
 ( #15340, #2792, #2398 ),
 ( #24998, #40218, #34460 ),
 ( #24818, #11838, #2587 ),
 ( #12053, #27896, #14936 ),
 ( #21327, #37149, #21716 ),
 ( #37530, #33864, #5667 ),
 ( #3193, #34249, #6274 ),
 ( #12261, #15733, #9354 ),
 ( #21534, #18222, #30769 ),
 ( #8961, #37340, #31389 ),
 ( #40434, #149, #5452 ),
 ( #12643, #15125, #34054 ),
 ( #9152, #6061, #18629 ),
 ( #31185, #28101, #3003 ) ),
 .UNSPECIFIED., .F., .F., .F. ) 
 B_SPLINE_SURFACE_WITH_KNOTS ( ( 4, 2, 2, 2, 2, 2, 4 ),
 ( 3, 3 ),
 ( 0.000000000000000000, 0.0009840465490818996620, 0.001476069823622849601, 0.001968093098163799324, 0.002460116372704749046, 0.002952139647245699203, 0.003936186196327598648 ),
 ( 0.000000000000000000, 1.000000000000000000 ),
 .UNSPECIFIED. ) 
 GEOMETRIC_REPRESENTATION_ITEM ( )  RATIONAL_B_SPLINE_SURFACE ( (
 ( 1.000000000000000000, 0.7087966873486530872, 1.000000000000000000),
 ( 1.000000000000000000, 0.7099442161580019617, 1.000000000000000000),
 ( 1.000000000000000000, 0.7112044574294733579, 1.000000000000000000),
 ( 1.000000000000000000, 0.7127234984257925232, 1.000000000000000000),
 ( 1.000000000000000000, 0.7131586427699522224, 1.000000000000000000),
 ( 1.000000000000000000, 0.7137747606611323237, 1.000000000000000000),
 ( 1.000000000000000000, 0.7139535051142154032, 1.000000000000000000),
 ( 1.000000000000000000, 0.7139024756042031683, 1.000000000000000000),
 ( 1.000000000000000000, 0.7136769813686398845, 1.000000000000000000),
 ( 1.000000000000000000, 0.7127126671718326811, 1.000000000000000000),
 ( 1.000000000000000000, 0.7119648005323482298, 1.000000000000000000),
 ( 1.000000000000000000, 0.7089786222043976682, 1.000000000000000000),
 ( 1.000000000000000000, 0.7059048385594330899, 1.000000000000000000),
 ( 1.000000000000000000, 0.7024277927095089469, 1.000000000000000000) ) ) 
 REPRESENTATION_ITEM ( '' )  SURFACE ( )  );
#5033 = ORGANIZATION ( 'NAUO-ORG16', 'UNSPECIFIED', 'UNSPECIFIED' ) ;
#5034 = ORIENTED_EDGE ( 'NONE', *, *, #950, .F. ) ;
#5035 = CARTESIAN_POINT ( 'NONE',  ( 0.2429745329104363027, -0.8738914638608461516, 0.4819356518895884789 ) ) ;
#5036 = CARTESIAN_POINT ( 'NONE',  ( -0.1969433606228570832, 0.5138636982738132852, 0.3750000000000001110 ) ) ;
#5037 = AXIS2_PLACEMENT_3D ( 'NONE', #39230, #5060, #8145 ) ;
#5038 = CARTESIAN_POINT ( 'NONE',  ( 0.1994650021643780136, -1.295469678022094229, 0.6991101051189098081 ) ) ;
#5039 = VERTEX_POINT ( 'NONE', #16927 ) ;
#5040 = CARTESIAN_POINT ( 'NONE',  ( -0.02869942827333567606, 0.2420058122830187619, 0.4357544236535290105 ) ) ;
#5041 = CARTESIAN_POINT ( 'NONE',  ( 0.03875523708677763163, 0.03329700455359576455, 0.4752403914626244230 ) ) ;
#5042 = CARTESIAN_POINT ( 'NONE',  ( 0.02238826743732996727, -0.5044115272350837564, -0.09031638658505519723 ) ) ;
#5043 = CARTESIAN_POINT ( 'NONE',  ( 0.1800577004789429558, -1.845764677012176724, -0.3170475007989994598 ) ) ;
#5044 = CARTESIAN_POINT ( 'NONE',  ( 0.4675665044693247951, -1.237121799919192355, 0.6039218906317980196 ) ) ;
#5045 = EDGE_CURVE ( 'NONE', #5149, #4721, #10253, .T. ) ;
#5047 = CARTESIAN_POINT ( 'NONE',  ( 0.3622253751127874066, -1.756884464425453984, -0.4902987826081479650 ) ) ;
#5046 = CARTESIAN_POINT ( 'NONE',  ( -0.02000000000000000042, -2.200964426145791464, -1.002314564012858566 ) ) ;
#5048 = CARTESIAN_POINT ( 'NONE',  ( -0.03309060444528731659, -0.2303206394829994674, -0.4671006372792942396 ) ) ;
#5049 = ORIENTED_EDGE ( 'NONE', *, *, #21937, .F. ) ;
#5050 = CARTESIAN_POINT ( 'NONE',  ( 0.4861228912811037528, -1.648612142294594074, 0.4182417262808776903 ) ) ;
#5051 = ORIENTED_EDGE ( 'NONE', *, *, #10049, .T. ) ;
#5052 = DIRECTION ( 'NONE',  ( -1.000000000000000000, -0.000000000000000000, -0.000000000000000000 ) ) ;
#5053 = CARTESIAN_POINT ( 'NONE',  ( 0.06047652861071878966, -0.5421273095757789262, 0.1825153154440289915 ) ) ;
#5055 = CARTESIAN_POINT ( 'NONE',  ( 0.1983634613346075826, -0.7568214873327272496, 0.3192403157822673032 ) ) ;
#5054 = CARTESIAN_POINT ( 'NONE',  ( 0.08859551772052549901, -0.5985747499489527668, 0.03208008976688550562 ) ) ;
#5056 = CARTESIAN_POINT ( 'NONE',  ( 0.4062230848227149638, -1.145582794160931117, 0.4248905050063955802 ) ) ;
#5057 = VERTEX_POINT ( 'NONE', #7445 ) ;
#5058 = ORIENTED_EDGE ( 'NONE', *, *, #35119, .T. ) ;
#5059 = CIRCLE ( 'NONE', #28073, 0.01500000000000001853 ) ;
#5060 = DIRECTION ( 'NONE',  ( 1.000000000000000000, 0.000000000000000000, 0.000000000000000000 ) ) ;
#5061 = CARTESIAN_POINT ( 'NONE',  ( 0.1337051625169099478, -0.6233194395910383045, 0.3688355370247377585 ) ) ;
#5062 = ORIENTED_EDGE ( 'NONE', *, *, #18590, .F. ) ;
#5063 = DIRECTION ( 'NONE',  ( 1.000000000000000000, 6.779273404243070203E-32, 4.314083075427408311E-32 ) ) ;
#5064 = CARTESIAN_POINT ( 'NONE',  ( 0.05634206451479450983, -0.4332270636364607408, 0.1516455289248211102 ) ) ;
#5065 = CARTESIAN_POINT ( 'NONE',  ( 0.6190054265851119286, -1.579626031360436222, 0.4182417262808776348 ) ) ;
#5066 = CARTESIAN_POINT ( 'NONE',  ( 0.1228677259314389508, -1.296195397236784785, 0.4358613769847314301 ) ) ;
#5067 = CARTESIAN_POINT ( 'NONE',  ( 0.3956653418828486868, -1.754139636876368424, -0.4989181662982050125 ) ) ;
#5068 = DIRECTION ( 'NONE',  ( 0.000000000000000000, 0.8063205929144885431, -0.5914787413272156735 ) ) ;
#5069 = CARTESIAN_POINT ( 'NONE',  ( 0.4812359531826634340, -1.078470577594583979, 0.8616913018466071383 ) ) ;
#5070 = CARTESIAN_POINT ( 'NONE',  ( 0.3656049513378988314, -1.732259804546445681, -0.6036892049131413751 ) ) ;
#5071 = CARTESIAN_POINT ( 'NONE',  ( -0.06980746140711623082, 7.160938508832261116E-17, 0.2149999999999999967 ) ) ;
#5072 = B_SPLINE_CURVE_WITH_KNOTS ( 'NONE', 3,
 ( #24989, #8952, #31177, #37331, #21923, #8739, #36724, #30759, #2579, #21525, #1294, #16155, #38699, #19993, #10727, #15725 ),
 .UNSPECIFIED., .F., .F.,
 ( 4, 2, 2, 2, 2, 2, 2, 4 ),
 ( 0.002977954003792171109, 0.003350115585507550727, 0.003722277167222930346, 0.004094438748938309530, 0.004466600330653689582, 0.004838761912369069634, 0.005210923494084448819, 0.005955246657515208056 ),
 .UNSPECIFIED. ) ;
#5073 = CARTESIAN_POINT ( 'NONE',  ( 0.6022157181008760407, -1.594425423205000580, -0.5367861729570986284 ) ) ;
#5074 = CARTESIAN_POINT ( 'NONE',  ( 0.02872242845529805050, 0.2464193076120176074, 0.4721747535845016164 ) ) ;
#5075 = DIRECTION ( 'NONE',  ( 0.4999551463232372317, -0.8660512985181134660, 0.000000000000000000 ) ) ;
#5076 = CARTESIAN_POINT ( 'NONE',  ( 0.5755854119334320451, -1.646982683870169328, -0.5473203437262896820 ) ) ;
#5077 = CARTESIAN_POINT ( 'NONE',  ( -0.03650581953630666066, 0.5059763899182377900, -0.07647306779615337113 ) ) ;
#5078 = CARTESIAN_POINT ( 'NONE',  ( 0.008057578236607982475, -0.5544447393747381492, 0.4149153965127375110 ) ) ;
#5079 = CARTESIAN_POINT ( 'NONE',  ( 0.5644318452406892339, -1.583177861798296115, -0.4893328019707191556 ) ) ;
#5080 = CARTESIAN_POINT ( 'NONE',  ( 0.1784822832398731962, -1.263697370786425411, 0.5370935804641795430 ) ) ;
#5081 = CARTESIAN_POINT ( 'NONE',  ( 0.05582223227535057508, -1.291805717968274037, 0.5182417262812423209 ) ) ;
#5083 = VERTEX_POINT ( 'NONE', #20418 ) ;
#5082 = B_SPLINE_SURFACE_WITH_KNOTS ( 'NONE', 5, 5, ( 
 ( #550, #3579, #28877, #38127, #19628, #13047 ),
 ( #37730, #31968, #6854, #13454, #22930, #16338 ),
 ( #22130, #34646, #31549, #19018, #25187, #19822 ),
 ( #35044, #7059, #25599, #735, #7247, #15921 ),
 ( #9951, #13241, #12846, #342, #6646, #3366 ),
 ( #3972, #32163, #25407, #32355, #12623, #29075 ) ),
 .UNSPECIFIED., .F., .F., .F.,
 ( 6, 6 ),
 ( 6, 6 ),
 ( -6.477000000001651436, 6.477000000001639002 ),
 ( -2.080605796196421498, 4.396394203803585476 ),
 .UNSPECIFIED. ) ;
#5084 = CARTESIAN_POINT ( 'NONE',  ( -0.01548846960707545191, -0.5346638663566692928, 0.07572681171513533094 ) ) ;
#5085 = CARTESIAN_POINT ( 'NONE',  ( 0.4091335057472371695, -1.131547141905885789, 0.4177417262808780229 ) ) ;
#5086 = DIRECTION ( 'NONE',  ( 0.000000000000000000, -0.5781348229923757298, 0.8159412518334727693 ) ) ;
#5087 = CARTESIAN_POINT ( 'NONE',  ( 0.6000000852309536059, -1.576678414952007445, -0.4214712295370082740 ) ) ;
#5088 = CARTESIAN_POINT ( 'NONE',  ( 0.5224595318596155780, -1.331650646383924386, 0.6038439222826686992 ) ) ;
#5090 = VERTEX_POINT ( 'NONE', #1127 ) ;
#5089 = CARTESIAN_POINT ( 'NONE',  ( -0.05634301242525814601, 0.4396003943662979419, 0.1320237143668709923 ) ) ;
#5091 = CARTESIAN_POINT ( 'NONE',  ( 0.4767475950167052168, -1.082687895696078595, 0.6905128956159171105 ) ) ;
#5092 = ADVANCED_FACE ( 'NONE', ( #32340 ), #35433, .F. ) ;
#5093 = CARTESIAN_POINT ( 'NONE',  ( 0.04293317454820645696, 0.4876093284570318653, -0.08292018301452643014 ) ) ;
#5094 = ORIENTED_EDGE ( 'NONE', *, *, #28235, .T. ) ;
#5095 = DIRECTION ( 'NONE',  ( 0.3468893892380797150, 0.2594111197900920152, 0.9013177145509138066 ) ) ;
#5096 = EDGE_CURVE ( 'NONE', #29289, #14658, #23431, .T. ) ;
#5097 = ORIENTED_EDGE ( 'NONE', *, *, #37671, .T. ) ;
#5098 = CARTESIAN_POINT ( 'NONE',  ( 0.3402366556150817622, -1.560274116414339884, 0.8083988018111346596 ) ) ;
#5100 = CARTESIAN_POINT ( 'NONE',  ( 0.1763856455429072267, -0.5524551084071943619, -0.04065491940077346072 ) ) ;
#5099 = CARTESIAN_POINT ( 'NONE',  ( 0.6706115226080072711, -1.534602134890148850, 0.4364891473496426699 ) ) ;
#5101 = CARTESIAN_POINT ( 'NONE',  ( 0.4971920908461615607, -1.080069027881642052, 0.4687417262808780127 ) ) ;
#5102 = EDGE_CURVE ( 'NONE', #33386, #35465, #39880, .T. ) ;
#5103 = ORIENTED_EDGE ( 'NONE', *, *, #37614, .T. ) ;
#5104 = EDGE_CURVE ( 'NONE', #39766, #35558, #31887, .T. ) ;
#5105 = EDGE_LOOP ( 'NONE', ( #22590, #19444, #18928, #28486 ) ) ;
#5106 = CARTESIAN_POINT ( 'NONE',  ( -0.2399999999999999079, -3.723902497147952406, 0.1004495357399106253 ) ) ;
#5107 = CARTESIAN_POINT ( 'NONE',  ( 0.3686258320291115886, -2.054720120239651671, -0.5116857311949160048 ) ) ;
#5108 = CARTESIAN_POINT ( 'NONE',  ( 0.1267896730660402760, -0.9030892566507676689, 0.5786158305868386309 ) ) ;
#5109 = CARTESIAN_POINT ( 'NONE',  ( 0.3224764602545437953, -1.754077001593124185, 0.4780754602289729593 ) ) ;
#5110 = DIRECTION ( 'NONE',  ( 0.2994471003784440755, -0.9541129042597328302, 0.000000000000000000 ) ) ;
#5111 = CARTESIAN_POINT ( 'NONE',  ( 7.512581982576723358E-16, -0.2981948553318921613, -3.414809992080329023E-16 ) ) ;
#5112 = CARTESIAN_POINT ( 'NONE',  ( 0.6596209037232241279, -1.565455939274822184, 0.3157417262808776548 ) ) ;
#5113 = CARTESIAN_POINT ( 'NONE',  ( 0.05562144613422637801, 0.2870684680408734923, -0.3605846877396488570 ) ) ;
#5114 = EDGE_CURVE ( 'NONE', #8591, #25550, #19736, .T. ) ;
#5115 = CARTESIAN_POINT ( 'NONE',  ( 0.01548846960707524721, 0.5346638663566677385, -0.07572681171513587217 ) ) ;
#5116 = CARTESIAN_POINT ( 'NONE',  ( 0.000000000000000000, 0.1969856463038233696, 0.03459270371430114843 ) ) ;
#5117 = PERSON_AND_ORGANIZATION ( #28500, #32463 ) ;
#5118 = APPLIED_DATE_AND_TIME_ASSIGNMENT ( #38217, #16413, ( #33833 ) ) ;
#5119 = B_SPLINE_CURVE_WITH_KNOTS ( 'NONE', 3,
 ( #9170, #14753, #5470, #21347 ),
 .UNSPECIFIED., .F., .F.,
 ( 4, 4 ),
 ( 0.002631652860467224766, 0.002956730596035610920 ),
 .UNSPECIFIED. ) ;
#5120 = CARTESIAN_POINT ( 'NONE',  ( 0.4035007565703578325, -1.146148456392026116, 0.4243490465986823335 ) ) ;
#5121 = CARTESIAN_POINT ( 'NONE',  ( 0.4474917948846165450, -1.247628998557391400, 0.6057417262809816627 ) ) ;
#5122 = CIRCLE ( 'NONE', #37313, 0.01499999999999999424 ) ;
#5123 = CARTESIAN_POINT ( 'NONE',  ( 0.1999999999999789724, -2.183180860297921466, -0.4937760292030871079 ) ) ;
#5124 = CARTESIAN_POINT ( 'NONE',  ( 1.372100516120995828E-05, -0.5265032726816540887, -0.06060675249349117139 ) ) ;
#5125 = CARTESIAN_POINT ( 'NONE',  ( 0.3782504645320439174, -1.760900442173329195, -0.5806069901403015932 ) ) ;
#5126 = DIRECTION ( 'NONE',  ( -0.8660254037844394848, 0.3322823180458164272, -0.3736153919662538736 ) ) ;
#5127 = CARTESIAN_POINT ( 'NONE',  ( -0.2746410161513776482, -3.812085038045152974, -0.02801711824816583915 ) ) ;
#5128 = ORIENTED_EDGE ( 'NONE', *, *, #34424, .F. ) ;
#5129 = EDGE_LOOP ( 'NONE', ( #18820, #30719, #4794, #34099 ) ) ;
#5130 = CARTESIAN_POINT ( 'NONE',  ( -0.02000000000000000042, -1.765869171405739957, -0.8132390237819782097 ) ) ;
#5131 = ORIENTED_EDGE ( 'NONE', *, *, #2953, .F. ) ;
#5132 = DIRECTION ( 'NONE',  ( 0.3779644730092284743, 0.9258200997725509751, 0.000000000000000000 ) ) ;
#5134 = ORIENTED_EDGE ( 'NONE', *, *, #20063, .F. ) ;
#5133 = PLANE ( 'NONE',  #4663 ) ;
#5136 = ORIENTED_EDGE ( 'NONE', *, *, #18783, .F. ) ;
#5135 = CARTESIAN_POINT ( 'NONE',  ( 0.0006976930216080560456, -0.6123561560918749924, -0.004704502767504344096 ) ) ;
#5137 = ORIENTED_EDGE ( 'NONE', *, *, #28394, .T. ) ;
#5138 = CARTESIAN_POINT ( 'NONE',  ( 0.3511079287476752686, -1.164805985122749687, 0.4335040596137051394 ) ) ;
#5139 = ADVANCED_FACE ( 'NONE', ( #19349 ), #25518, .T. ) ;
#5140 =( BOUNDED_SURFACE ( )  B_SPLINE_SURFACE ( 3, 2, ( 
 ( #36742, #27499, #33877 ),
 ( #11848, #34065, #39837 ),
 ( #15350, #18422, #5462 ),
 ( #12272, #27909, #24829 ) ),
 .UNSPECIFIED., .F., .F., .F. ) 
 B_SPLINE_SURFACE_WITH_KNOTS ( ( 4, 4 ),
 ( 3, 3 ),
 ( -2.744332538995308823E-15, 0.004359680035277800104 ),
 ( 0.000000000000000000, 1.000000000000000000 ),
 .UNSPECIFIED. ) 
 GEOMETRIC_REPRESENTATION_ITEM ( )  RATIONAL_B_SPLINE_SURFACE ( (
 ( 1.000000000000000000, 0.7004196158486113433, 1.000000000000000000),
 ( 1.000000000000000000, 0.7024542282359754752, 1.000000000000000000),
 ( 1.000000000000000000, 0.7046422212203753421, 1.000000000000000000),
 ( 1.000000000000000000, 0.7054447009685760328, 1.000000000000000000) ) ) 
 REPRESENTATION_ITEM ( '' )  SURFACE ( )  );
#5141 = ORIENTED_EDGE ( 'NONE', *, *, #24940, .F. ) ;
#5142 = CARTESIAN_POINT ( 'NONE',  ( 0.2233061389546777964, -1.398491456369854280, 0.9267770701875633899 ) ) ;
#5144 = CARTESIAN_POINT ( 'NONE',  ( 0.1399309073568716921, -1.253615150487832341, 0.6230334390714287185 ) ) ;
#5143 = CARTESIAN_POINT ( 'NONE',  ( -0.03868264068766668479, -0.4417248602032604055, -0.1788646266443680855 ) ) ;
#5145 = CARTESIAN_POINT ( 'NONE',  ( 0.6380336481227063539, -1.610932490174762366, -0.4493560576004195783 ) ) ;
#5146 = COORDINATED_UNIVERSAL_TIME_OFFSET ( 0, 0, .AHEAD. ) ;
#5147 = EDGE_CURVE ( 'NONE', #29909, #33903, #659, .T. ) ;
#5148 = CARTESIAN_POINT ( 'NONE',  ( 0.7092779456818100181, -1.502766204822708174, 0.5668339295794848631 ) ) ;
#5150 = ORIENTED_EDGE ( 'NONE', *, *, #20791, .T. ) ;
#5149 = VERTEX_POINT ( 'NONE', #6374 ) ;
#5151 = B_SPLINE_CURVE_WITH_KNOTS ( 'NONE', 3,
 ( #5844, #37520, #33628, #6265, #5441, #27286 ),
 .UNSPECIFIED., .F., .F.,
 ( 4, 2, 4 ),
 ( 0.008641842504323983890, 0.009239025970640010743, 0.009836209436956035862 ),
 .UNSPECIFIED. ) ;
#5152 = ADVANCED_FACE ( 'NONE', ( #28799 ), #3497, .T. ) ;
#5153 = DIRECTION ( 'NONE',  ( 0.8660512985181126888, 0.4999551463232385085, 0.000000000000000000 ) ) ;
#5154 = DIRECTION ( 'NONE',  ( 0.8660512985181142431, 0.4999551463232357884, 0.000000000000000000 ) ) ;
#5155 = CARTESIAN_POINT ( 'NONE',  ( 0.1760646372844321683, -0.7862967544061189029, 0.6064719630404880046 ) ) ;
#5156 = CARTESIAN_POINT ( 'NONE',  ( 0.1869504391848741121, -0.7244332150394979797, 0.03244844288826874423 ) ) ;
#5157 = LINE ( 'NONE', #21018, #36933 ) ;
#5158 = CARTESIAN_POINT ( 'NONE',  ( 0.6472156995107305466, -1.554538954898049052, 0.4226020063017070227 ) ) ;
#5159 = CARTESIAN_POINT ( 'NONE',  ( 0.01220508677664999299, -0.4284039737085656996, 0.1457185332388702959 ) ) ;
#5160 = DIRECTION ( 'NONE',  ( 0.01455087615875041117, 0.9998941303973198913, 0.000000000000000000 ) ) ;
#5161 = CARTESIAN_POINT ( 'NONE',  ( 0.1927077495703349852, -0.8180328145591141409, 0.2791508387892263077 ) ) ;
#5162 = CARTESIAN_POINT ( 'NONE',  ( 0.3699999999999787903, -2.050772785069567838, -0.3050017341552441197 ) ) ;
#5163 = DIRECTION ( 'NONE',  ( 0.4999551463232372317, -0.8660512985181133550, 0.000000000000000000 ) ) ;
#5164 = CARTESIAN_POINT ( 'NONE',  ( -0.2746410161513776482, -3.941790907013290823, -0.4709369376873030477 ) ) ;
#5165 = EDGE_CURVE ( 'NONE', #4884, #25380, #2372, .T. ) ;
#5166 = CARTESIAN_POINT ( 'NONE',  ( 0.4377606765896609464, -1.229990982179016701, 0.5852478207895496221 ) ) ;
#5167 = MANIFOLD_SOLID_BREP ( 'Fillet1', #1725 ) ;
#5168 = CARTESIAN_POINT ( 'NONE',  ( 0.6307892698844480561, -1.598909026140060918, -0.5827525826989481406 ) ) ;
#5169 = CARTESIAN_POINT ( 'NONE',  ( -8.537024980200822558E-17, -0.6872203660140394632, 0.1631394164078588394 ) ) ;
#5170 = CARTESIAN_POINT ( 'NONE',  ( 0.4544126380536514520, -1.061573323663441704, 0.6302127423442334120 ) ) ;
#5171 = CARTESIAN_POINT ( 'NONE',  ( 0.03176206407908215706, -0.9495151868022172481, 0.6313809608633471626 ) ) ;
#5172 = PERSON_AND_ORGANIZATION ( #28500, #32463 ) ;
#5173 = CARTESIAN_POINT ( 'NONE',  ( 0.5012199843439465452, -1.111650260509063681, 0.8688705274730272876 ) ) ;
#5174 = CARTESIAN_POINT ( 'NONE',  ( 0.3632268640774227175, -1.623167453423570050, -0.6631189784283982869 ) ) ;
#5175 = CARTESIAN_POINT ( 'NONE',  ( 0.03478489236951704672, 0.07228210831916115353, -0.5113624180529584562 ) ) ;
#5176 = DIRECTION ( 'NONE',  ( 0.000000000000000000, 0.9510565162951627460, -0.3090169943749190296 ) ) ;
#5177 = VERTEX_POINT ( 'NONE', #1065 ) ;
#5178 = CARTESIAN_POINT ( 'NONE',  ( 0.2534230856981304347, -1.365321207853003926, -0.7462941026102631881 ) ) ;
#5179 = CARTESIAN_POINT ( 'NONE',  ( 0.04850978628623311278, -0.8094765694360999131, 0.6771444674279119003 ) ) ;
#5180 = CARTESIAN_POINT ( 'NONE',  ( 0.5848005186207935191, -1.482150277494033608, 0.6650156861691463028 ) ) ;
#5181 = CARTESIAN_POINT ( 'NONE',  ( 0.3003068002427916605, -1.655642049652715331, 0.4394976263036083353 ) ) ;
#5183 = ORIENTED_EDGE ( 'NONE', *, *, #13209, .T. ) ;
#5182 = CARTESIAN_POINT ( 'NONE',  ( 0.3923243630925589143, -1.966611948492527073, -0.4968729097669083439 ) ) ;
#5184 = CARTESIAN_POINT ( 'NONE',  ( -0.03309060444528701822, -0.4608881774262385544, -0.2425132784556381649 ) ) ;
#5185 = CARTESIAN_POINT ( 'NONE',  ( 0.6089993539687283963, -1.280207732015472333, 0.6563525730433853456 ) ) ;
#5187 = ORIENTED_EDGE ( 'NONE', *, *, #36047, .F. ) ;
#5186 = ORIENTED_EDGE ( 'NONE', *, *, #2706, .T. ) ;
#5188 = CARTESIAN_POINT ( 'NONE',  ( 0.07370827096331192263, -1.490549976626241557, -0.6787781514709749775 ) ) ;
#5189 = ADVANCED_FACE ( 'NONE', ( #3706 ), #10960, .F. ) ;
#5190 = VERTEX_POINT ( 'NONE', #9461 ) ;
#5191 = DIRECTION ( 'NONE',  ( 0.000000000000000000, 0.5877852522924701395, -0.8090169943749496717 ) ) ;
#5192 = PRODUCT_DEFINITION_SHAPE ( 'NONE', 'NONE',  #40657 ) ;
#5193 = DIRECTION ( 'NONE',  ( 7.771561172376107616E-16, -7.170354002788761615E-17, 1.000000000000000000 ) ) ;
#5194 = SECURITY_CLASSIFICATION_LEVEL ( 'unclassified' ) ;
#5195 = ADVANCED_FACE ( 'NONE', ( #28390 ), #12919, .F. ) ;
#5196 = DIRECTION ( 'NONE',  ( 0.000000000000000000, -0.9510565162951465368, -0.3090169943749687120 ) ) ;
#5197 = VERTEX_POINT ( 'NONE', #22040 ) ;
#5198 = CARTESIAN_POINT ( 'NONE',  ( 0.1471926383934134275, -1.243287368939621773, 0.6046105284403431313 ) ) ;
#5199 = EDGE_CURVE ( 'NONE', #14323, #36573, #32269, .T. ) ;
#5200 = CARTESIAN_POINT ( 'NONE',  ( 0.08692586860950439476, -0.7045980206078545915, 0.1457185332388693799 ) ) ;
#5201 = CARTESIAN_POINT ( 'NONE',  ( 0.1371221799207314740, -1.062251636642305819, 0.9748385851047789430 ) ) ;
#5202 = CARTESIAN_POINT ( 'NONE',  ( 0.1029772949285807093, -0.5926062987907158019, 0.3127404110831066841 ) ) ;
#5204 = CARTESIAN_POINT ( 'NONE',  ( 0.01548846960706681299, -0.3772621329472835017, 0.3651003739303615991 ) ) ;
#5203 = CYLINDRICAL_SURFACE ( 'NONE', #12537, 0.1000000000000000194 ) ;
#5205 = CARTESIAN_POINT ( 'NONE',  ( 0.000000000000000000, -0.9481888444201338473, 0.1457185332388702959 ) ) ;
#5206 = VERTEX_POINT ( 'NONE', #22242 ) ;
#5207 = ADVANCED_FACE ( 'NONE', ( #22649 ), #35548, .T. ) ;
#5208 = EDGE_LOOP ( 'NONE', ( #756, #24455, #8581, #24753, #38506 ) ) ;
#5209 = DIRECTION ( 'NONE',  ( -0.5000000000000009992, -0.7066258520834616252, -0.5006794435238185459 ) ) ;
#5210 = CARTESIAN_POINT ( 'NONE',  ( 0.3345257678029842086, -0.8717194449991449989, 0.6804045188348578632 ) ) ;
#5211 = CARTESIAN_POINT ( 'NONE',  ( 0.4170115945640069932, -1.702980413955156758, -0.6123808887097255127 ) ) ;
#5212 = ADVANCED_FACE ( 'NONE', ( #37858 ), #28989, .F. ) ;
#5213 = CARTESIAN_POINT ( 'NONE',  ( -2.775557561562891351E-16, -0.05999999999999977573, -0.1999999999999994837 ) ) ;
#5214 =( NAMED_UNIT ( * ) PLANE_ANGLE_UNIT ( ) SI_UNIT ( $, .RADIAN. ) );
#5215 = EDGE_CURVE ( 'NONE', #13200, #11734, #37915, .T. ) ;
#5216 = CARTESIAN_POINT ( 'NONE',  ( 0.3695052819757340123, -1.758428263776099287, -0.4278193900811940176 ) ) ;
#5217 = ADVANCED_FACE ( 'NONE', ( #38459 ), #23466, .T. ) ;
#5218 = CARTESIAN_POINT ( 'NONE',  ( 0.3839258146201624533, -1.730368705836311083, -0.7198767004735652231 ) ) ;
#5219 = CARTESIAN_POINT ( 'NONE',  ( 0.3124895060288936377, -1.175537060766050246, 0.5079170196689681838 ) ) ;
#5220 = CARTESIAN_POINT ( 'NONE',  ( 0.2766509774079478068, -0.8188515361471339071, 0.5743688119339978027 ) ) ;
#5221 = DATE_AND_TIME ( #7552, #25958 ) ;
#5222 = DIRECTION ( 'NONE',  ( 1.000000000000000000, 6.779273404243070203E-32, 4.314083075427408311E-32 ) ) ;
#5223 = FACE_OUTER_BOUND ( 'NONE', #2773, .T. ) ;
#5224 = CARTESIAN_POINT ( 'NONE',  ( -0.2399999999999999079, -2.914247627487775105, -0.7567636692719127423 ) ) ;
#5225 = VERTEX_POINT ( 'NONE', #2036 ) ;
#5226 = CARTESIAN_POINT ( 'NONE',  ( 0.4567587145471871390, -1.219596911210154566, 0.5765795053216835608 ) ) ;
#5227 = LINE ( 'NONE', #17386, #9381 ) ;
#5228 = CARTESIAN_POINT ( 'NONE',  ( -0.03647137243075214419, -0.3644785006310388709, -0.3593174381849628674 ) ) ;
#5229 = ORIENTED_EDGE ( 'NONE', *, *, #31657, .F. ) ;
#5230 = CARTESIAN_POINT ( 'NONE',  ( 0.2923286432308245808, -1.660243258845594649, -0.6250000000000000000 ) ) ;
#5231 = DIRECTION ( 'NONE',  ( -7.771561172376107616E-16, 7.170354002788761615E-17, -1.000000000000000000 ) ) ;
#5232 = CARTESIAN_POINT ( 'NONE',  ( 0.06895221775114691865, -0.9317196315810322149, 0.6128942806377850605 ) ) ;
#5233 = VERTEX_POINT ( 'NONE', #38656 ) ;
#5234 = CARTESIAN_POINT ( 'NONE',  ( 0.03171861681796955129, -0.07587220456996765505, 0.5191007718638491752 ) ) ;
#5235 = CARTESIAN_POINT ( 'NONE',  ( 0.03875523708678054596, -0.4622698113760334016, -0.1151900242215433134 ) ) ;
#5236 = CARTESIAN_POINT ( 'NONE',  ( 0.1963846320365078280, -1.666482349971158072, -0.3293983578754329233 ) ) ;
#5237 = CARTESIAN_POINT ( 'NONE',  ( 0.4771042051721851029, -1.253291307408614053, 0.6140431522715210644 ) ) ;
#5238 = EDGE_CURVE ( 'NONE', #5225, #38396, #39269, .T. ) ;
#5240 = CARTESIAN_POINT ( 'NONE',  ( 0.2729656450513567312, -1.175066423404427463, -0.5155029497116575543 ) ) ;
#5239 = CARTESIAN_POINT ( 'NONE',  ( -0.1443375672974067936, 0.05141091571461216952, 0.000000000000000000 ) ) ;
#5241 = CARTESIAN_POINT ( 'NONE',  ( -0.1743922129835729085, -0.5166151207188712791, 0.3750000000000001110 ) ) ;
#5242 = ORIENTED_EDGE ( 'NONE', *, *, #25793, .F. ) ;
#5243 = ORIENTED_EDGE ( 'NONE', *, *, #23622, .T. ) ;
#5244 = EDGE_CURVE ( 'NONE', #15727, #1246, #31947, .T. ) ;
#5245 = CARTESIAN_POINT ( 'NONE',  ( 0.4012118689501711910, -1.155916157891842211, 0.4182417262808778013 ) ) ;
#5246 = ORIENTED_EDGE ( 'NONE', *, *, #33175, .F. ) ;
#5247 = CARTESIAN_POINT ( 'NONE',  ( 0.1912830164987288084, -0.5477411782657776174, 0.1015045423513593059 ) ) ;
#5248 = CARTESIAN_POINT ( 'NONE',  ( 0.4434119773370868711, -1.573474031461190581, 0.6057253118067152942 ) ) ;
#5250 = CARTESIAN_POINT ( 'NONE',  ( 0.4333248279805138603, -1.117134059754063102, -0.6448776663562968414 ) ) ;
#5249 = CARTESIAN_POINT ( 'NONE',  ( 0.08770615875230125535, -0.6684773603782572238, 0.002659437449977570134 ) ) ;
#5251 = CARTESIAN_POINT ( 'NONE',  ( 0.5884429758178558734, -1.489330091540539636, 0.4807459044743478405 ) ) ;
#5252 = EDGE_LOOP ( 'NONE', ( #15782, #28149, #18458, #38492 ) ) ;
#5253 = CARTESIAN_POINT ( 'NONE',  ( 0.3999999999999789280, -2.042495778117166427, -0.2760839614659714170 ) ) ;
#5254 = CARTESIAN_POINT ( 'NONE',  ( 0.4888238443203842265, -1.356165068348983205, 0.8108664833413182782 ) ) ;
#5255 = CARTESIAN_POINT ( 'NONE',  ( 0.3301505661793556201, -1.753418133777565835, 0.5634441686133024874 ) ) ;
#5256 = CARTESIAN_POINT ( 'NONE',  ( 0.6394864831434140529, -1.564145959968468169, 0.4219395085220526975 ) ) ;
#5257 = CARTESIAN_POINT ( 'NONE',  ( 0.1472428470117045640, -1.270554630056540901, 0.4305824032786366162 ) ) ;
#5258 = VECTOR ( 'NONE', #10278, 39.37007874015748143 ) ;
#5259 = CARTESIAN_POINT ( 'NONE',  ( 0.3969982963057281378, -1.750077671058421824, -0.4821875037442182599 ) ) ;
#5260 = CARTESIAN_POINT ( 'NONE',  ( 0.3815368266015568555, -1.759003287083186651, -0.4522571440128324571 ) ) ;
#5261 = CARTESIAN_POINT ( 'NONE',  ( 0.3762811493344272451, -0.8989788859175238400, 0.7888608478858359918 ) ) ;
#5262 = AXIS2_PLACEMENT_3D ( 'NONE', #26166, #10506, #20192 ) ;
#5263 = CARTESIAN_POINT ( 'NONE',  ( 0.07881452883472495063, -1.319805653379759525, 0.4755639510338647291 ) ) ;
#5264 = CARTESIAN_POINT ( 'NONE',  ( -0.1603938765018561030, 0.4636889572247975266, 0.3382895567582887564 ) ) ;
#5265 = CARTESIAN_POINT ( 'NONE',  ( 0.5781127729594031095, -1.609402375371582261, -0.4754652686900157632 ) ) ;
#5266 = CARTESIAN_POINT ( 'NONE',  ( 0.02242828275839013272, 0.2417645306140285832, 0.4517153736362803929 ) ) ;
#5267 = DIRECTION ( 'NONE',  ( 5.264498737790487855E-15, -0.7185945389471846134, -0.6954292836768403152 ) ) ;
#5268 = CARTESIAN_POINT ( 'NONE',  ( 0.3867756831795865491, -1.746236785580605799, -0.4374737505989281794 ) ) ;
#5269 = DIRECTION ( 'NONE',  ( 0.000000000000000000, 1.707404996040147600E-15, -1.000000000000000000 ) ) ;
#5270 = CARTESIAN_POINT ( 'NONE',  ( -9.828236692375560680E-17, -0.4262518876079541830, 0.09312799375524088985 ) ) ;
#5271 = CARTESIAN_POINT ( 'NONE',  ( 0.4025254666410605919, -1.691731883620783972, -0.6096246207440890741 ) ) ;
#5272 = DIRECTION ( 'NONE',  ( 1.000000000000000000, 0.000000000000000000, 0.000000000000000000 ) ) ;
#5273 = FACE_OUTER_BOUND ( 'NONE', #32684, .T. ) ;
#5274 = ORIENTED_EDGE ( 'NONE', *, *, #25537, .T. ) ;
#5275 = DIRECTION ( 'NONE',  ( -0.4999551463232373427, 0.8660512985181134660, -0.000000000000000000 ) ) ;
#5276 = CARTESIAN_POINT ( 'NONE',  ( 0.3874633503144017110, -1.108325317417463873, 0.6051044758646879629 ) ) ;
#5277 = CARTESIAN_POINT ( 'NONE',  ( -0.05562144613422701639, 0.2542273817772375821, -0.3844451335760736277 ) ) ;
#5278 = CARTESIAN_POINT ( 'NONE',  ( 0.5328282478916582798, -1.349129593841621455, 0.6122296912113598388 ) ) ;
#5279 = CIRCLE ( 'NONE', #19120, 0.02499999999999993894 ) ;
#5281 = VERTEX_POINT ( 'NONE', #1652 ) ;
#5280 = CARTESIAN_POINT ( 'NONE',  ( -0.03309057659885079189, 0.5154121718708730704, 0.07470590733143719908 ) ) ;
#5282 = CARTESIAN_POINT ( 'NONE',  ( 0.4864609864856930255, -1.087049186798351608, 0.6366279691173203359 ) ) ;
#5283 = VERTEX_POINT ( 'NONE', #23853 ) ;
#5284 = DIRECTION ( 'NONE',  ( -1.000000000000000000, -0.000000000000000000, -0.000000000000000000 ) ) ;
#5285 = ORIENTED_EDGE ( 'NONE', *, *, #3996, .T. ) ;
#5286 = DIRECTION ( 'NONE',  ( -0.4999551463232377313, 0.8660512985181132439, 0.000000000000000000 ) ) ;
#5287 = AXIS2_PLACEMENT_3D ( 'NONE', #16382, #38591, #10413 ) ;
#5288 = CARTESIAN_POINT ( 'NONE',  ( 0.3554062530147323873, -1.622120902010288690, 0.5636526721968185827 ) ) ;
#5290 = CARTESIAN_POINT ( 'NONE',  ( -0.03159140494780091069, -0.3316214887069892647, 0.3635694333040963011 ) ) ;
#5289 = CARTESIAN_POINT ( 'NONE',  ( 0.7070466114709489380, -1.508851404092110826, 0.5588543131432650579 ) ) ;
#5291 = DIRECTION ( 'NONE',  ( 1.000000000000000000, 0.000000000000000000, 0.000000000000000000 ) ) ;
#5292 = ORIENTED_EDGE ( 'NONE', *, *, #6808, .T. ) ;
#5293 = ORIENTED_EDGE ( 'NONE', *, *, #6869, .T. ) ;
#5294 = ORIENTED_EDGE ( 'NONE', *, *, #39382, .F. ) ;
#5295 = CARTESIAN_POINT ( 'NONE',  ( 0.1499999999999993561, 0.000000000000000000, 0.000000000000000000 ) ) ;
#5296 = DIRECTION ( 'NONE',  ( 0.000000000000000000, 0.000000000000000000, -1.000000000000000000 ) ) ;
#5297 = CARTESIAN_POINT ( 'NONE',  ( 0.3319403630591542531, -1.291129383779237250, 0.5682417262808747704 ) ) ;
#5298 = CARTESIAN_POINT ( 'NONE',  ( -0.1530923209794422257, 0.4738745695581272344, 0.09813923389055254076 ) ) ;
#5299 = FACE_OUTER_BOUND ( 'NONE', #21620, .T. ) ;
#5300 = DIRECTION ( 'NONE',  ( -1.000000000000000000, 0.000000000000000000, 0.000000000000000000 ) ) ;
#5301 = CARTESIAN_POINT ( 'NONE',  ( 0.07172816549509457296, -1.333591607576925187, 0.4986374818479088478 ) ) ;
#5302 = CARTESIAN_POINT ( 'NONE',  ( 0.2625973931889362678, -0.6796768235205253861, 0.1477649966949237115 ) ) ;
#5303 = DIRECTION ( 'NONE',  ( -1.000000000000000000, -0.000000000000000000, -0.000000000000000000 ) ) ;
#5304 = CARTESIAN_POINT ( 'NONE',  ( 6.608588869366793274E-05, -0.9486129085773968850, 0.1942756810714297844 ) ) ;
#5305 = DATE_AND_TIME ( #14378, #6885 ) ;
#5306 = CIRCLE ( 'NONE', #3354, 0.02999999999999998501 ) ;
#5307 = CARTESIAN_POINT ( 'NONE',  ( 0.4285077932704187131, -1.141367488323234758, 0.4310073631607372335 ) ) ;
#5308 = AXIS2_PLACEMENT_3D ( 'NONE', #215, #6729, #31847 ) ;
#5309 = CARTESIAN_POINT ( 'NONE',  ( 0.05999999999999990757, 0.000000000000000000, 0.6114999999999938263 ) ) ;
#5310 = APPLICATION_CONTEXT ( 'configuration controlled 3d designs of mechanical parts and assemblies' ) ;
#5311 = DIRECTION ( 'NONE',  ( 0.000000000000000000, 0.000000000000000000, -1.000000000000000000 ) ) ;
#5312 = TOROIDAL_SURFACE ( 'NONE', #19813, 0.04500000000000023426, 0.01499999999999999944 ) ;
#5313 = VERTEX_POINT ( 'NONE', #35777 ) ;
#5314 = CIRCLE ( 'NONE', #2705, 0.08830708661417320526 ) ;
#5315 = CARTESIAN_POINT ( 'NONE',  ( 0.01188081175741144760, -0.5563285785164118202, -0.07779187151457800375 ) ) ;
#5316 = CARTESIAN_POINT ( 'NONE',  ( -0.02000000000000000042, -2.196071624283071788, -0.8624000883860228894 ) ) ;
#5317 = CIRCLE ( 'NONE', #32907, 0.2526340763130724976 ) ;
#5318 = DIRECTION ( 'NONE',  ( -0.4887635750373031107, -0.8724162812079762075, 4.177458024893467913E-17 ) ) ;
#5319 = CARTESIAN_POINT ( 'NONE',  ( 0.5953303036072959964, -1.457508885835639978, 0.6057417262805095959 ) ) ;
#5320 = EDGE_LOOP ( 'NONE', ( #36211, #16158, #9047, #14488 ) ) ;
#5321 = ORIENTED_EDGE ( 'NONE', *, *, #27622, .T. ) ;
#5322 = CARTESIAN_POINT ( 'NONE',  ( -0.1092363788443199563, -0.4985689912535452017, 0.1005717796976069445 ) ) ;
#5323 = ORIENTED_EDGE ( 'NONE', *, *, #25654, .F. ) ;
#5324 = DIRECTION ( 'NONE',  ( 1.000000000000000000, 2.341930812374887555E-31, -1.664003471950578127E-31 ) ) ;
#5325 = CARTESIAN_POINT ( 'NONE',  ( -0.1044436713285806784, -0.4741860147766130407, 0.09550516381870173543 ) ) ;
#5327 = ORIENTED_EDGE ( 'NONE', *, *, #2098, .T. ) ;
#5326 = CARTESIAN_POINT ( 'NONE',  ( -0.001385626645067268960, -0.8086677941022779592, 0.04152584225078851526 ) ) ;
#5328 = CIRCLE ( 'NONE', #28352, 0.03000000000000022787 ) ;
#5329 = EDGE_LOOP ( 'NONE', ( #7402, #38141, #34306, #29185, #28421, #4390, #29755, #11054, #5879, #32034 ) ) ;
#5330 = DIRECTION ( 'NONE',  ( -0.4999551463232371762, 0.8660512985181134660, -0.000000000000000000 ) ) ;
#5331 = VERTEX_POINT ( 'NONE', #35567 ) ;
#5332 = ADVANCED_FACE ( 'NONE', ( #7788 ), #32690, .T. ) ;
#5333 = CARTESIAN_POINT ( 'NONE',  ( 0.1004293403852877520, -0.9989955727027649557, 0.8255344432128082222 ) ) ;
#5335 = CARTESIAN_POINT ( 'NONE',  ( 0.5277393960915062188, -1.600937019047668386, -0.4329714461315667950 ) ) ;
#5334 = CARTESIAN_POINT ( 'NONE',  ( -0.2746410161513782033, -2.183180860297908144, -0.4937760292030871079 ) ) ;
#5336 = APPLIED_PERSON_AND_ORGANIZATION_ASSIGNMENT ( #34704, #11877, ( #38779 ) ) ;
#5337 = DIRECTION ( 'NONE',  ( -0.5000000000000012212, -0.3297230132044404183, -0.8008013077932520929 ) ) ;
#5338 = AXIS2_PLACEMENT_3D ( 'NONE', #14846, #11562, #24126 ) ;
#5339 = CARTESIAN_POINT ( 'NONE',  ( 0.5382321766149029685, -1.161161941655082241, 0.5682417262808779901 ) ) ;
#5341 = ORIENTED_EDGE ( 'NONE', *, *, #25341, .T. ) ;
#5340 = VERTEX_POINT ( 'NONE', #20162 ) ;
#5342 = DIRECTION ( 'NONE',  ( 0.4999551463232373427, -0.8660512985181134660, 0.000000000000000000 ) ) ;
#5343 = DIRECTION ( 'NONE',  ( 1.000000000000000000, -2.276539994720207319E-15, 1.138269997360103659E-15 ) ) ;
#5344 = CARTESIAN_POINT ( 'NONE',  ( 0.3709216698330897177, -1.101076713354972370, 0.7945692480043649031 ) ) ;
#5345 = CIRCLE ( 'NONE', #35582, 0.02999999999999999195 ) ;
#5346 = CIRCLE ( 'NONE', #23219, 0.1749999999999999889 ) ;
#5347 = CARTESIAN_POINT ( 'NONE',  ( 0.1852718761952666104, -0.8389489029336036907, 0.1457185345930598341 ) ) ;
#5348 = CARTESIAN_POINT ( 'NONE',  ( 0.2325938614944302874, -1.347997356825076487, 0.5182417262812506475 ) ) ;
#5349 = CARTESIAN_POINT ( 'NONE',  ( 0.2914323826288400254, -1.233685883474753497, -0.5166151207188711680 ) ) ;
#5350 = AXIS2_PLACEMENT_3D ( 'NONE', #13602, #16478, #38077 ) ;
#5351 = CARTESIAN_POINT ( 'NONE',  ( 0.01220820732087773454, -0.4290243149126032329, 0.1652642515859651107 ) ) ;
#5352 = CARTESIAN_POINT ( 'NONE',  ( 0.4165626002392254779, -1.713172581087865076, 0.4267767144038969729 ) ) ;
#5353 = CARTESIAN_POINT ( 'NONE',  ( 0.3327215102334385999, -1.655855958731206279, -0.6422681889546366651 ) ) ;
#5354 = CARTESIAN_POINT ( 'NONE',  ( 0.4584717390208091770, -1.703043547193807017, -0.5155029497116575543 ) ) ;
#5355 = CARTESIAN_POINT ( 'NONE',  ( 0.3227706286670864455, -1.035098858529321930, 0.7546302758663894217 ) ) ;
#5356 = ADVANCED_FACE ( 'NONE', ( #14171 ), #35965, .T. ) ;
#5357 = DIRECTION ( 'NONE',  ( 0.000000000000000000, -0.5877852522924640333, 0.8090169943749540016 ) ) ;
#5358 = CARTESIAN_POINT ( 'NONE',  ( 0.3397077535880360655, -1.654685348432989089, -0.3858274525146618839 ) ) ;
#5359 = CARTESIAN_POINT ( 'NONE',  ( 0.02238826743732924215, -0.2417677220642108493, 0.4518145715460074596 ) ) ;
#5360 = EDGE_CURVE ( 'NONE', #14981, #36888, #34588, .T. ) ;
#5361 = CARTESIAN_POINT ( 'NONE',  ( 0.09104835764951833832, -0.9296025949902090302, 0.8700335549320106221 ) ) ;
#5362 = CARTESIAN_POINT ( 'NONE',  ( 0.04079229832238050191, -0.9851896272356041040, 0.6760550084579007857 ) ) ;
#5363 = EDGE_CURVE ( 'NONE', #7929, #15843, #20799, .T. ) ;
#5364 = PERSON_AND_ORGANIZATION ( #28500, #32463 ) ;
#5365 = CARTESIAN_POINT ( 'NONE',  ( 0.6791199086483500347, -1.400839286187941957, 0.8214794356666539343 ) ) ;
#5366 = ADVANCED_FACE ( 'NONE', ( #37389 ), #11887, .F. ) ;
#5367 = AXIS2_PLACEMENT_3D ( 'NONE', #31690, #35577, #4313 ) ;
#5368 = FACE_OUTER_BOUND ( 'NONE', #32642, .T. ) ;
#5369 = ADVANCED_FACE ( 'NONE', ( #2449 ), #9625, .F. ) ;
#5370 = CARTESIAN_POINT ( 'NONE',  ( 0.04575185649130582288, 0.06505045373102633088, -0.4827759578813190511 ) ) ;
#5371 = ADVANCED_BREP_SHAPE_REPRESENTATION ( '', ( #5167, #27819 ), #11399 ) ;
#5372 = AXIS2_PLACEMENT_3D ( 'NONE', #15044, #24125, #5569 ) ;
#5373 =( BOUNDED_SURFACE ( )  B_SPLINE_SURFACE ( 3, 2, ( 
 ( #919, #10534, #13423 ),
 ( #26597, #4360, #25997 ),
 ( #10351, #10959, #22912 ),
 ( #13624, #23106, #16921 ) ),
 .UNSPECIFIED., .F., .F., .F. ) 
 B_SPLINE_SURFACE_WITH_KNOTS ( ( 4, 4 ),
 ( 3, 3 ),
 ( -3.816391647148975608E-16, 0.002151548051257937220 ),
 ( 0.000000000000000000, 0.5629264174124741782 ),
 .UNSPECIFIED. ) 
 GEOMETRIC_REPRESENTATION_ITEM ( )  RATIONAL_B_SPLINE_SURFACE ( (
 ( 1.000000000000000000, 0.8349447961261939888, 0.8557174614363223242),
 ( 1.000000000000000000, 0.8351496430544862459, 0.8558965277979837527),
 ( 1.000000000000000000, 0.8351234014981824272, 0.8558735888159310079),
 ( 1.000000000000000000, 0.8351226696489343349, 0.8558729490719854116) ) ) 
 REPRESENTATION_ITEM ( '' )  SURFACE ( )  );
#5374 = VECTOR ( 'NONE', #31646, 39.37007874015748854 ) ;
#5375 = FACE_OUTER_BOUND ( 'NONE', #20113, .T. ) ;
#5376 = ORIENTED_EDGE ( 'NONE', *, *, #27253, .F. ) ;
#5377 = LINE ( 'NONE', #18350, #8589 ) ;
#5378 = CARTESIAN_POINT ( 'NONE',  ( 0.04104228371791049379, -0.8021798566012479093, 0.6857248727280681466 ) ) ;
#5379 = AXIS2_PLACEMENT_3D ( 'NONE', #32359, #16752, #29299 ) ;
#5380 = CARTESIAN_POINT ( 'NONE',  ( 0.5632287970188207815, -1.453831970626443981, 0.7328793321959286011 ) ) ;
#5381 = CARTESIAN_POINT ( 'NONE',  ( 0.2875448026290280401, -1.663016392949335565, 0.4537443422403701354 ) ) ;
#5383 = EDGE_LOOP ( 'NONE', ( #14112, #30826, #2571, #17555 ) ) ;
#5382 = CARTESIAN_POINT ( 'NONE',  ( 0.3840624009215719559, -1.828512337075534067, -0.4831679149489520042 ) ) ;
#5384 = CARTESIAN_POINT ( 'NONE',  ( 0.5231597928089396499, -1.148848539795074508, 0.7464108937515090414 ) ) ;
#5386 = ORIENTED_EDGE ( 'NONE', *, *, #138, .F. ) ;
#5385 = ORIENTED_EDGE ( 'NONE', *, *, #9431, .T. ) ;
#5387 = CARTESIAN_POINT ( 'NONE',  ( 0.05005283029671573486, -1.480230044530827183, -0.6492973086577381592 ) ) ;
#5388 = ORIENTED_EDGE ( 'NONE', *, *, #1662, .F. ) ;
#5389 = CARTESIAN_POINT ( 'NONE',  ( 0.3641350647596797163, -1.746033381779148685, -0.5249093166418893341 ) ) ;
#5390 = EDGE_CURVE ( 'NONE', #33903, #1802, #37202, .T. ) ;
#5391 = CARTESIAN_POINT ( 'NONE',  ( -0.3000000000000000999, -2.183180860297908144, -0.4937760292030871079 ) ) ;
#5392 = APPROVAL_STATUS ( 'not_yet_approved' ) ;
#5393 = DIRECTION ( 'NONE',  ( -7.771561172376107616E-16, 7.170354002788761615E-17, -1.000000000000000000 ) ) ;
#5394 = ORIENTED_EDGE ( 'NONE', *, *, #33707, .F. ) ;
#5395 = CARTESIAN_POINT ( 'NONE',  ( 0.2503298133092587974, -0.9500301554809115201, 0.6860627806878819568 ) ) ;
#5396 = CARTESIAN_POINT ( 'NONE',  ( 0.2208413595467774437, -1.374101648533643250, 1.025128890476463051 ) ) ;
#5397 = CARTESIAN_POINT ( 'NONE',  ( 0.4967266092558669799, -1.542263453013163588, 0.5610250318491952770 ) ) ;
#5399 = CARTESIAN_POINT ( 'NONE',  ( -0.002214229356001021481, -0.8555149127599896985, 0.1346324584729416685 ) ) ;
#5398 = CARTESIAN_POINT ( 'NONE',  ( 0.3235114482504872768, -1.763390692376212820, 0.5025175481131797239 ) ) ;
#5400 = CARTESIAN_POINT ( 'NONE',  ( 0.005238257023236751568, -0.9818020271132209542, 0.4509873321765103249 ) ) ;
#5401 = ORIENTED_EDGE ( 'NONE', *, *, #14696, .T. ) ;
#5402 = ORIENTED_EDGE ( 'NONE', *, *, #21576, .T. ) ;
#5403 = CARTESIAN_POINT ( 'NONE',  ( 0.3173336537065408192, -1.761100837031106536, 0.5505159244398599716 ) ) ;
#5404 = CARTESIAN_POINT ( 'NONE',  ( 0.5377357579551512723, -1.280405483484106766, 0.8977613861871198697 ) ) ;
#5405 = FACE_OUTER_BOUND ( 'NONE', #18669, .T. ) ;
#5406 = AXIS2_PLACEMENT_3D ( 'NONE', #36345, #23822, #21130 ) ;
#5407 = CONICAL_SURFACE ( 'NONE', #19241, 0.1500000000000009936, 1.047197551196599630 ) ;
#5408 = CARTESIAN_POINT ( 'NONE',  ( 0.01548846960707292615, 0.5198120922912253805, -0.07362328916738401785 ) ) ;
#5409 = VECTOR ( 'NONE', #2069, 39.37007874015748143 ) ;
#5410 = CARTESIAN_POINT ( 'NONE',  ( -0.02953079040095652960, 0.09152108205202803826, 0.5223162075576412988 ) ) ;
#5411 = CARTESIAN_POINT ( 'NONE',  ( 0.3905383237075480407, -1.946889847283715502, -0.6985532018724728287 ) ) ;
#5412 = CARTESIAN_POINT ( 'NONE',  ( 0.3175115894100313252, -1.184234847365859933, 0.5079114793355775648 ) ) ;
#5413 = CARTESIAN_POINT ( 'NONE',  ( 0.5556676709287090565, -1.190831894458023177, 0.5757950255497361614 ) ) ;
#5414 = ADVANCED_FACE ( 'NONE', ( #24253 ), #27134, .F. ) ;
#5415 = DATE_AND_TIME ( #37307, #18093 ) ;
#5416 = CARTESIAN_POINT ( 'NONE',  ( -0.1151536691905414717, -0.5265970617445885349, 0.3290111518013588698 ) ) ;
#5417 = AXIS2_PLACEMENT_3D ( 'NONE', #4963, #33351, #5160 ) ;
#5418 = EDGE_CURVE ( 'NONE', #354, #24980, #39173, .T. ) ;
#5419 = CARTESIAN_POINT ( 'NONE',  ( 0.1989987071918978556, -2.049746683003707659, -0.6828288310443214604 ) ) ;
#5420 = DIRECTION ( 'NONE',  ( 0.000000000000000000, 0.000000000000000000, 1.000000000000000000 ) ) ;
#5421 = EDGE_CURVE ( 'NONE', #16052, #40212, #26056, .T. ) ;
#5422 = DIRECTION ( 'NONE',  ( 8.881784197001245421E-16, -2.361472542561082612E-16, 1.000000000000000000 ) ) ;
#5423 = ORIENTED_EDGE ( 'NONE', *, *, #9735, .F. ) ;
#5424 = CARTESIAN_POINT ( 'NONE',  ( 0.2209260011871197193, -1.309027873449325918, -0.4125659523519145666 ) ) ;
#5425 = AXIS2_PLACEMENT_3D ( 'NONE', #24881, #222, #21397 ) ;
#5426 = DIRECTION ( 'NONE',  ( -1.000000000000000000, -0.000000000000000000, -0.000000000000000000 ) ) ;
#5427 = CARTESIAN_POINT ( 'NONE',  ( -0.05269191099236000819, -0.004472488327042840883, -0.4686046460979745309 ) ) ;
#5428 = CARTESIAN_POINT ( 'NONE',  ( 0.01030066036532899590, -0.8502541615097699568, 0.2885088771235587712 ) ) ;
#5429 = ORIENTED_EDGE ( 'NONE', *, *, #8033, .F. ) ;
#5430 = DIRECTION ( 'NONE',  ( 1.000000000000000000, -1.544378112879837308E-12, -7.552944938426195655E-13 ) ) ;
#5431 = CIRCLE ( 'NONE', #4154, 0.1000000000000000194 ) ;
#5432 = TOROIDAL_SURFACE ( 'NONE', #34350, 0.5250000000000000222, 0.01499999999999999944 ) ;
#5433 = CARTESIAN_POINT ( 'NONE',  ( 0.05279755784604317492, 0.03988345070377673218, 0.4667183143801719170 ) ) ;
#5434 = EDGE_CURVE ( 'NONE', #33332, #5225, #8300, .T. ) ;
#5435 = CARTESIAN_POINT ( 'NONE',  ( 0.04229974373173520791, -0.4483441990207298611, -0.1365932678717892423 ) ) ;
#5436 = EDGE_CURVE ( 'NONE', #5597, #24586, #3698, .T. ) ;
#5437 = PLANE ( 'NONE',  #14047 ) ;
#5438 = AXIS2_PLACEMENT_3D ( 'NONE', #26834, #8493, #32776 ) ;
#5439 = CARTESIAN_POINT ( 'NONE',  ( 0.3842197382819592666, -1.129692149189392314, 0.6942442540008864071 ) ) ;
#5441 = CARTESIAN_POINT ( 'NONE',  ( 0.4782148911042844452, -1.678884647045308265, 0.5560315867989329419 ) ) ;
#5440 = DIRECTION ( 'NONE',  ( 1.000000000000000000, 6.779273404243070203E-32, -6.162975822039154730E-33 ) ) ;
#5442 = DIRECTION ( 'NONE',  ( 5.551115123125759899E-17, -4.553079989440443628E-16, -1.000000000000000000 ) ) ;
#5443 = ORIENTED_EDGE ( 'NONE', *, *, #35326, .T. ) ;
#5444 = EDGE_CURVE ( 'NONE', #26723, #478, #40270, .T. ) ;
#5445 = CARTESIAN_POINT ( 'NONE',  ( 0.2137558955837162433, -0.8305973034474390948, 0.6882441447716853844 ) ) ;
#5446 = EDGE_LOOP ( 'NONE', ( #2196, #5000, #22033, #8564 ) ) ;
#5447 = VECTOR ( 'NONE', #9079, 39.37007874015748143 ) ;
#5448 = DIRECTION ( 'NONE',  ( -0.4999999999999981126, 0.6509737717187621397, -0.5711682313769305130 ) ) ;
#5449 = ADVANCED_FACE ( 'NONE', ( #36775 ), #8394, .F. ) ;
#5450 = CARTESIAN_POINT ( 'NONE',  ( 0.4430914525986213715, -1.573752655959022695, 0.5975272644295865909 ) ) ;
#5452 = CARTESIAN_POINT ( 'NONE',  ( 0.5670143714999978934, -1.627296631171844643, 0.5238801071547340982 ) ) ;
#5451 = CARTESIAN_POINT ( 'NONE',  ( -0.03654364704248686674, -0.4542255574219898895, 0.2354487068768213731 ) ) ;
#5453 = CARTESIAN_POINT ( 'NONE',  ( -0.1107910466892926965, -0.04310840302198015728, 0.09999999999999895084 ) ) ;
#5454 = ORIENTED_EDGE ( 'NONE', *, *, #7418, .T. ) ;
#5455 = CARTESIAN_POINT ( 'NONE',  ( 0.3660264286422114655, -1.617698911701153541, -0.3269368557715229273 ) ) ;
#5456 = ORIENTED_EDGE ( 'NONE', *, *, #13655, .F. ) ;
#5457 = CARTESIAN_POINT ( 'NONE',  ( 0.4013789418293162159, -1.744061236993332598, -0.3095045109458399168 ) ) ;
#5458 = CARTESIAN_POINT ( 'NONE',  ( 0.3295425949762220696, -1.070172357806076890, 0.7949539627233549455 ) ) ;
#5459 = CARTESIAN_POINT ( 'NONE',  ( 0.4805909393811602093, -1.666072907763637145, 0.5622759738902064486 ) ) ;
#5460 = DIRECTION ( 'NONE',  ( 1.000000000000000000, 0.000000000000000000, 0.000000000000000000 ) ) ;
#5461 = DIRECTION ( 'NONE',  ( 1.000000000000000000, 2.341930812374887555E-31, -1.664003471950578127E-31 ) ) ;
#5462 = CARTESIAN_POINT ( 'NONE',  ( 0.5409306160700753097, -1.629405757603852756, 0.4283118798799024907 ) ) ;
#5463 = AXIS2_PLACEMENT_3D ( 'NONE', #11018, #23576, #17383 ) ;
#5464 = LINE ( 'NONE', #24831, #27942 ) ;
#5465 = CARTESIAN_POINT ( 'NONE',  ( 1.530770926392632502E-17, 0.06117178301711245075, 0.1249999999999993477 ) ) ;
#5466 = CARTESIAN_POINT ( 'NONE',  ( 0.3337757566908341467, -0.8338946305499669309, 0.7209303476996544724 ) ) ;
#5467 = CIRCLE ( 'NONE', #6795, 0.1249999999999999584 ) ;
#5468 = AXIS2_PLACEMENT_3D ( 'NONE', #22627, #34333, #28583 ) ;
#5469 = CARTESIAN_POINT ( 'NONE',  ( 0.07954607876224152607, -1.328936092439369832, 0.4736269073421923714 ) ) ;
#5470 = CARTESIAN_POINT ( 'NONE',  ( 0.4809559340294914387, -1.681307585311514030, -0.4166691164814795845 ) ) ;
#5471 = EDGE_CURVE ( 'NONE', #21617, #17567, #20965, .T. ) ;
#5472 = CARTESIAN_POINT ( 'NONE',  ( 0.6250251996679087041, -1.551063519682329916, -0.6012742504684129852 ) ) ;
#5473 = CARTESIAN_POINT ( 'NONE',  ( 0.04047043078435960672, 0.2415826219374435924, 0.4392104278743103052 ) ) ;
#5474 = CARTESIAN_POINT ( 'NONE',  ( 0.6699292074404746833, -1.569526485364061807, 0.6071573546319920522 ) ) ;
#5475 = EDGE_CURVE ( 'NONE', #23598, #19341, #7653, .T. ) ;
#5476 = DIRECTION ( 'NONE',  ( 0.000000000000000000, 1.000000000000000000, 1.566396143878659165E-12 ) ) ;
#5477 = VECTOR ( 'NONE', #9786, 39.37007874015748143 ) ;
#5478 = CARTESIAN_POINT ( 'NONE',  ( -0.1443922129835731594, -0.5166151207188711680, 0.3749999999999999445 ) ) ;
#5479 = VECTOR ( 'NONE', #5163, 39.37007874015748854 ) ;
#5480 = ORIENTED_EDGE ( 'NONE', *, *, #25219, .T. ) ;
#5481 = CARTESIAN_POINT ( 'NONE',  ( 0.07120675875603865723, -0.8149881486554784171, 0.8228864848196146831 ) ) ;
#5482 = CARTESIAN_POINT ( 'NONE',  ( 0.4054951491981567679, -1.758726281608485875, -0.5878757131129308533 ) ) ;
#5483 = CARTESIAN_POINT ( 'NONE',  ( 0.4186432780919986940, -1.612034538517058246, -0.6668481824684705517 ) ) ;
#5484 = DIRECTION ( 'NONE',  ( 0.8660512985181134660, 0.4999551463232372317, 0.000000000000000000 ) ) ;
#5485 = VERTEX_POINT ( 'NONE', #33485 ) ;
#5486 = ORIENTED_EDGE ( 'NONE', *, *, #31048, .T. ) ;
#5487 = DIRECTION ( 'NONE',  ( -1.000000000000000000, -0.000000000000000000, -0.000000000000000000 ) ) ;
#5488 = CARTESIAN_POINT ( 'NONE',  ( 0.3540817610093318635, -1.633452470505663667, 0.5182417262812423209 ) ) ;
#5489 = EDGE_CURVE ( 'NONE', #38598, #19021, #16783, .T. ) ;
#5490 = DIRECTION ( 'NONE',  ( 0.000000000000000000, 0.000000000000000000, 1.000000000000000000 ) ) ;
#5491 = VECTOR ( 'NONE', #32208, 39.37007874015748854 ) ;
#5492 = CARTESIAN_POINT ( 'NONE',  ( 0.4465842785464451681, -1.213871555848032191, 0.7431748963014650489 ) ) ;
#5493 = APPLIED_PERSON_AND_ORGANIZATION_ASSIGNMENT ( #36431, #33337, ( #11608 ) ) ;
#5495 = ORIENTED_EDGE ( 'NONE', *, *, #2383, .T. ) ;
#5494 = CARTESIAN_POINT ( 'NONE',  ( -0.08000000000000000167, -2.041899626011815183, -0.6359449730384926225 ) ) ;
#5496 = CARTESIAN_POINT ( 'NONE',  ( 0.4679067357895266843, -1.070896998011005019, 0.6479521087143890190 ) ) ;
#5497 = ORIENTED_EDGE ( 'NONE', *, *, #11148, .T. ) ;
#5498 = ADVANCED_FACE ( 'NONE', ( #15392 ), #40487, .F. ) ;
#5499 = SPHERICAL_SURFACE ( 'NONE', #9938, 0.01499999999999999944 ) ;
#5500 = VERTEX_POINT ( 'NONE', #21771 ) ;
#5501 = DIRECTION ( 'NONE',  ( 1.000000000000000000, 6.779273404243070203E-32, 4.314083075427408311E-32 ) ) ;
#5502 = ORIENTED_EDGE ( 'NONE', *, *, #28027, .F. ) ;
#5503 = CIRCLE ( 'NONE', #17353, 0.1849999999999994982 ) ;
#5504 = CARTESIAN_POINT ( 'NONE',  ( 0.3557947951631240113, -1.622273835114473872, 0.5692848210717039725 ) ) ;
#5506 = CARTESIAN_POINT ( 'NONE',  ( 0.1763220507667064563, -0.5650253974486517672, -0.04914117235521991284 ) ) ;
#5505 = CARTESIAN_POINT ( 'NONE',  ( 0.06671723372763513349, -0.6968592392116272904, -0.001943235594188709708 ) ) ;
#5507 = FACE_OUTER_BOUND ( 'NONE', #18611, .T. ) ;
#5508 = ORIENTED_EDGE ( 'NONE', *, *, #37754, .T. ) ;
#5509 = EDGE_LOOP ( 'NONE', ( #15231, #30470, #20552, #39415, #3368 ) ) ;
#5510 = CARTESIAN_POINT ( 'NONE',  ( 0.5218509088173163279, -1.137553602289696819, 0.6585442127631569997 ) ) ;
#5512 = ORIENTED_EDGE ( 'NONE', *, *, #14966, .F. ) ;
#5511 = B_SPLINE_CURVE_WITH_KNOTS ( 'NONE', 3,
 ( #38263, #677, #32702, #26155, #29223, #3725 ),
 .UNSPECIFIED., .F., .F.,
 ( 4, 2, 4 ),
 ( 3.469446951953614189E-18, 0.0006014525054105407170, 0.001202905010821077965 ),
 .UNSPECIFIED. ) ;
#5513 = CIRCLE ( 'NONE', #24593, 0.1000000000000000194 ) ;
#5514 = CARTESIAN_POINT ( 'NONE',  ( 0.2484378334537183652, -1.581318528659484191, -0.3509054470090272604 ) ) ;
#5515 = LINE ( 'NONE', #24876, #19154 ) ;
#5516 = CIRCLE ( 'NONE', #34445, 0.1000000000000000194 ) ;
#5517 = CARTESIAN_POINT ( 'NONE',  ( 0.3843371407211308433, -1.261522862150258995, 0.5783999743260659354 ) ) ;
#5518 = CARTESIAN_POINT ( 'NONE',  ( 0.0006028978349475794165, -1.952399615628604757, -0.3318938993356948530 ) ) ;
#5519 = B_SPLINE_CURVE_WITH_KNOTS ( 'NONE', 3,
 ( #6705, #31819, #15586, #38181, #10007, #22579, #6910, #32016, #16381, #28921, #786, #13296 ),
 .UNSPECIFIED., .F., .F.,
 ( 4, 2, 2, 2, 2, 4 ),
 ( 0.001537871260908298121, 0.002663464713205636845, 0.003789058165502975570, 0.004351854891651643631, 0.004914651617800311692, 0.006040245070097646947 ),
 .UNSPECIFIED. ) ;
#5520 = DIRECTION ( 'NONE',  ( 0.000000000000000000, -0.5877852522924607026, -0.8090169943749563330 ) ) ;
#5521 = CARTESIAN_POINT ( 'NONE',  ( -0.1642263573060748216, 0.5103503758725048689, 0.3090632479873839378 ) ) ;
#5522 = CARTESIAN_POINT ( 'NONE',  ( 0.4136294883733862005, -1.694877849074643672, 0.4182417262808776903 ) ) ;
#5523 = DIRECTION ( 'NONE',  ( 0.000000000000000000, -2.697841949839120927E-14, -1.000000000000000000 ) ) ;
#5524 = CARTESIAN_POINT ( 'NONE',  ( 0.3924513946351673721, -1.141110873382124913, 0.4807468720547258823 ) ) ;
#5525 = CARTESIAN_POINT ( 'NONE',  ( 0.05447883519600660307, -1.297772118441766542, 0.6273051521731305424 ) ) ;
#5526 = APPROVAL_STATUS ( 'not_yet_approved' ) ;
#5527 = AXIS2_PLACEMENT_3D ( 'NONE', #2340, #40374, #24759 ) ;
#5528 = EDGE_CURVE ( 'NONE', #15019, #39255, #31307, .T. ) ;
#5529 = CIRCLE ( 'NONE', #20679, 0.1000000000000000194 ) ;
#5530 = CARTESIAN_POINT ( 'NONE',  ( 0.4668492548151236265, -1.130293246669365370, 0.4644915327382355685 ) ) ;
#5531 = CARTESIAN_POINT ( 'NONE',  ( 0.5623916231413996769, -1.181299486036711199, 0.6057417262809813296 ) ) ;
#5532 = CARTESIAN_POINT ( 'NONE',  ( 0.5724688059860902900, -1.573362539590891229, -0.5731659206011648910 ) ) ;
#5533 = VECTOR ( 'NONE', #11107, 39.37007874015748143 ) ;
#5534 = CIRCLE ( 'NONE', #7494, 0.04249999999999994754 ) ;
#5535 = APPROVAL_PERSON_ORGANIZATION ( #22617, #26276, #35146 ) ;
#5536 = CARTESIAN_POINT ( 'NONE',  ( 0.0001449614208580852083, -0.5613537431353852192, -0.06918609228517788590 ) ) ;
#5537 = CARTESIAN_POINT ( 'NONE',  ( 0.3247324306352935563, -1.759421949583405365, 0.4854534786567430427 ) ) ;
#5538 = CARTESIAN_POINT ( 'NONE',  ( 0.0006674789801655854095, -0.4508007590529634068, 0.2320570027856783679 ) ) ;
#5539 = LINE ( 'NONE', #27976, #4671 ) ;
#5540 = CIRCLE ( 'NONE', #18032, 0.01000000000000009388 ) ;
#5541 = ORIENTED_EDGE ( 'NONE', *, *, #29814, .F. ) ;
#5542 = EDGE_LOOP ( 'NONE', ( #25312, #11118, #8858, #14251 ) ) ;
#5543 = CARTESIAN_POINT ( 'NONE',  ( -0.1062912471183375118, -0.4837944836747087862, 0.1097058945452914075 ) ) ;
#5544 = ORIENTED_EDGE ( 'NONE', *, *, #23991, .T. ) ;
#5545 = CARTESIAN_POINT ( 'NONE',  ( -2.070754768975508586, -0.09959325338431662678, 0.3600000000000021516 ) ) ;
#5546 = CARTESIAN_POINT ( 'NONE',  ( -0.1111952754772430191, -0.5081759048641460996, 0.1244868412816072106 ) ) ;
#5548 = ORIENTED_EDGE ( 'NONE', *, *, #3465, .T. ) ;
#5547 = CARTESIAN_POINT ( 'NONE',  ( 0.5985082606850495868, -1.473464502187743941, 0.6023744451300401259 ) ) ;
#5549 = EDGE_LOOP ( 'NONE', ( #40368, #31161, #39101, #32810, #26372 ) ) ;
#5550 = FACE_OUTER_BOUND ( 'NONE', #16484, .T. ) ;
#5551 = ORIENTED_EDGE ( 'NONE', *, *, #33769, .F. ) ;
#5552 = CARTESIAN_POINT ( 'NONE',  ( -0.001590528238760143074, -0.5283317060040648716, 0.1648872331919332412 ) ) ;
#5554 = CARTESIAN_POINT ( 'NONE',  ( 0.1199895787080857840, -1.258723611029123557, 0.6044653572558237320 ) ) ;
#5553 = CARTESIAN_POINT ( 'NONE',  ( 0.1943609810622756173, -1.255083399771677266, -0.3178472134378122482 ) ) ;
#5555 = DIRECTION ( 'NONE',  ( 0.000000000000000000, 0.000000000000000000, -1.000000000000000000 ) ) ;
#5556 = APPROVAL_DATE_TIME ( #37035, #16070 ) ;
#5557 = CIRCLE ( 'NONE', #10187, 0.08000000000000000167 ) ;
#5558 = CARTESIAN_POINT ( 'NONE',  ( -0.1630570426857044508, 0.4726602372414858144, 0.3374198529391160273 ) ) ;
#5560 = ORIENTED_EDGE ( 'NONE', *, *, #19480, .F. ) ;
#5559 = VERTEX_POINT ( 'NONE', #31241 ) ;
#5561 = AXIS2_PLACEMENT_3D ( 'NONE', #12825, #31738, #25386 ) ;
#5562 = CARTESIAN_POINT ( 'NONE',  ( 0.3612865554702208715, -1.133767101051816883, 0.6202026458649380070 ) ) ;
#5563 = CARTESIAN_POINT ( 'NONE',  ( 0.000000000000000000, -0.3458405862425447119, -0.1052451372150005060 ) ) ;
#5564 = CARTESIAN_POINT ( 'NONE',  ( -0.03672309138969633013, -0.4682479968340325094, 0.1092356788912448168 ) ) ;
#5565 = VECTOR ( 'NONE', #35996, 39.37007874015748143 ) ;
#5566 = CARTESIAN_POINT ( 'NONE',  ( 0.4538561152830952738, -1.255326032114347568, 0.8184392061610863411 ) ) ;
#5567 = CIRCLE ( 'NONE', #10155, 0.1050228153667111808 ) ;
#5568 = CARTESIAN_POINT ( 'NONE',  ( 0.1865116958955829740, -0.7545155313687175180, 0.04158996775387410749 ) ) ;
#5569 = DIRECTION ( 'NONE',  ( 0.000000000000000000, 0.000000000000000000, -1.000000000000000000 ) ) ;
#5570 = LOCAL_TIME ( 0, 53, 7.000000000000000000, #6741 ) ;
#5571 = CARTESIAN_POINT ( 'NONE',  ( 0.6011193747858227798, -1.595581932925101976, 0.4276689662439276396 ) ) ;
#5572 = CARTESIAN_POINT ( 'NONE',  ( 0.4116746766561834581, -1.754103855848320626, -0.4360744270256505239 ) ) ;
#5573 = CARTESIAN_POINT ( 'NONE',  ( 0.3860498842613241943, -1.725354837844226052, 0.4274986991496981803 ) ) ;
#5574 = AXIS2_PLACEMENT_3D ( 'NONE', #9366, #21946, #31400 ) ;
#5575 = CARTESIAN_POINT ( 'NONE',  ( -0.01548846960707524721, 0.3772621329472709006, 0.3651003739303413931 ) ) ;
#5576 = PLANE ( 'NONE',  #6732 ) ;
#5577 = DIRECTION ( 'NONE',  ( 0.4999551463232372317, -0.8660512985181135770, 0.000000000000000000 ) ) ;
#5578 = CARTESIAN_POINT ( 'NONE',  ( 0.4085116948120698366, -1.104829239061055013, 0.5999620787602801819 ) ) ;
#5579 = CARTESIAN_POINT ( 'NONE',  ( 0.05999999999999990757, 0.000000000000000000, 0.000000000000000000 ) ) ;
#5580 = DIRECTION ( 'NONE',  ( 1.232595164407830946E-32, 0.2098598043933069257, 0.9777314879352116961 ) ) ;
#5581 = DIRECTION ( 'NONE',  ( -0.000000000000000000, 0.9396926207859070956, 0.3420201433256722101 ) ) ;
#5582 = CARTESIAN_POINT ( 'NONE',  ( 0.008057578236607982475, -0.5544447393747381492, 0.4149153965127375110 ) ) ;
#5583 = CARTESIAN_POINT ( 'NONE',  ( 0.07862385513909125878, -1.240140462211094530, 0.7484620922004757704 ) ) ;
#5584 = DATE_AND_TIME ( #24530, #20719 ) ;
#5585 = CARTESIAN_POINT ( 'NONE',  ( 0.5753152089321617035, -1.233008725051026655, 0.8518361925389578149 ) ) ;
#5586 = VECTOR ( 'NONE', #13157, 39.37007874015748854 ) ;
#5587 = CIRCLE ( 'NONE', #401, 0.1000000000000000194 ) ;
#5588 = CARTESIAN_POINT ( 'NONE',  ( 0.4184753273149498520, -1.633759443312357229, -0.5155029497116575543 ) ) ;
#5589 = CARTESIAN_POINT ( 'NONE',  ( 0.03643058821096969296, -0.08373535757664375689, -0.5050280785339864575 ) ) ;
#5590 = CARTESIAN_POINT ( 'NONE',  ( -0.3000000000000000999, -3.791721498889941255, -0.2726869407194119077 ) ) ;
#5591 = ORIENTED_EDGE ( 'NONE', *, *, #9908, .T. ) ;
#5592 = LINE ( 'NONE', #8889, #38834 ) ;
#5593 = APPLIED_SECURITY_CLASSIFICATION_ASSIGNMENT ( #7563, ( #1014 ) ) ;
#5594 = CARTESIAN_POINT ( 'NONE',  ( 0.03184741477609578930, -0.7213761098217522649, 0.5732232197377126193 ) ) ;
#5595 = CARTESIAN_POINT ( 'NONE',  ( 0.5878605360589412854, -1.491219481631713029, 0.5721084594529655121 ) ) ;
#5597 = VERTEX_POINT ( 'NONE', #36592 ) ;
#5596 = CARTESIAN_POINT ( 'NONE',  ( 0.3476685035120829492, -1.750311407975150280, 0.4514359344836209043 ) ) ;
#5598 = AXIS2_PLACEMENT_3D ( 'NONE', #7003, #26337, #20176 ) ;
#5599 = CARTESIAN_POINT ( 'NONE',  ( 0.6136594321969363053, -1.288375518029639233, 0.6368171400845314967 ) ) ;
#5601 = ORIENTED_EDGE ( 'NONE', *, *, #11715, .T. ) ;
#5600 = VERTEX_POINT ( 'NONE', #11502 ) ;
#5602 = CARTESIAN_POINT ( 'NONE',  ( 0.6687172182925377184, -1.381928324059317426, 0.7472473190455153347 ) ) ;
#5603 = FACE_OUTER_BOUND ( 'NONE', #12081, .T. ) ;
#5604 = CARTESIAN_POINT ( 'NONE',  ( 0.4380553862277722921, -1.229819722584721164, 0.5856983068965045947 ) ) ;
#5605 = B_SPLINE_CURVE_WITH_KNOTS ( 'NONE', 3,
 ( #13495, #10816, #38580, #19864, #32399, #16790 ),
 .UNSPECIFIED., .F., .F.,
 ( 4, 2, 4 ),
 ( 0.001086186341203851033, 0.004311068202048287321, 0.007535950062892723608 ),
 .UNSPECIFIED. ) ;
#5606 = CARTESIAN_POINT ( 'NONE',  ( 0.1890965627226634804, -1.347655541994686068, 0.5182417262812423209 ) ) ;
#5607 = ORIENTED_EDGE ( 'NONE', *, *, #9676, .T. ) ;
#5608 = ADVANCED_FACE ( 'NONE', ( #5507 ), #18165, .T. ) ;
#5609 = CARTESIAN_POINT ( 'NONE',  ( 0.1020195082480463700, -0.7293290528718650023, 0.3482666274738245304 ) ) ;
#5610 = EDGE_CURVE ( 'NONE', #28969, #22322, #28016, .T. ) ;
#5611 = CARTESIAN_POINT ( 'NONE',  ( 0.3059622673449214902, -1.701610228655562773, 0.8344189609799835816 ) ) ;
#5612 = CARTESIAN_POINT ( 'NONE',  ( 0.3795518307925651036, -1.261362786936248037, 0.8506242053835164629 ) ) ;
#5614 = CARTESIAN_POINT ( 'NONE',  ( 0.06954796871655651025, -1.315582234632707515, 0.5182417262812430980 ) ) ;
#5613 = SPHERICAL_SURFACE ( 'NONE', #13844, 0.01499999999999999944 ) ;
#5615 = CARTESIAN_POINT ( 'NONE',  ( 0.01675195241592676923, -1.055683844097430324, 0.6015879664242336222 ) ) ;
#5616 = VERTEX_POINT ( 'NONE', #13927 ) ;
#5617 = VERTEX_POINT ( 'NONE', #19913 ) ;
#5618 = ADVANCED_FACE ( 'NONE', ( #32058 ), #32902, .T. ) ;
#5619 = CARTESIAN_POINT ( 'NONE',  ( -0.1631212487981108517, 0.5067506594879367388, 0.1120476149576248998 ) ) ;
#5620 = CARTESIAN_POINT ( 'NONE',  ( 0.2919827015984412522, -0.8702395470303202485, 0.7938945491903462992 ) ) ;
#5621 = AXIS2_PLACEMENT_3D ( 'NONE', #39189, #23762, #11014 ) ;
#5622 = EDGE_CURVE ( 'NONE', #31054, #40610, #33259, .T. ) ;
#5623 = DIRECTION ( 'NONE',  ( 2.465190328815661892E-32, 1.000000000000000000, 6.656013887802287108E-31 ) ) ;
#5624 = CARTESIAN_POINT ( 'NONE',  ( 0.3690031775293027283, -2.059871137024939625, -0.4867069271398427599 ) ) ;
#5625 = PRODUCT_DEFINITION_FORMATION_WITH_SPECIFIED_SOURCE ( 'ANY', '', #39358, .NOT_KNOWN. ) ;
#5626 = DIRECTION ( 'NONE',  ( 7.771561172376107616E-16, -7.170354002788761615E-17, 1.000000000000000000 ) ) ;
#5627 = DIRECTION ( 'NONE',  ( 0.8660512985181132439, 0.4999551463232376758, 0.000000000000000000 ) ) ;
#5628 = CARTESIAN_POINT ( 'NONE',  ( -0.02000000000000000042, -2.320036485105098301, -0.4341690811493933433 ) ) ;
#5629 = CONICAL_SURFACE ( 'NONE', #17481, 0.1600000000000005584, 1.047197551196598075 ) ;
#5630 = CARTESIAN_POINT ( 'NONE',  ( 0.3597322771628292393, -1.737184542215604033, -0.5031181248198197675 ) ) ;
#5631 = CARTESIAN_POINT ( 'NONE',  ( 0.2618294899476097393, -0.7990503781373888836, 0.5447687035333291794 ) ) ;
#5632 = DATE_AND_TIME ( #36705, #406 ) ;
#5633 =( BOUNDED_SURFACE ( )  B_SPLINE_SURFACE ( 3, 2, ( 
 ( #26197, #23116, #10356 ),
 ( #16132, #37923, #7446 ),
 ( #537, #25790, #19615 ),
 ( #3563, #38314, #6837 ),
 ( #35027, #10143, #12831 ),
 ( #22716, #13631, #16728 ) ),
 .UNSPECIFIED., .F., .F., .F. ) 
 B_SPLINE_SURFACE_WITH_KNOTS ( ( 4, 2, 4 ),
 ( 3, 3 ),
 ( 0.000000000000000000, 0.0006488076353390061744, 0.001297615270678012349 ),
 ( 0.000000000000000000, 1.000000000000000000 ),
 .UNSPECIFIED. ) 
 GEOMETRIC_REPRESENTATION_ITEM ( )  RATIONAL_B_SPLINE_SURFACE ( (
 ( 1.000000000000000000, 0.8219793159978276975, 1.000000000000000000),
 ( 1.000000000000000000, 0.8058033770605222967, 1.000000000000000000),
 ( 1.000000000000000000, 0.7882677358999856665, 1.000000000000000000),
 ( 1.000000000000000000, 0.7498419410649512784, 1.000000000000000000),
 ( 1.000000000000000000, 0.7296076275689642454, 1.000000000000000000),
 ( 1.000000000000000000, 0.7071067811865446862, 1.000000000000000000) ) ) 
 REPRESENTATION_ITEM ( '' )  SURFACE ( )  );
#5634 = CARTESIAN_POINT ( 'NONE',  ( 0.5772157698596116493, -1.612763119636421383, 0.5867784257054611263 ) ) ;
#5635 = EDGE_CURVE ( 'NONE', #6325, #13571, #40299, .T. ) ;
#5636 = APPLIED_PERSON_AND_ORGANIZATION_ASSIGNMENT ( #31452, #6344, ( #33155 ) ) ;
#5637 = CARTESIAN_POINT ( 'NONE',  ( 0.3662805103927266881, -2.019948479727926571, -0.5051633158473676222 ) ) ;
#5638 = LINE ( 'NONE', #20896, #7679 ) ;
#5639 = CARTESIAN_POINT ( 'NONE',  ( -0.02881329448201062557, -0.3393412917002096019, -0.3647544004888587099 ) ) ;
#5640 = ORIENTED_EDGE ( 'NONE', *, *, #30794, .F. ) ;
#5641 = CARTESIAN_POINT ( 'NONE',  ( -0.08978098643734171158, 0.000000000000000000, 0.000000000000000000 ) ) ;
#5642 = CARTESIAN_POINT ( 'NONE',  ( -0.04575334816098278190, -0.2311426348461427527, 0.4288046462019637350 ) ) ;
#5643 = CARTESIAN_POINT ( 'NONE',  ( 0.2698036132048247104, -0.9625005881386677897, 0.7146062034794288254 ) ) ;
#5644 = EDGE_LOOP ( 'NONE', ( #11088, #31673, #20106, #7309, #24098 ) ) ;
#5645 = AXIS2_PLACEMENT_3D ( 'NONE', #20462, #14081, #17585 ) ;
#5646 = CARTESIAN_POINT ( 'NONE',  ( -0.02881302694830004812, 0.06014213504333749266, -0.4945521340962376056 ) ) ;
#5647 = CARTESIAN_POINT ( 'NONE',  ( 0.09909909854404998220, -1.020393566678226005, 0.7132605819709517680 ) ) ;
#5649 = EDGE_LOOP ( 'NONE', ( #13473, #23420, #6721, #11652 ) ) ;
#5648 = ORIENTED_EDGE ( 'NONE', *, *, #23113, .F. ) ;
#5650 = FACE_OUTER_BOUND ( 'NONE', #31232, .T. ) ;
#5651 = CARTESIAN_POINT ( 'NONE',  ( 0.04047043078436458191, -0.06271696546453207899, 0.4973274026419853278 ) ) ;
#5652 = ORGANIZATION ( 'NAUO-ORG8', 'UNSPECIFIED', 'UNSPECIFIED' ) ;
#5653 = CARTESIAN_POINT ( 'NONE',  ( 0.7426951793279046310, -1.510662807742832348, 0.6358527240479500131 ) ) ;
#5654 = CARTESIAN_POINT ( 'NONE',  ( 0.2456699162554547011, -1.579418306085378143, -0.3207381830095928921 ) ) ;
#5655 = CARTESIAN_POINT ( 'NONE',  ( 0.4691437399998080737, -1.240809866259031002, 0.5800955640248587342 ) ) ;
#5657 = CARTESIAN_POINT ( 'NONE',  ( 0.008480392309630364542, -0.9466935224705154139, 0.1457226493340757767 ) ) ;
#5656 = DIRECTION ( 'NONE',  ( 0.000000000000000000, 3.885780586188049371E-16, 1.000000000000000000 ) ) ;
#5658 = CARTESIAN_POINT ( 'NONE',  ( 0.03303737228521275160, -0.3731855291841249533, -0.3634704002369493203 ) ) ;
#5659 = ORIENTED_EDGE ( 'NONE', *, *, #35292, .F. ) ;
#5660 = EDGE_LOOP ( 'NONE', ( #24762, #35441, #20112 ) ) ;
#5661 = DIRECTION ( 'NONE',  ( 0.4220386480983009392, 0.000000000000000000, 0.9065778397420479751 ) ) ;
#5662 = ORIENTED_EDGE ( 'NONE', *, *, #18862, .F. ) ;
#5663 = EDGE_CURVE ( 'NONE', #20453, #40011, #1118, .T. ) ;
#5664 = CARTESIAN_POINT ( 'NONE',  ( 0.6728294579378611973, -1.556433697830899687, 0.6139941624117232211 ) ) ;
#5665 = CARTESIAN_POINT ( 'NONE',  ( 0.4436065027728119947, -1.573014041395296436, 0.6136667051735021916 ) ) ;
#5667 = CARTESIAN_POINT ( 'NONE',  ( 0.5722925517058021772, -1.623342969514509182, 0.4835929536261462380 ) ) ;
#5666 = CARTESIAN_POINT ( 'NONE',  ( -0.3000000000000000999, -4.385325017590463226, -0.5985264029706663935 ) ) ;
#5668 = CARTESIAN_POINT ( 'NONE',  ( 0.4870042317405073873, -1.170188898918880893, 0.4224809036138285623 ) ) ;
#5669 = CARTESIAN_POINT ( 'NONE',  ( 0.3699999999999786793, -2.166079853131637201, -0.5407606602423821185 ) ) ;
#5670 = EDGE_LOOP ( 'NONE', ( #19353, #30949, #10333, #30249 ) ) ;
#5671 = EDGE_CURVE ( 'NONE', #36494, #2835, #35954, .T. ) ;
#5672 = CARTESIAN_POINT ( 'NONE',  ( 0.4357251440965448919, -1.593374815047817750, -0.6129939512658331147 ) ) ;
#5673 = CARTESIAN_POINT ( 'NONE',  ( 0.3988316749348294610, -2.033309342251372165, -0.2786258215130219540 ) ) ;
#5674 = EDGE_CURVE ( 'NONE', #33666, #6106, #18245, .T. ) ;
#5675 = CARTESIAN_POINT ( 'NONE',  ( 0.5488630487633856525, -1.446887613430648090, 0.7481907029641444717 ) ) ;
#5676 = CARTESIAN_POINT ( 'NONE',  ( 0.4590038926919776108, -1.675844875513867294, 0.4569803339803656939 ) ) ;
#5677 = CARTESIAN_POINT ( 'NONE',  ( 0.4234909963964844648, -1.082397635545747638, -0.5155029497116575543 ) ) ;
#5678 = ORIENTED_EDGE ( 'NONE', *, *, #27507, .T. ) ;
#5679 = CARTESIAN_POINT ( 'NONE',  ( -0.04154009738085488734, 0.4416556227939107404, 0.1617111092119882798 ) ) ;
#5680 = DIRECTION ( 'NONE',  ( -7.771561172376097755E-16, -7.170354002788760383E-17, 1.000000000000000000 ) ) ;
#5681 = DIRECTION ( 'NONE',  ( 0.8660512985181126888, 0.4999551463232385085, 0.000000000000000000 ) ) ;
#5682 = CARTESIAN_POINT ( 'NONE',  ( -0.08978098643734171158, -4.231851475640401875E-16, 0.3698489655878013371 ) ) ;
#5683 = AXIS2_PLACEMENT_3D ( 'NONE', #39461, #8197, #36378 ) ;
#5684 = CARTESIAN_POINT ( 'NONE',  ( 0.3679852976493193095, -0.8933044249262621639, 0.7616870389678419562 ) ) ;
#5685 = CARTESIAN_POINT ( 'NONE',  ( -0.02881329448201175314, 0.3393412917002295859, 0.3647544004888629288 ) ) ;
#5686 = ADVANCED_FACE ( 'NONE', ( #2012 ), #28461, .F. ) ;
#5687 = CARTESIAN_POINT ( 'NONE',  ( 0.009064896295912058116, -1.006671522247063022, 0.5204707375227085597 ) ) ;
#5688 = EDGE_CURVE ( 'NONE', #34185, #38544, #40590, .T. ) ;
#5689 = CARTESIAN_POINT ( 'NONE',  ( 0.6093641782434934262, -1.558562247244742016, -0.4097570653135631513 ) ) ;
#5690 = DIRECTION ( 'NONE',  ( 0.000000000000000000, 0.000000000000000000, -1.000000000000000000 ) ) ;
#5691 = CARTESIAN_POINT ( 'NONE',  ( -2.070903537920736781, -2.678131749591557309, 0.6057417262810178560 ) ) ;
#5692 = CIRCLE ( 'NONE', #22821, 0.01500000000000001159 ) ;
#5693 = CARTESIAN_POINT ( 'NONE',  ( -0.02000000000000000042, -2.183180860297908144, -0.4937760292030871079 ) ) ;
#5694 = ORIENTED_EDGE ( 'NONE', *, *, #35631, .F. ) ;
#5695 = FACE_OUTER_BOUND ( 'NONE', #34716, .T. ) ;
#5696 = CARTESIAN_POINT ( 'NONE',  ( 0.3955714498361173059, -1.685393650580701674, -0.6248087526158117022 ) ) ;
#5697 = CARTESIAN_POINT ( 'NONE',  ( 0.2456699162554547011, -1.579418306085378143, -0.3207381830095928921 ) ) ;
#5698 = DIRECTION ( 'NONE',  ( 0.8660512985181132439, 0.4999551463232376758, 0.000000000000000000 ) ) ;
#5699 = ORIENTED_EDGE ( 'NONE', *, *, #8406, .F. ) ;
#5700 = CARTESIAN_POINT ( 'NONE',  ( 0.4697623592636159806, -1.061459377010899541, -0.6056023639864148711 ) ) ;
#5701 = ORIENTED_EDGE ( 'NONE', *, *, #26598, .T. ) ;
#5702 = CARTESIAN_POINT ( 'NONE',  ( 0.3709243015156632461, -1.147037477812652195, 0.6031947222724455271 ) ) ;
#5703 = CARTESIAN_POINT ( 'NONE',  ( -0.2399999999999999079, -3.478759481804464038, -0.3573324461326447543 ) ) ;
#5704 = CARTESIAN_POINT ( 'NONE',  ( 0.03875673594170014197, 0.3062691647558835606, -0.3649083695375474057 ) ) ;
#5705 = CARTESIAN_POINT ( 'NONE',  ( 0.4551546549851303580, -1.225298050788209414, 0.7259450990592548614 ) ) ;
#5707 = ORIENTED_EDGE ( 'NONE', *, *, #20111, .F. ) ;
#5706 = DIRECTION ( 'NONE',  ( -1.000000000000000000, 0.000000000000000000, 0.000000000000000000 ) ) ;
#5708 = CARTESIAN_POINT ( 'NONE',  ( 0.3711835952353229051, -0.9982156264046870842, 0.6339317236198600547 ) ) ;
#5709 = AXIS2_PLACEMENT_3D ( 'NONE', #29066, #4168, #32561 ) ;
#5710 = EDGE_LOOP ( 'NONE', ( #19824, #13050, #14817, #5134 ) ) ;
#5711 = CALENDAR_DATE ( 2026, 13, 10 ) ;
#5712 = DIRECTION ( 'NONE',  ( 0.8660512985181140211, 0.4999551463232362880, 0.000000000000000000 ) ) ;
#5713 = ORIENTED_EDGE ( 'NONE', *, *, #25352, .F. ) ;
#5714 = CARTESIAN_POINT ( 'NONE',  ( 0.01054817777343857940, -0.5296544771352952319, 0.1457185332388703236 ) ) ;
#5715 = ADVANCED_FACE ( 'NONE', ( #20743 ), #18039, .F. ) ;
#5716 = ORIENTED_EDGE ( 'NONE', *, *, #15694, .T. ) ;
#5717 = CARTESIAN_POINT ( 'NONE',  ( 0.03638364785045244965, -0.5559812057408780595, 0.2471708904571671417 ) ) ;
#5719 = CARTESIAN_POINT ( 'NONE',  ( 0.1863655194128141790, -0.6771278842445480617, -0.02150419001686059914 ) ) ;
#5718 = CARTESIAN_POINT ( 'NONE',  ( 0.06682908180107070828, -0.6872203660146791737, -0.001923513761143209400 ) ) ;
#5720 = DIRECTION ( 'NONE',  ( -6.162975822039154730E-33, 0.000000000000000000, -1.000000000000000000 ) ) ;
#5721 = EDGE_CURVE ( 'NONE', #28382, #14767, #29332, .T. ) ;
#5722 = B_SPLINE_CURVE_WITH_KNOTS ( 'NONE', 3,
 ( #30388, #27103, #11672, #33662, #5268, #18040, #29992, #14758, #11860, #2218 ),
 .UNSPECIFIED., .F., .F.,
 ( 4, 2, 2, 2, 4 ),
 ( 2.928550287019058723E-17, 0.0003680060388662723830, 0.0007360120777325154925, 0.001104018116598758656, 0.001472024155465001712 ),
 .UNSPECIFIED. ) ;
#5723 = ORIENTED_EDGE ( 'NONE', *, *, #19465, .T. ) ;
#5724 = EDGE_LOOP ( 'NONE', ( #11049, #30551 ) ) ;
#5725 = CARTESIAN_POINT ( 'NONE',  ( 0.3308510979688408238, -0.9309371998241751101, 0.6266194620381673186 ) ) ;
#5726 = CARTESIAN_POINT ( 'NONE',  ( 0.5536301873218408831, -1.511148576249882192, 0.5861183057439698363 ) ) ;
#5727 = EDGE_LOOP ( 'NONE', ( #36317, #31719, #31137, #19503 ) ) ;
#5728 = CYLINDRICAL_SURFACE ( 'NONE', #35756, 0.5400000000000017009 ) ;
#5729 = DIRECTION ( 'NONE',  ( -2.465190328815661892E-32, -1.000000000000000000, -6.656013887802287108E-31 ) ) ;
#5730 = FACE_OUTER_BOUND ( 'NONE', #12863, .T. ) ;
#5731 = EDGE_CURVE ( 'NONE', #36006, #19301, #33266, .T. ) ;
#5732 = CARTESIAN_POINT ( 'NONE',  ( -0.1212185660208173754, -0.5071153786978156441, 0.3078438575813711164 ) ) ;
#5733 = CARTESIAN_POINT ( 'NONE',  ( -0.06034227824829735409, 0.05439570041090503044, 0.1249999999999993477 ) ) ;
#5734 = CARTESIAN_POINT ( 'NONE',  ( 0.05999999999999990757, 0.7171888913565960255, -0.2950238883388468514 ) ) ;
#5735 = CARTESIAN_POINT ( 'NONE',  ( 0.1089214313634646741, -1.279151142302971778, 0.6159407968199497319 ) ) ;
#5736 = CARTESIAN_POINT ( 'NONE',  ( -0.2399999999999999079, -1.891808285041389093, -0.4498908273618595910 ) ) ;
#5737 = CARTESIAN_POINT ( 'NONE',  ( 1.365923996832131609E-16, -0.9481888444201336252, 0.1622877746734860682 ) ) ;
#5738 = PERSON_AND_ORGANIZATION ( #28500, #32463 ) ;
#5739 = EDGE_CURVE ( 'NONE', #39763, #33249, #28080, .T. ) ;
#5740 = EDGE_CURVE ( 'NONE', #20593, #33666, #14956, .T. ) ;
#5741 = CARTESIAN_POINT ( 'NONE',  ( 0.4727378706625928184, -1.129322216815012325, 0.4725836227227263597 ) ) ;
#5742 = CARTESIAN_POINT ( 'NONE',  ( 0.4580986008033318679, -1.241505888743733577, 0.6057417262809813296 ) ) ;
#5743 = CARTESIAN_POINT ( 'NONE',  ( -0.2900000000000005906, 0.5182417262804733804, 0.1000000000000000749 ) ) ;
#5744 = CARTESIAN_POINT ( 'NONE',  ( 0.1873045545006853108, -1.548079183614573306, 0.6123590530682133659 ) ) ;
#5745 = CARTESIAN_POINT ( 'NONE',  ( 0.2615957342988080581, -1.678037082261113921, 0.5379576451024024042 ) ) ;
#5746 = PLANE ( 'NONE',  #2816 ) ;
#5747 = CARTESIAN_POINT ( 'NONE',  ( 0.1909286924077253367, -1.257064795538238577, -0.3194715457588298002 ) ) ;
#5748 = CIRCLE ( 'NONE', #16283, 0.01999999999999927530 ) ;
#5749 = VERTEX_POINT ( 'NONE', #24424 ) ;
#5750 = EDGE_LOOP ( 'NONE', ( #23965, #1059, #23365, #6251 ) ) ;
#5751 = CARTESIAN_POINT ( 'NONE',  ( -0.1044436713285770701, -0.4741860147766130962, 0.09550516381870584326 ) ) ;
#5752 = ORIENTED_EDGE ( 'NONE', *, *, #24141, .F. ) ;
#5753 = CARTESIAN_POINT ( 'NONE',  ( -0.1873388932668320073, 0.5325605939836577374, 0.09999999999999989453 ) ) ;
#5754 = CARTESIAN_POINT ( 'NONE',  ( 0.6252338399778394340, -1.468100857423625838, 0.5182417262812428760 ) ) ;
#5756 = ORIENTED_EDGE ( 'NONE', *, *, #11155, .F. ) ;
#5755 = CARTESIAN_POINT ( 'NONE',  ( 0.001385844221826001152, -0.5662722994882537497, 0.04168102574831390045 ) ) ;
#5757 = ORIENTED_EDGE ( 'NONE', *, *, #24584, .T. ) ;
#5758 = DIRECTION ( 'NONE',  ( -1.000000000000000000, -0.000000000000000000, -0.000000000000000000 ) ) ;
#5759 = ORIENTED_EDGE ( 'NONE', *, *, #12225, .T. ) ;
#5760 = CARTESIAN_POINT ( 'NONE',  ( 0.2691513416950872539, -1.675382000085723133, 0.6134701876119651454 ) ) ;
#5762 = CARTESIAN_POINT ( 'NONE',  ( 0.1025666744235219086, -1.287399128809481930, 0.6111874459470316712 ) ) ;
#5761 = CARTESIAN_POINT ( 'NONE',  ( 0.4341051395151963033, -1.228754679272166861, 0.6047424332237795186 ) ) ;
#5763 = LINE ( 'NONE', #33527, #29238 ) ;
#5764 = ITEM_DEFINED_TRANSFORMATION ( 'NONE', 'NONE', #20656,  #27819 ) ;
#5765 = EDGE_CURVE ( 'NONE', #22491, #28751, #25406, .T. ) ;
#5766 = CARTESIAN_POINT ( 'NONE',  ( -0.1210148435730253880, -0.5061394519557965710, 0.3122829191278980177 ) ) ;
#5768 = ORIENTED_EDGE ( 'NONE', *, *, #31035, .F. ) ;
#5767 = EDGE_LOOP ( 'NONE', ( #28652, #4612, #14707 ) ) ;
#5769 = EDGE_CURVE ( 'NONE', #23685, #26774, #36956, .T. ) ;
#5770 = CARTESIAN_POINT ( 'NONE',  ( 0.01161528454259690320, -0.8017023655927671966, -0.08667232896669077591 ) ) ;
#5771 = DIRECTION ( 'NONE',  ( 0.000000000000000000, 0.000000000000000000, 1.000000000000000000 ) ) ;
#5772 = CARTESIAN_POINT ( 'NONE',  ( -0.03642997641688847099, -0.5061875831641888812, 0.07642488348722685509 ) ) ;
#5773 = B_SPLINE_SURFACE_WITH_KNOTS ( 'NONE', 3, 3, ( 
 ( #24681, #37210, #12511, #5918 ),
 ( #18690, #31251, #3069, #15612 ),
 ( #9421, #31445, #22001, #18908 ),
 ( #15802, #38212, #19514, #10250 ),
 ( #31851, #32044, #22819, #6941 ),
 ( #3855, #10036, #16407, #25680 ),
 ( #31642, #13322, #812, #4263 ) ),
 .UNSPECIFIED., .F., .F., .F.,
 ( 4, 1, 1, 1, 4 ),
 ( 4, 4 ),
 ( 0.000000000000000000, 0.2500000000000000000, 0.5000000000000000000, 0.7500000000000000000, 1.000000000000000000 ),
 ( 0.000000000000000000, 1.000000000000000000 ),
 .UNSPECIFIED. ) ;
#5774 = CARTESIAN_POINT ( 'NONE',  ( 0.2397879752593336244, -0.9193312231006620650, 0.6873777895663281123 ) ) ;
#5775 = DIRECTION ( 'NONE',  ( 1.000000000000000000, 0.000000000000000000, 0.000000000000000000 ) ) ;
#5776 = CARTESIAN_POINT ( 'NONE',  ( 0.2563022272722030315, -1.568531830826473961, 0.8673523457354177513 ) ) ;
#5777 = CARTESIAN_POINT ( 'NONE',  ( 0.03505638526559837903, -0.6086893780663767961, 0.5882652742279115277 ) ) ;
#5778 = AXIS2_PLACEMENT_3D ( 'NONE', #30366, #29972, #8352 ) ;
#5779 = CARTESIAN_POINT ( 'NONE',  ( 0.4103533436992015671, -1.245885857446504374, 0.5182417262812503145 ) ) ;
#5780 = FACE_OUTER_BOUND ( 'NONE', #18681, .T. ) ;
#5781 = CARTESIAN_POINT ( 'NONE',  ( -0.0004160691872336406234, -0.9369703133356521718, 0.1337599650683027885 ) ) ;
#5782 = CARTESIAN_POINT ( 'NONE',  ( 0.2215734864168983353, -1.328907224007676913, 0.5182417262812423209 ) ) ;
#5783 =( NAMED_UNIT ( * ) PLANE_ANGLE_UNIT ( ) SI_UNIT ( $, .RADIAN. ) );
#5784 = DIRECTION ( 'NONE',  ( 1.000000000000000000, 0.000000000000000000, 0.000000000000000000 ) ) ;
#5785 = CARTESIAN_POINT ( 'NONE',  ( 0.2721752123224986386, -1.596339224327277595, 0.9197038883954219424 ) ) ;
#5786 = CARTESIAN_POINT ( 'NONE',  ( 0.06169161831772442678, -1.079659987968021762, 0.7429596578979000832 ) ) ;
#5787 = APPLICATION_PROTOCOL_DEFINITION ( 'international standard', 'automotive_design', 2000, #35544 ) ;
#5788 = CARTESIAN_POINT ( 'NONE',  ( 0.5517781715537678489, -1.195290833855036983, 0.8540039827052086086 ) ) ;
#5789 = DIRECTION ( 'NONE',  ( -8.881784197001246407E-16, 2.361472542561082612E-16, -1.000000000000000000 ) ) ;
#5790 = CARTESIAN_POINT ( 'NONE',  ( 0.04946426091936618336, 0.03515176265875070982, -0.4760065386269222709 ) ) ;
#5791 = CARTESIAN_POINT ( 'NONE',  ( 0.3888422987255840124, -1.656336475002445852, -0.4124152405210352867 ) ) ;
#5792 = ORIENTED_EDGE ( 'NONE', *, *, #11664, .F. ) ;
#5793 = DIRECTION ( 'NONE',  ( -7.000205099780314469E-17, -1.000000000000000000, 6.590151126658399604E-16 ) ) ;
#5794 = CARTESIAN_POINT ( 'NONE',  ( 0.2073178280655720573, -1.399379311278335480, 0.9347264154772038092 ) ) ;
#5795 = CARTESIAN_POINT ( 'NONE',  ( 0.5807400140824149348, -1.476489732972543489, 0.6842656776274327335 ) ) ;
#5797 = VERTEX_POINT ( 'NONE', #18649 ) ;
#5796 = CARTESIAN_POINT ( 'NONE',  ( -0.01548846960712831414, -0.5203207976466733831, 0.08861466064782504148 ) ) ;
#5798 = CARTESIAN_POINT ( 'NONE',  ( 0.1896483993057378192, -0.6911749089203499397, 0.2228938739458891649 ) ) ;
#5800 = ORIENTED_EDGE ( 'NONE', *, *, #29614, .T. ) ;
#5799 = ORIENTED_EDGE ( 'NONE', *, *, #15710, .F. ) ;
#5801 = CARTESIAN_POINT ( 'NONE',  ( 0.5439789624071748042, -1.183015531583673674, 0.8191768695127470412 ) ) ;
#5802 = DIRECTION ( 'NONE',  ( 1.417484439069006026E-31, -3.885780586188048878E-16, -1.000000000000000000 ) ) ;
#5803 = CARTESIAN_POINT ( 'NONE',  ( -0.1509132741912886377, 0.4664843738648666305, 0.09813923389061204872 ) ) ;
#5804 = COORDINATED_UNIVERSAL_TIME_OFFSET ( 0, 0, .AHEAD. ) ;
#5805 = DIRECTION ( 'NONE',  ( 0.000000000000000000, -1.000000000000000000, 3.330669073875470607E-16 ) ) ;
#5806 = ORIENTED_EDGE ( 'NONE', *, *, #27739, .T. ) ;
#5807 = CARTESIAN_POINT ( 'NONE',  ( 0.08692586860950433925, -0.7045980206078551467, 0.1576013572116870820 ) ) ;
#5808 = CARTESIAN_POINT ( 'NONE',  ( 0.2211959769661343000, -1.309495541150525799, -0.7462941026102624109 ) ) ;
#5809 = CARTESIAN_POINT ( 'NONE',  ( 0.5252982915109456474, -1.526881808260259987, 0.5746848141541492927 ) ) ;
#5811 = CARTESIAN_POINT ( 'NONE',  ( 9.210829332990911559E-05, -0.6768113429346261922, -0.02211036473533352364 ) ) ;
#5810 = CARTESIAN_POINT ( 'NONE',  ( 0.3252627854908551330, -1.766295133273483309, 0.5020845719335209623 ) ) ;
#5812 = CARTESIAN_POINT ( 'NONE',  ( -0.04293701532779557045, -0.3457382709204471771, 0.3536859687696398136 ) ) ;
#5813 = ORIENTED_EDGE ( 'NONE', *, *, #24369, .F. ) ;
#5814 = CARTESIAN_POINT ( 'NONE',  ( 0.2059273467974225835, -1.283046334493782359, -0.6184399470714002645 ) ) ;
#5815 = CARTESIAN_POINT ( 'NONE',  ( 0.5472056306734645048, -1.297393719792277134, 0.8953388641935672299 ) ) ;
#5816 = CARTESIAN_POINT ( 'NONE',  ( 0.01548846960707524721, 0.000000000000000000, 0.000000000000000000 ) ) ;
#5817 = CARTESIAN_POINT ( 'NONE',  ( 0.3675290616383497522, -2.037944530059963899, -0.5194381825500766769 ) ) ;
#5818 = CARTESIAN_POINT ( 'NONE',  ( 0.3704697912810961946, -1.166474544107111599, 0.4182417262808778013 ) ) ;
#5819 = CARTESIAN_POINT ( 'NONE',  ( -0.3000000000000000999, -2.068584980338025847, -0.2731141320652225590 ) ) ;
#5820 = CARTESIAN_POINT ( 'NONE',  ( 3.020486921392359971E-16, -1.318030225331671786E-16, 0.1999999999999994837 ) ) ;
#5821 = CARTESIAN_POINT ( 'NONE',  ( 0.2322244407957205770, -0.7584751632699872070, 0.4677412183550399005 ) ) ;
#5822 = PERSON_AND_ORGANIZATION_ROLE ( 'creator' ) ;
#5823 = CARTESIAN_POINT ( 'NONE',  ( 0.3597251525720394638, -1.934001777038073966, -0.5018490200258421963 ) ) ;
#5824 = CARTESIAN_POINT ( 'NONE',  ( 0.1977396076612820686, -2.033875238904685911, -0.6790160287402571271 ) ) ;
#5825 = FACE_OUTER_BOUND ( 'NONE', #39488, .T. ) ;
#5826 = CARTESIAN_POINT ( 'NONE',  ( -0.03174036153405352528, -0.07585545617081303205, 0.5190446117378583191 ) ) ;
#5827 = ORIENTED_EDGE ( 'NONE', *, *, #21997, .F. ) ;
#5828 = DIRECTION ( 'NONE',  ( 1.000000000000000000, 0.000000000000000000, 0.000000000000000000 ) ) ;
#5829 = DIRECTION ( 'NONE',  ( 0.8660512985181132439, 0.4999551463232376758, 0.000000000000000000 ) ) ;
#5830 = CARTESIAN_POINT ( 'NONE',  ( -0.2746410161513776482, -3.849534981189179028, -0.1910928155360645808 ) ) ;
#5831 = ORIENTED_EDGE ( 'NONE', *, *, #23024, .T. ) ;
#5832 = CARTESIAN_POINT ( 'NONE',  ( -0.03303708955568570443, 0.08827115631758945813, -0.5134073995267796064 ) ) ;
#5833 = ADVANCED_FACE ( 'NONE', ( #21738 ), #39196, .T. ) ;
#5834 = CARTESIAN_POINT ( 'NONE',  ( 0.09299045696175671505, -1.001796792555563087, 0.6985355088916623822 ) ) ;
#5836 = ORIENTED_EDGE ( 'NONE', *, *, #9802, .F. ) ;
#5835 = ORIENTED_EDGE ( 'NONE', *, *, #18262, .F. ) ;
#5837 = DIRECTION ( 'NONE',  ( 0.3468893892380643384, 0.7770416411310695493, 0.5252371270030109507 ) ) ;
#5838 = ORIENTED_EDGE ( 'NONE', *, *, #6733, .F. ) ;
#5839 = CARTESIAN_POINT ( 'NONE',  ( 0.02953079040094806068, -0.09152108205202535984, 0.5223162075576641694 ) ) ;
#5840 = CARTESIAN_POINT ( 'NONE',  ( 0.04575106512774684830, -0.4792499720836655430, -0.08732285767966210810 ) ) ;
#5841 = CARTESIAN_POINT ( 'NONE',  ( 0.2388826316829160967, -1.586798636953708153, -0.3224480331617204376 ) ) ;
#5842 = CARTESIAN_POINT ( 'NONE',  ( 0.000000000000000000, -0.3852620677835773555, -0.4748740771268961103 ) ) ;
#5844 = CARTESIAN_POINT ( 'NONE',  ( 0.4841487358689927634, -1.673745430023940717, 0.5182417262823179049 ) ) ;
#5843 = CARTESIAN_POINT ( 'NONE',  ( 0.01899468245560481314, 0.5123206680798495505, 0.08888613072388773517 ) ) ;
#5845 = CARTESIAN_POINT ( 'NONE',  ( -0.2399999999999999079, -2.323257895298838971, -0.7902071827178637209 ) ) ;
#5846 = VERTEX_POINT ( 'NONE', #18868 ) ;
#5847 = CARTESIAN_POINT ( 'NONE',  ( 0.2581756672896094451, -0.9092364711756537599, 0.7438128635199100502 ) ) ;
#5848 = ORIENTED_EDGE ( 'NONE', *, *, #20744, .T. ) ;
#5849 = CARTESIAN_POINT ( 'NONE',  ( 0.05634304521267756438, 0.01028123094841836525, 0.4588823192046724841 ) ) ;
#5850 = CARTESIAN_POINT ( 'NONE',  ( 0.4229029504711039888, -1.459654819224503353, 0.8188420036968601101 ) ) ;
#5851 = EDGE_CURVE ( 'NONE', #13497, #33249, #2440, .T. ) ;
#5853 = CARTESIAN_POINT ( 'NONE',  ( -0.09579104668929040722, -0.04310840302198015034, 0.09999999999999897859 ) ) ;
#5852 = CARTESIAN_POINT ( 'NONE',  ( 0.3357988224803010735, -1.647249694224340644, -0.6476600625557819013 ) ) ;
#5854 = CARTESIAN_POINT ( 'NONE',  ( 0.5611303468409032380, -1.505106176321531875, 0.5084158906598846839 ) ) ;
#5855 = CARTESIAN_POINT ( 'NONE',  ( 0.3700000000034951997, -2.073259481263499904, -0.6892711341747153053 ) ) ;
#5856 = APPLIED_DATE_AND_TIME_ASSIGNMENT ( #33364, #17724, ( #2357 ) ) ;
#5857 = PRODUCT_DEFINITION_CONTEXT ( 'detailed design', #15854, 'design' ) ;
#5858 = FACE_OUTER_BOUND ( 'NONE', #24697, .T. ) ;
#5859 = CARTESIAN_POINT ( 'NONE',  ( 0.3958825554100721122, -1.762582803447005464, -0.5282878467486828988 ) ) ;
#5860 = CARTESIAN_POINT ( 'NONE',  ( 0.1504400051554825868, -0.6766857922489548649, 0.4634885189021805685 ) ) ;
#5861 = CARTESIAN_POINT ( 'NONE',  ( 0.4400739460935926273, -1.687131003255787354, 0.4386290681939620240 ) ) ;
#5862 = PLANE ( 'NONE',  #31829 ) ;
#5863 =( BOUNDED_SURFACE ( )  B_SPLINE_SURFACE ( 3, 2, ( 
 ( #19500, #28748, #6718 ),
 ( #10022, #7116, #29145 ),
 ( #13523, #25469, #10235 ),
 ( #25881, #12914, #32029 ),
 ( #801, #3836, #9812 ),
 ( #26085, #38604, #4248 ),
 ( #34910, #25663, #25259 ),
 ( #19292, #16816, #29360 ),
 ( #37801, #10424, #28934 ),
 ( #3652, #13103, #9620 ),
 ( #22985, #16213, #22194 ),
 ( #38399, #15998, #31625 ),
 ( #22804, #28546, #420 ),
 ( #7312, #610, #38197 ),
 ( #35123, #35327, #19682 ),
 ( #32217, #4035, #13705 ),
 ( #17411, #39007, #8140 ),
 ( #32639, #20304, #23802 ),
 ( #4444, #5249, #17802 ),
 ( #30365, #20108, #1593 ),
 ( #8351, #36539, #39412 ),
 ( #26692, #26273, #38789 ),
 ( #7533, #11045, #17006 ),
 ( #10621, #5054, #23197 ),
 ( #29549, #1388, #29751 ),
 ( #20921, #35720, #13899 ),
 ( #11230, #39225, #7926 ),
 ( #33441, #26880, #26472 ),
 ( #23605, #17615, #36119 ),
 ( #10843, #4839, #33037 ),
 ( #23418, #29971, #35932 ),
 ( #7740, #32824, #4630 ),
 ( #17206, #14120, #1805 ),
 ( #20503, #14321, #36321 ) ),
 .UNSPECIFIED., .F., .F., .T. ) 
 B_SPLINE_SURFACE_WITH_KNOTS ( ( 4, 2, 2, 2, 2, 2, 2, 2, 2, 2, 2, 2, 2, 2, 2, 2, 4 ),
 ( 3, 3 ),
 ( 0.001710004797882772650, 0.002329098799114573057, 0.002948192800346373897, 0.003567286801578174304, 0.004186380802809974710, 0.004805474804041774683, 0.005424568805273575524, 0.006043662806505376364, 0.006662756807737176337, 0.007281850808968977178, 0.007900944810200778018, 0.008520038811432577991, 0.009139132812664377964, 0.009758226813896177937, 0.01037732081512797791, 0.01099641481635977788, 0.01161550881759157959 ),
 ( 0.000000000000000000, 1.000000000000000000 ),
 .UNSPECIFIED. ) 
 GEOMETRIC_REPRESENTATION_ITEM ( )  RATIONAL_B_SPLINE_SURFACE ( (
 ( 1.000000000000000000, 0.7661775686432606980, 1.000000000000000000),
 ( 1.000000000000000000, 0.7660633144985160570, 1.000000000000000000),
 ( 1.000000000000000000, 0.7659625556653616441, 1.000000000000000000),
 ( 1.000000000000000000, 0.7657843064335759786, 1.000000000000000000),
 ( 1.000000000000000000, 0.7657059323776339577, 1.000000000000000000),
 ( 1.000000000000000000, 0.7655651667306325736, 1.000000000000000000),
 ( 1.000000000000000000, 0.7655031821185447338, 1.000000000000000000),
 ( 1.000000000000000000, 0.7654067721134163449, 1.000000000000000000),
 ( 1.000000000000000000, 0.7653717631867683613, 1.000000000000000000),
 ( 1.000000000000000000, 0.7653379689688158960, 1.000000000000000000),
 ( 1.000000000000000000, 0.7653399838946506328, 1.000000000000000000),
 ( 1.000000000000000000, 0.7653826612811753805, 1.000000000000000000),
 ( 1.000000000000000000, 0.7654239822339510280, 1.000000000000000000),
 ( 1.000000000000000000, 0.7655382443605589504, 1.000000000000000000),
 ( 1.000000000000000000, 0.7656103788928951825, 1.000000000000000000),
 ( 1.000000000000000000, 0.7657736866170623546, 1.000000000000000000),
 ( 1.000000000000000000, 0.7658654630984720324, 1.000000000000000000),
 ( 1.000000000000000000, 0.7660476170358867520, 1.000000000000000000),
 ( 1.000000000000000000, 0.7661388857263637941, 1.000000000000000000),
 ( 1.000000000000000000, 0.7663086609638074531, 1.000000000000000000),
 ( 1.000000000000000000, 0.7663852831037184510, 1.000000000000000000),
 ( 1.000000000000000000, 0.7665082163394573156, 1.000000000000000000),
 ( 1.000000000000000000, 0.7665553051685600749, 1.000000000000000000),
 ( 1.000000000000000000, 0.7666099424742220947, 1.000000000000000000),
 ( 1.000000000000000000, 0.7666174550739168758, 1.000000000000000000),
 ( 1.000000000000000000, 0.7665941758084844349, 1.000000000000000000),
 ( 1.000000000000000000, 0.7665628199831622247, 1.000000000000000000),
 ( 1.000000000000000000, 0.7664711555354097872, 1.000000000000000000),
 ( 1.000000000000000000, 0.7664113945286483709, 1.000000000000000000),
 ( 1.000000000000000000, 0.7662685914096645234, 1.000000000000000000),
 ( 1.000000000000000000, 0.7661862752594525983, 1.000000000000000000),
 ( 1.000000000000000000, 0.7659979125830966851, 1.000000000000000000),
 ( 1.000000000000000000, 0.7658906909088671888, 1.000000000000000000),
 ( 1.000000000000000000, 0.7657622705003380714, 1.000000000000000000) ) ) 
 REPRESENTATION_ITEM ( '' )  SURFACE ( )  );
#5864 = CARTESIAN_POINT ( 'NONE',  ( -0.04155248107635943489, 0.4523094957185410658, 0.1288470070525102595 ) ) ;
#5865 = DIRECTION ( 'NONE',  ( 1.000000000000000000, -0.000000000000000000, -0.000000000000000000 ) ) ;
#5866 = CARTESIAN_POINT ( 'NONE',  ( 0.01548846960721238578, 0.07651041855108486889, -0.5222379212565272377 ) ) ;
#5867 = CARTESIAN_POINT ( 'NONE',  ( 0.2334441654029815461, -1.232220874905952002, 0.5357669168543389704 ) ) ;
#5868 = CARTESIAN_POINT ( 'NONE',  ( 0.3136609249452982917, -0.7980415872784507592, 0.6920156437578004471 ) ) ;
#5869 = ADVANCED_FACE ( 'NONE', ( #40458 ), #37171, .T. ) ;
#5870 = CARTESIAN_POINT ( 'NONE',  ( -0.03674260963082939813, 0.3145436874713448683, 0.3636070162938564443 ) ) ;
#5871 = CARTESIAN_POINT ( 'NONE',  ( 0.0007958614940114835511, -0.9534529561155069555, 0.2845628645576042670 ) ) ;
#5872 = CARTESIAN_POINT ( 'NONE',  ( 0.6481235002692135039, -1.442380924828635447, -0.4125509721431598886 ) ) ;
#5873 = CARTESIAN_POINT ( 'NONE',  ( 0.1173046356037009130, -1.376169800289570366, -0.7015791660361966331 ) ) ;
#5874 = EDGE_CURVE ( 'NONE', #2060, #25189, #23481, .T. ) ;
#5875 = CARTESIAN_POINT ( 'NONE',  ( 0.08509462337972420465, -0.8106601073620037790, 0.1457185332388698795 ) ) ;
#5876 = CARTESIAN_POINT ( 'NONE',  ( 0.06954796871655651025, -1.315582234632707515, 0.5182417262812430980 ) ) ;
#5877 = CARTESIAN_POINT ( 'NONE',  ( 0.5972649584706940518, -1.597985788488442527, 0.4298582196018018720 ) ) ;
#5878 = ADVANCED_FACE ( 'NONE', ( #3210 ), #22725, .F. ) ;
#5879 = ORIENTED_EDGE ( 'NONE', *, *, #21242, .T. ) ;
#5880 = DIRECTION ( 'NONE',  ( -1.000000000000000000, -6.779273404243070203E-32, -4.314083075427408311E-32 ) ) ;
#5881 = CARTESIAN_POINT ( 'NONE',  ( 0.3855795899639143376, -1.693646422290408848, -0.6199096498204479389 ) ) ;
#5882 = EDGE_CURVE ( 'NONE', #38697, #4624, #37906, .T. ) ;
#5883 = CARTESIAN_POINT ( 'NONE',  ( 0.6636547731126125615, -1.509847865698558556, 0.4182417262808776903 ) ) ;
#5884 = EDGE_CURVE ( 'NONE', #33803, #10331, #30138, .T. ) ;
#5885 = CARTESIAN_POINT ( 'NONE',  ( 0.4081716264380484960, -1.688076292791303334, -0.6123051696410528599 ) ) ;
#5886 = EDGE_CURVE ( 'NONE', #24301, #30304, #11627, .T. ) ;
#5887 = ADVANCED_BREP_SHAPE_REPRESENTATION ( '', ( #32046, #27819 ), #33063 ) ;
#5888 = VERTEX_POINT ( 'NONE', #4810 ) ;
#5889 = FACE_OUTER_BOUND ( 'NONE', #13516, .T. ) ;
#5890 = CARTESIAN_POINT ( 'NONE',  ( 0.3332069212083951792, -1.175771073360517116, 0.5719569841860573378 ) ) ;
#5891 = CYLINDRICAL_SURFACE ( 'NONE', #28970, 0.1620173459747806799 ) ;
#5892 = CARTESIAN_POINT ( 'NONE',  ( 0.04230170315644368045, 0.2824006788359467723, -0.3740536075335736399 ) ) ;
#5893 = CARTESIAN_POINT ( 'NONE',  ( 0.4874005273354089507, -1.272337409915087258, 0.6815837265936333100 ) ) ;
#5895 = CARTESIAN_POINT ( 'NONE',  ( 0.5435933681566625930, -1.596171129003035150, -0.5612309872450876869 ) ) ;
#5894 = CARTESIAN_POINT ( 'NONE',  ( -0.3000000000000000999, -3.156018320128275878, -0.4841849112664152743 ) ) ;
#5896 = CARTESIAN_POINT ( 'NONE',  ( 0.5133443775832216005, -1.117606250044787863, 0.5819851345710455037 ) ) ;
#5897 = ORIENTED_EDGE ( 'NONE', *, *, #27113, .T. ) ;
#5898 = SECURITY_CLASSIFICATION_LEVEL ( 'unclassified' ) ;
#5899 = DIRECTION ( 'NONE',  ( 7.967889981520751253E-15, 0.9901182710308658041, 0.1402348365095101024 ) ) ;
#5900 = EDGE_LOOP ( 'NONE', ( #22797, #7537, #23343, #6978 ) ) ;
#5901 = ORIENTED_EDGE ( 'NONE', *, *, #27040, .T. ) ;
#5902 = CARTESIAN_POINT ( 'NONE',  ( 0.2499116230160881025, -1.320538391621939533, 0.9121915517445829957 ) ) ;
#5903 = EDGE_CURVE ( 'NONE', #1786, #27128, #5638, .T. ) ;
#5905 = CARTESIAN_POINT ( 'NONE',  ( 0.1138168093370103690, -0.5794347803528829832, -0.06987067695535194300 ) ) ;
#5904 = CARTESIAN_POINT ( 'NONE',  ( 0.4137599315576335757, -1.590143257116447995, -0.4137273532990812797 ) ) ;
#5906 = DIRECTION ( 'NONE',  ( -6.162975822039151309E-33, 0.000000000000000000, -1.000000000000000000 ) ) ;
#5907 = APPLIED_DATE_AND_TIME_ASSIGNMENT ( #30836, #12122, ( #20515 ) ) ;
#5908 = CIRCLE ( 'NONE', #7896, 0.2200000000000000844 ) ;
#5909 = VERTEX_POINT ( 'NONE', #8518 ) ;
#5910 = ORIENTED_EDGE ( 'NONE', *, *, #17691, .T. ) ;
#5911 = CARTESIAN_POINT ( 'NONE',  ( 0.3349705278058782709, -1.064816160538507139, 0.6377121673170756955 ) ) ;
#5912 = CARTESIAN_POINT ( 'NONE',  ( 0.4769129862565332223, -1.388126235601429892, 0.8131988394239295648 ) ) ;
#5913 = VERTEX_POINT ( 'NONE', #33609 ) ;
#5914 = DIRECTION ( 'NONE',  ( 1.000000000000000000, 2.280301054154495132E-31, -1.664003471950577689E-31 ) ) ;
#5915 = DIRECTION ( 'NONE',  ( 0.8660512985181132439, 0.4999551463232376758, 0.000000000000000000 ) ) ;
#5916 = CIRCLE ( 'NONE', #30891, 0.08000000000000000167 ) ;
#5917 = CARTESIAN_POINT ( 'NONE',  ( 0.5827850094984949880, -1.549234897118938248, -0.4241087081391718971 ) ) ;
#5918 = CARTESIAN_POINT ( 'NONE',  ( 0.3999999999999787059, -2.097675824466503691, -0.2588528740066097233 ) ) ;
#5919 = CARTESIAN_POINT ( 'NONE',  ( 0.3740960844805631957, -1.108072201694596526, 0.5182417262812423209 ) ) ;
#5920 = CARTESIAN_POINT ( 'NONE',  ( 0.3056347003372518745, -1.768333716703696323, 0.5707417262808793801 ) ) ;
#5921 = CARTESIAN_POINT ( 'NONE',  ( 0.09106859344845208426, -1.304999351207305480, 0.5974602131358454082 ) ) ;
#5922 = CARTESIAN_POINT ( 'NONE',  ( 0.04579397197547097759, -1.450962534347209898, -0.6396520520129289622 ) ) ;
#5923 = CARTESIAN_POINT ( 'NONE',  ( 0.08042334443895514384, -1.362032735465325661, 0.6028738014108521170 ) ) ;
#5924 = APPROVAL_ROLE ( '' ) ;
#5925 = CARTESIAN_POINT ( 'NONE',  ( 0.3459602365858145401, -1.002069219538038736, 0.6041729112776661470 ) ) ;
#5926 = CARTESIAN_POINT ( 'NONE',  ( 0.4826234098002670780, -1.120895762997321077, 0.5150456658529999343 ) ) ;
#5927 = CARTESIAN_POINT ( 'NONE',  ( 0.4568206499005321164, -1.218986888361895282, 0.5856983068965044836 ) ) ;
#5928 = CARTESIAN_POINT ( 'NONE',  ( 0.03113248654051816583, 0.5878163732725504298, -0.2204268771689479045 ) ) ;
#5929 = EDGE_CURVE ( 'NONE', #1752, #17150, #14234, .T. ) ;
#5930 = CARTESIAN_POINT ( 'NONE',  ( 0.1172025164431036715, -1.392648223243311723, 0.6963985612953286219 ) ) ;
#5931 = DIRECTION ( 'NONE',  ( -1.000000000000000000, -0.000000000000000000, -0.000000000000000000 ) ) ;
#5932 = ADVANCED_FACE ( 'NONE', ( #24183 ), #11414, .F. ) ;
#5933 = FACE_OUTER_BOUND ( 'NONE', #250, .T. ) ;
#5934 = AXIS2_PLACEMENT_3D ( 'NONE', #28475, #9754, #350 ) ;
#5935 = CARTESIAN_POINT ( 'NONE',  ( 0.3177856290042974652, -1.645584934368151009, 0.5182417262812344383 ) ) ;
#5936 = EDGE_CURVE ( 'NONE', #31618, #34948, #25440, .T. ) ;
#5937 = VERTEX_POINT ( 'NONE', #33835 ) ;
#5938 = ORIENTED_EDGE ( 'NONE', *, *, #6468, .F. ) ;
#5939 = CIRCLE ( 'NONE', #2007, 0.01500000000000001679 ) ;
#5940 = CARTESIAN_POINT ( 'NONE',  ( -0.01548846960688982435, -0.5198120922917083275, 0.07362328916747526431 ) ) ;
#5941 = VERTEX_POINT ( 'NONE', #17385 ) ;
#5942 = EDGE_CURVE ( 'NONE', #38229, #15275, #22809, .T. ) ;
#5943 = DIRECTION ( 'NONE',  ( 0.000000000000000000, -1.047646519776162108E-15, -1.000000000000000000 ) ) ;
#5944 = DIRECTION ( 'NONE',  ( 1.000000000000000000, -0.000000000000000000, -0.000000000000000000 ) ) ;
#5945 = AXIS2_PLACEMENT_3D ( 'NONE', #12052, #3002, #40014 ) ;
#5946 = LINE ( 'NONE', #24489, #26374 ) ;
#5948 = EDGE_LOOP ( 'NONE', ( #12791, #23837, #5456, #302 ) ) ;
#5947 = DIRECTION ( 'NONE',  ( 4.930380657631319405E-32, -0.5237184928541299689, 0.8518913899333638851 ) ) ;
#5949 = ORIENTED_EDGE ( 'NONE', *, *, #8061, .T. ) ;
#5950 = EDGE_LOOP ( 'NONE', ( #21037, #37396, #15447, #21709 ) ) ;
#5951 = CARTESIAN_POINT ( 'NONE',  ( 0.03868264068766662234, 0.4417248602032609606, -0.1788646266443645882 ) ) ;
#5952 = ORIENTED_EDGE ( 'NONE', *, *, #28522, .T. ) ;
#5953 = ADVANCED_FACE ( 'NONE', ( #29944 ), #15565, .T. ) ;
#5954 = CARTESIAN_POINT ( 'NONE',  ( -0.001446413187643280814, -0.5403182641434959299, 0.2206895948476451930 ) ) ;
#5956 = CARTESIAN_POINT ( 'NONE',  ( 0.4264202721361137760, -1.467519734074644200, -0.5166151207188711680 ) ) ;
#5955 = CARTESIAN_POINT ( 'NONE',  ( 0.4190035292061285999, -1.208494183746581463, 0.6641413202029121665 ) ) ;
#5957 = DIRECTION ( 'NONE',  ( 0.000000000000000000, 5.978086547377980964E-31, 1.000000000000000000 ) ) ;
#5958 = EDGE_CURVE ( 'NONE', #12799, #51, #14297, .T. ) ;
#5959 = CARTESIAN_POINT ( 'NONE',  ( -0.1129900121204312630, -0.5167580615070168637, 0.3146079272632524848 ) ) ;
#5961 = ORIENTED_EDGE ( 'NONE', *, *, #514, .F. ) ;
#5960 = EDGE_LOOP ( 'NONE', ( #33297, #39298 ) ) ;
#5962 = ADVANCED_FACE ( 'NONE', ( #11020 ), #11207, .T. ) ;
#5963 = CARTESIAN_POINT ( 'NONE',  ( 0.3861171055049215095, -1.790989158299715500, -0.4824067298016651573 ) ) ;
#5964 = DIRECTION ( 'NONE',  ( 1.000000000000000000, 6.779273404243070203E-32, 4.314083075427408311E-32 ) ) ;
#5965 = CARTESIAN_POINT ( 'NONE',  ( -0.03303708955568582240, -0.5155567402493581586, 0.07470075307485188332 ) ) ;
#5966 = CARTESIAN_POINT ( 'NONE',  ( 0.5132325995285942355, -1.352621407328026493, 0.8007139552203286215 ) ) ;
#5967 = CARTESIAN_POINT ( 'NONE',  ( 0.2230041220662333790, -0.9268358352298275982, 0.6424936301217993861 ) ) ;
#5968 = CARTESIAN_POINT ( 'NONE',  ( 0.5271998568954198161, -1.674914755896795837, -0.4628290575504125925 ) ) ;
#5969 = AXIS2_PLACEMENT_3D ( 'NONE', #33083, #32683, #4488 ) ;
#5970 = CARTESIAN_POINT ( 'NONE',  ( 0.3192871411569696005, -1.699607763058582632, 0.8452318849098621190 ) ) ;
#5971 = B_SPLINE_CURVE_WITH_KNOTS ( 'NONE', 3,
 ( #14695, #7495, #20075, #31359 ),
 .UNSPECIFIED., .F., .F.,
 ( 4, 4 ),
 ( 0.000000000000000000, 0.004353774562966205262 ),
 .UNSPECIFIED. ) ;
#5972 = DIRECTION ( 'NONE',  ( 0.000000000000000000, 0.000000000000000000, -1.000000000000000000 ) ) ;
#5973 = CARTESIAN_POINT ( 'NONE',  ( 0.5708401535611469235, -1.615683077095924736, 0.5197417262808792238 ) ) ;
#5974 = CARTESIAN_POINT ( 'NONE',  ( 0.3409152363046951129, -1.516880185093671063, -0.7462941026102624109 ) ) ;
#5975 = CARTESIAN_POINT ( 'NONE',  ( 0.3969982963057278047, -1.750077671058422046, -0.4821875037442182599 ) ) ;
#5976 = CIRCLE ( 'NONE', #28973, 0.01499999999999995261 ) ;
#5977 = VECTOR ( 'NONE', #24941, 39.37007874015748143 ) ;
#5978 = CARTESIAN_POINT ( 'NONE',  ( -6.552157794917040043E-17, -0.4262518876079541830, 0.1106581735831166785 ) ) ;
#5979 = CARTESIAN_POINT ( 'NONE',  ( 0.09137806685966429199, -1.251329420820371352, 0.7514797811827245155 ) ) ;
#5980 = SECURITY_CLASSIFICATION_LEVEL ( 'unclassified' ) ;
#5981 = CARTESIAN_POINT ( 'NONE',  ( 0.6116693357450743163, -1.291191393066782211, 0.8405059385265429839 ) ) ;
#5982 = EDGE_CURVE ( 'NONE', #20771, #4299, #39386, .T. ) ;
#5983 = CARTESIAN_POINT ( 'NONE',  ( -0.2399999999999999079, -3.719155698466370286, -0.2948051799630662106 ) ) ;
#5984 = CIRCLE ( 'NONE', #13879, 0.06250000000000001388 ) ;
#5985 = CARTESIAN_POINT ( 'NONE',  ( 0.1399999999999994582, -1.330566893520353813E-17, -0.05000000000000000971 ) ) ;
#5986 = ADVANCED_FACE ( 'NONE', ( #30935 ), #18385, .F. ) ;
#5987 = CARTESIAN_POINT ( 'NONE',  ( 0.03309060444528739986, -0.2303206394829937220, 0.4671006372792966821 ) ) ;
#5988 = CARTESIAN_POINT ( 'NONE',  ( 0.3700641620961017120, -1.680321446636507954, -0.4309109543678180665 ) ) ;
#5989 = ORIENTED_EDGE ( 'NONE', *, *, #11507, .F. ) ;
#5990 = CARTESIAN_POINT ( 'NONE',  ( -0.08000000000000000167, -1.706654027108509997, -0.06438491259384497567 ) ) ;
#5991 = CARTESIAN_POINT ( 'NONE',  ( 0.2706767884852234185, -1.629893486181000384, 0.7916626055961630826 ) ) ;
#5992 = AXIS2_PLACEMENT_3D ( 'NONE', #28995, #13367, #6988 ) ;
#5994 = ORIENTED_EDGE ( 'NONE', *, *, #33815, .T. ) ;
#5993 = CARTESIAN_POINT ( 'NONE',  ( 0.1286531880915039450, -0.5504795770112219655, 0.1457185332388692689 ) ) ;
#5996 = ORIENTED_EDGE ( 'NONE', *, *, #14908, .T. ) ;
#5995 = DIRECTION ( 'NONE',  ( 1.000000000000000000, 6.779273404243070203E-32, 4.314083075427408311E-32 ) ) ;
#5997 = CARTESIAN_POINT ( 'NONE',  ( 0.3677026761718887315, -0.9383931188863808837, 0.6934371584156296953 ) ) ;
#5999 = ORIENTED_EDGE ( 'NONE', *, *, #39380, .F. ) ;
#5998 = ORIENTED_EDGE ( 'NONE', *, *, #14680, .T. ) ;
#6000 = CARTESIAN_POINT ( 'NONE',  ( 0.2186022828414512231, -0.6499659907669792513, 0.4387193036502484711 ) ) ;
#6001 = CARTESIAN_POINT ( 'NONE',  ( -0.3000000000000000999, -3.941790907013290823, -0.4709369376873030477 ) ) ;
#6002 = DIRECTION ( 'NONE',  ( -1.000000000000000000, -2.280301054154495132E-31, 1.664003471950577689E-31 ) ) ;
#6003 = COORDINATED_UNIVERSAL_TIME_OFFSET ( 0, 0, .AHEAD. ) ;
#6004 = CIRCLE ( 'NONE', #3402, 0.9237847906030128842 ) ;
#6005 = DIRECTION ( 'NONE',  ( 1.000000000000000000, 0.000000000000000000, 0.000000000000000000 ) ) ;
#6006 = EDGE_LOOP ( 'NONE', ( #7813, #31891, #14351 ) ) ;
#6007 = ADVANCED_FACE ( 'NONE', ( #31360 ), #20537, .T. ) ;
#6008 = CARTESIAN_POINT ( 'NONE',  ( 0.09634828771505739298, -0.7600076796586502370, 0.3121834059226053504 ) ) ;
#6009 = CARTESIAN_POINT ( 'NONE',  ( 0.2059273467974225835, -1.283046334493782359, -0.2869361388274796476 ) ) ;
#6010 = CARTESIAN_POINT ( 'NONE',  ( 0.5252677807972566670, -1.526876841991572142, 0.5741887749453796763 ) ) ;
#6012 = CARTESIAN_POINT ( 'NONE',  ( 0.0001905119757726109924, -0.6656977259803509295, -0.02102838956235005691 ) ) ;
#6011 = CARTESIAN_POINT ( 'NONE',  ( 0.3499317094845418308, -1.754137739073130753, 0.4513909310129528007 ) ) ;
#6013 = CARTESIAN_POINT ( 'NONE',  ( -0.05634301242525816683, -0.2614060064472246703, 0.3772872482281147688 ) ) ;
#6014 = ORIENTED_EDGE ( 'NONE', *, *, #4618, .F. ) ;
#6015 = CARTESIAN_POINT ( 'NONE',  ( 0.4327791790642120384, -1.706049035981101358, 0.6054719847766963925 ) ) ;
#6016 = B_SPLINE_CURVE_WITH_KNOTS ( 'NONE', 3,
 ( #39087, #7604, #29619, #13976 ),
 .UNSPECIFIED., .F., .F.,
 ( 4, 4 ),
 ( 8.673617379884035472E-19, 0.0008438904120417860255 ),
 .UNSPECIFIED. ) ;
#6017 = CARTESIAN_POINT ( 'NONE',  ( 0.2866465215685243817, -0.7220565828703142675, 0.6519108322339883799 ) ) ;
#6018 = CARTESIAN_POINT ( 'NONE',  ( 0.5014513378216763906, -1.607116428610278369, -0.6294611457982872693 ) ) ;
#6019 = CARTESIAN_POINT ( 'NONE',  ( 0.006030796843114796454, -0.8457574864219309374, 0.1381917444211341606 ) ) ;
#6020 = FACE_OUTER_BOUND ( 'NONE', #25602, .T. ) ;
#6021 = CIRCLE ( 'NONE', #32282, 0.2000000000000000111 ) ;
#6022 = CARTESIAN_POINT ( 'NONE',  ( 0.000000000000000000, 0.000000000000000000, 0.000000000000000000 ) ) ;
#6023 = CARTESIAN_POINT ( 'NONE',  ( -2.112273405726188513E-14, -2.097675824466503691, -0.6968637352380161465 ) ) ;
#6024 = CARTESIAN_POINT ( 'NONE',  ( 0.1614670899430008522, -0.7569536277469717245, 0.1022936816274460647 ) ) ;
#6025 = CARTESIAN_POINT ( 'NONE',  ( 0.5342447626335863342, -1.156090923338821463, 0.6541422520001994867 ) ) ;
#6026 = COORDINATED_UNIVERSAL_TIME_OFFSET ( 0, 0, .AHEAD. ) ;
#6027 = AXIS2_PLACEMENT_3D ( 'NONE', #24820, #9154, #34251 ) ;
#6028 = AXIS2_PLACEMENT_3D ( 'NONE', #14289, #35690, #30132 ) ;
#6029 = CARTESIAN_POINT ( 'NONE',  ( 0.6477906992409429021, -1.570672284941449615, 0.6203763125787145061 ) ) ;
#6031 = B_SPLINE_CURVE_WITH_KNOTS ( 'NONE', 3,
 ( #36355, #7769, #32857, #20534, #29786, #23834, #32668, #11477, #26301, #8377 ),
 .UNSPECIFIED., .F., .F.,
 ( 4, 3, 3, 4 ),
 ( -6.000000000173966796E-08, 0.000000000000000000, 1.599765854542544604E-05, 3.053234943348237166E-05 ),
 .UNSPECIFIED. ) ;
#6030 = AXIS2_PLACEMENT_3D ( 'NONE', #40417, #9134, #21700 ) ;
#6032 = CARTESIAN_POINT ( 'NONE',  ( 0.3572717916512525571, -1.888853545459783234, -0.6650645762259550509 ) ) ;
#6033 = CARTESIAN_POINT ( 'NONE',  ( 0.3986508974220148160, -1.711168768618083869, 0.4182305167228609899 ) ) ;
#6034 = CARTESIAN_POINT ( 'NONE',  ( -0.03674260963082456866, -0.3145436874713427589, -0.3636070162938578876 ) ) ;
#6035 = ORIENTED_EDGE ( 'NONE', *, *, #277, .T. ) ;
#6036 = CARTESIAN_POINT ( 'NONE',  ( 0.4730613458671842353, -1.134798785001164712, 0.4646432420420624210 ) ) ;
#6037 = CARTESIAN_POINT ( 'NONE',  ( -0.03301200226531778026, -0.2303790867044788193, 0.4673050311136081603 ) ) ;
#6038 = FACE_OUTER_BOUND ( 'NONE', #341, .T. ) ;
#6039 = ORIENTED_EDGE ( 'NONE', *, *, #12042, .F. ) ;
#6040 = CARTESIAN_POINT ( 'NONE',  ( -0.04047076529493147390, 0.06272252650431850429, -0.4973259435627279679 ) ) ;
#6041 = CARTESIAN_POINT ( 'NONE',  ( 0.07383395682904796142, -1.276537601224291274, 0.7475687110354797271 ) ) ;
#6043 = ORIENTED_EDGE ( 'NONE', *, *, #25118, .T. ) ;
#6042 = ORIENTED_EDGE ( 'NONE', *, *, #10399, .T. ) ;
#6044 = CARTESIAN_POINT ( 'NONE',  ( -0.08408070219615630669, -0.09959325338431362917, 0.08499999999999756362 ) ) ;
#6045 = EDGE_LOOP ( 'NONE', ( #4719, #20454, #37933, #9548 ) ) ;
#6046 = CARTESIAN_POINT ( 'NONE',  ( 0.5096379620664639454, -1.685052907890733698, -0.5155029497116575543 ) ) ;
#6047 = CARTESIAN_POINT ( 'NONE',  ( 0.03674078017396070067, -0.4430116966224423858, -0.1867947199041681827 ) ) ;
#6048 = CARTESIAN_POINT ( 'NONE',  ( 0.1825719458642482418, -1.864899009783420158, -0.3443257192141048750 ) ) ;
#6049 = FACE_OUTER_BOUND ( 'NONE', #19861, .T. ) ;
#6051 = LINE ( 'NONE', #28093, #12213 ) ;
#6050 = CARTESIAN_POINT ( 'NONE',  ( -0.1202595235781067778, 0.06028806207340019208, 0.04170439506869236951 ) ) ;
#6052 = CARTESIAN_POINT ( 'NONE',  ( 0.05561310505367052931, -0.2541457526436871062, -0.3845267872006568055 ) ) ;
#6053 = ORIENTED_EDGE ( 'NONE', *, *, #33366, .F. ) ;
#6054 = CARTESIAN_POINT ( 'NONE',  ( 0.07795955261373284373, -1.322072399571159407, 0.5462526511609022695 ) ) ;
#6055 = ORIENTED_EDGE ( 'NONE', *, *, #28191, .F. ) ;
#6056 = VECTOR ( 'NONE', #17111, 39.37007874015748143 ) ;
#6057 = DIRECTION ( 'NONE',  ( 1.000000000000000000, -0.000000000000000000, -0.000000000000000000 ) ) ;
#6058 = AXIS2_PLACEMENT_3D ( 'NONE', #10702, #32900, #29227 ) ;
#6059 = CARTESIAN_POINT ( 'NONE',  ( 0.4708967593789014638, -1.552455728631323417, 0.6553166368004886833 ) ) ;
#6061 = CARTESIAN_POINT ( 'NONE',  ( 0.5678328055818865350, -1.616694484607086313, 0.5530647866453864969 ) ) ;
#6060 = CARTESIAN_POINT ( 'NONE',  ( -0.05634307799789353005, -0.4395998308137162858, 0.1320249839696058525 ) ) ;
#6062 = CARTESIAN_POINT ( 'NONE',  ( 0.02953079040095728247, 0.000000000000000000, 0.000000000000000000 ) ) ;
#6063 = CARTESIAN_POINT ( 'NONE',  ( -0.01548846960707490547, 0.5346638663566671834, 0.07572681171513505338 ) ) ;
#6064 = AXIS2_PLACEMENT_3D ( 'NONE', #18114, #37241, #33958 ) ;
#6065 = EDGE_CURVE ( 'NONE', #6967, #30939, #12616, .T. ) ;
#6066 = CARTESIAN_POINT ( 'NONE',  ( -0.05464101615137770263, -2.542046649843399564, -0.2305290188067205259 ) ) ;
#6067 = CARTESIAN_POINT ( 'NONE',  ( 0.1866634323211664725, -1.707720045599271819, -0.3287304398696229146 ) ) ;
#6068 = CARTESIAN_POINT ( 'NONE',  ( 0.5817289510859825485, -1.495063960572125872, 0.5924595019112512961 ) ) ;
#6069 = CARTESIAN_POINT ( 'NONE',  ( 0.4792821459481910740, -1.664810697191674960, 0.5161465343054540966 ) ) ;
#6070 = CYLINDRICAL_SURFACE ( 'NONE', #8175, 0.2500000000000000000 ) ;
#6071 = CARTESIAN_POINT ( 'NONE',  ( 0.2183697179345998052, -1.229346570154329799, 0.5436728950768712210 ) ) ;
#6072 = CARTESIAN_POINT ( 'NONE',  ( 0.2225889308918536924, -1.238345268919997855, 0.5682417262808776570 ) ) ;
#6073 = CARTESIAN_POINT ( 'NONE',  ( 0.3585389588907697545, -1.160913934521024649, 0.4273619767025411131 ) ) ;
#6074 = CARTESIAN_POINT ( 'NONE',  ( 0.2232487200984690223, -0.6189500806901601093, 0.4773341886849224447 ) ) ;
#6075 = CARTESIAN_POINT ( 'NONE',  ( -0.05137569054208737662, 0.2590973494995081339, 0.3946951280584610200 ) ) ;
#6076 = CARTESIAN_POINT ( 'NONE',  ( 0.06844863008403212490, -1.325512397932680608, 0.5829276846574326099 ) ) ;
#6077 = CIRCLE ( 'NONE', #23854, 0.01499999999999998730 ) ;
#6078 = CARTESIAN_POINT ( 'NONE',  ( 0.6505092258671375527, -1.603730573490085964, -0.4546931408925402041 ) ) ;
#6079 = CARTESIAN_POINT ( 'NONE',  ( 0.3979572690256317213, -2.042933421733604149, -0.4802053186314065858 ) ) ;
#6080 = CARTESIAN_POINT ( 'NONE',  ( 0.1070150395144117139, -0.8615151753913300459, 0.4568215877972369166 ) ) ;
#6081 = DIRECTION ( 'NONE',  ( 0.000000000000000000, 0.000000000000000000, -1.000000000000000000 ) ) ;
#6082 = LINE ( 'NONE', #30990, #253 ) ;
#6083 = CIRCLE ( 'NONE', #6737, 0.01500000000000001159 ) ;
#6084 = ORIENTED_EDGE ( 'NONE', *, *, #9391, .F. ) ;
#6085 = CARTESIAN_POINT ( 'NONE',  ( -0.1969433606228568612, 0.5138636982738121750, 0.3749999999999991673 ) ) ;
#6086 = CARTESIAN_POINT ( 'NONE',  ( 0.000000000000000000, -0.2793841226333812489, -0.1799682156082512696 ) ) ;
#6087 = AXIS2_PLACEMENT_3D ( 'NONE', #4578, #21056, #17151 ) ;
#6088 = CARTESIAN_POINT ( 'NONE',  ( 0.6499217190830813839, -1.534003153280716569, 0.4182417262808776903 ) ) ;
#6089 = CARTESIAN_POINT ( 'NONE',  ( 0.5490567416132084988, -1.662297187303882984, -0.4838776693470574486 ) ) ;
#6090 = DIRECTION ( 'NONE',  ( -0.4999551463232372317, 0.8660512985181135770, -0.000000000000000000 ) ) ;
#6091 = VERTEX_POINT ( 'NONE', #25179 ) ;
#6092 = CARTESIAN_POINT ( 'NONE',  ( -0.2746410161513776482, -3.941790907013290823, -0.4709369376873030477 ) ) ;
#6093 = CIRCLE ( 'NONE', #15307, 0.01000000000000001582 ) ;
#6094 = CARTESIAN_POINT ( 'NONE',  ( 0.3528210451890865795, -1.143700418102651994, 0.6155400910483455057 ) ) ;
#6095 = CARTESIAN_POINT ( 'NONE',  ( 0.3499317094845083576, -1.754137739073151847, 0.4513909310129906038 ) ) ;
#6096 = DIRECTION ( 'NONE',  ( 0.8660512985181135770, 0.4999551463232370097, 0.000000000000000000 ) ) ;
#6097 = CARTESIAN_POINT ( 'NONE',  ( 0.4076508935747791273, -1.158461938185323392, 0.7296380582302550710 ) ) ;
#6099 = CARTESIAN_POINT ( 'NONE',  ( 0.4887808337931878744, -1.608878316057391400, -0.6385965546679245319 ) ) ;
#6098 = CARTESIAN_POINT ( 'NONE',  ( -0.1642263571684416112, 0.5103503754387010982, 0.1528658435937233773 ) ) ;
#6100 = CARTESIAN_POINT ( 'NONE',  ( 0.5003933895997771941, -1.101010879683239629, 0.6202731239902519178 ) ) ;
#6101 = EDGE_LOOP ( 'NONE', ( #11862, #7628, #29405, #36324 ) ) ;
#6102 = DATE_AND_TIME ( #22189, #4977 ) ;
#6103 =( REPRESENTATION_RELATIONSHIP ('NONE','NONE', #33020, #24383 ) REPRESENTATION_RELATIONSHIP_WITH_TRANSFORMATION ( #36217 )SHAPE_REPRESENTATION_RELATIONSHIP( ) );
#6104 = DIRECTION ( 'NONE',  ( -1.000000000000000000, -0.000000000000000000, -0.000000000000000000 ) ) ;
#6105 = ORIENTED_EDGE ( 'NONE', *, *, #11565, .T. ) ;
#6106 = VERTEX_POINT ( 'NONE', #24792 ) ;
#6107 =( BOUNDED_SURFACE ( )  B_SPLINE_SURFACE ( 3, 2, ( 
 ( #38032, #9844, #28781 ),
 ( #34544, #10055, #25694 ),
 ( #38227, #38632, #13340 ),
 ( #16848, #13936, #14148 ) ),
 .UNSPECIFIED., .F., .F., .T. ) 
 B_SPLINE_SURFACE_WITH_KNOTS ( ( 4, 4 ),
 ( 3, 3 ),
 ( 0.000000000000000000, 0.0003300252796214654259 ),
 ( 0.000000000000000000, 1.000000000000000000 ),
 .UNSPECIFIED. ) 
 GEOMETRIC_REPRESENTATION_ITEM ( )  RATIONAL_B_SPLINE_SURFACE ( (
 ( 1.000000000000000000, 0.4928180116091757101, 1.000000000000000000),
 ( 1.000000000000000000, 0.4791232869326966792, 1.000000000000000000),
 ( 1.000000000000000000, 0.4652192647841347783, 1.000000000000000000),
 ( 1.000000000000000000, 0.4512702095610768294, 1.000000000000000000) ) ) 
 REPRESENTATION_ITEM ( '' )  SURFACE ( )  );
#6108 = CARTESIAN_POINT ( 'NONE',  ( 0.2483516944684627248, -1.248337998612542687, 0.8972023426632544929 ) ) ;
#6110 = CARTESIAN_POINT ( 'NONE',  ( 0.1856984011870668194, -0.7578896140594062469, -0.005504663353492499946 ) ) ;
#6109 = CARTESIAN_POINT ( 'NONE',  ( 0.08978098643734212791, 0.000000000000000000, 0.000000000000000000 ) ) ;
#6111 = DIRECTION ( 'NONE',  ( -0.02995152272103777241, 0.7083160032631821146, -0.7052597718627959811 ) ) ;
#6112 = ORIENTED_EDGE ( 'NONE', *, *, #31657, .T. ) ;
#6113 = B_SPLINE_CURVE_WITH_KNOTS ( 'NONE', 3,
 ( #27709, #27513, #12285, #24841 ),
 .UNSPECIFIED., .F., .F.,
 ( 4, 4 ),
 ( 0.8401805954000729493, 1.000000000000000000 ),
 .UNSPECIFIED. ) ;
#6114 = CIRCLE ( 'NONE', #25846, 0.03000000000000022787 ) ;
#6115 = ORIENTED_EDGE ( 'NONE', *, *, #21991, .F. ) ;
#6116 = CARTESIAN_POINT ( 'NONE',  ( 0.4047361405965239078, -1.117070546656567132, 0.6130903832934563313 ) ) ;
#6117 = EDGE_CURVE ( 'NONE', #27170, #11941, #29365, .T. ) ;
#6118 = CARTESIAN_POINT ( 'NONE',  ( 0.4651104592015646855, -1.341950376707688797, 0.8227063177025514262 ) ) ;
#6119 = ORIENTED_EDGE ( 'NONE', *, *, #20219, .T. ) ;
#6120 = CARTESIAN_POINT ( 'NONE',  ( 0.1707094546937565349, -1.571949860022747947, -0.3635054096306748472 ) ) ;
#6121 = EDGE_CURVE ( 'NONE', #15679, #29483, #8931, .T. ) ;
#6122 = DIRECTION ( 'NONE',  ( 1.000000000000000000, 6.779273404243070203E-32, 4.314083075427408311E-32 ) ) ;
#6123 = VECTOR ( 'NONE', #17438, 39.37007874015748143 ) ;
#6124 = CIRCLE ( 'NONE', #4789, 0.06250000000000001388 ) ;
#6125 = CARTESIAN_POINT ( 'NONE',  ( -0.3000000000000000999, -4.015775813216793999, -0.6509878610687880318 ) ) ;
#6126 = EDGE_CURVE ( 'NONE', #10562, #13712, #15914, .T. ) ;
#6127 = CARTESIAN_POINT ( 'NONE',  ( -0.1129900121204308744, -0.5167580615070271888, 0.3146079272632520962 ) ) ;
#6128 = ADVANCED_FACE ( 'NONE', ( #5825 ), #29791, .T. ) ;
#6129 = CIRCLE ( 'NONE', #34386, 2.001674066779353556 ) ;
#6130 = DIRECTION ( 'NONE',  ( 0.8660254037844403729, 0.2563705595130079118, 0.4292716345334086081 ) ) ;
#6131 = CYLINDRICAL_SURFACE ( 'NONE', #20667, 0.04999999999999994726 ) ;
#6132 = CARTESIAN_POINT ( 'NONE',  ( -0.08000000000000000167, -2.032088213807425880, -0.4352898549974345555 ) ) ;
#6133 = VECTOR ( 'NONE', #40392, 39.37007874015748143 ) ;
#6134 = CARTESIAN_POINT ( 'NONE',  ( 0.07652314640226315356, -2.046395885474036724, -0.6781094798170426152 ) ) ;
#6135 = CARTESIAN_POINT ( 'NONE',  ( 0.05651694441833610832, -1.310850388052192894, 0.6148622741790434887 ) ) ;
#6136 = COORDINATED_UNIVERSAL_TIME_OFFSET ( 0, 0, .AHEAD. ) ;
#6137 = CARTESIAN_POINT ( 'NONE',  ( 0.1875000000000000833, -0.9151275355372969766, 0.1556228124470683261 ) ) ;
#6138 = B_SPLINE_CURVE_WITH_KNOTS ( 'NONE', 3,
 ( #28990, #12971, #16447, #25103, #12546, #10840 ),
 .UNSPECIFIED., .F., .F.,
 ( 4, 2, 4 ),
 ( 7.983724395024593614E-16, 0.0005669661630755714037, 0.001133932326150344401 ),
 .UNSPECIFIED. ) ;
#6139 = CARTESIAN_POINT ( 'NONE',  ( 0.4800703505524585579, -1.119839909059815897, 0.5356543536187720056 ) ) ;
#6140 = CARTESIAN_POINT ( 'NONE',  ( 0.4444713835028593629, -1.226065644031627766, 0.6057417262810037561 ) ) ;
#6141 = CARTESIAN_POINT ( 'NONE',  ( 0.5763338155049589906, -1.566475856062379934, -0.5858421376246120138 ) ) ;
#6142 = EDGE_CURVE ( 'NONE', #13011, #28606, #23642, .T. ) ;
#6143 = APPLIED_PERSON_AND_ORGANIZATION_ASSIGNMENT ( #27966, #9220, ( #17414 ) ) ;
#6144 = CARTESIAN_POINT ( 'NONE',  ( -0.003124719664520032511, -0.8057675726412022454, 0.1130684494947832019 ) ) ;
#6145 = DIRECTION ( 'NONE',  ( -0.3515883117872521946, -1.971562692052851690E-16, -0.9361547195921140485 ) ) ;
#6146 = TOROIDAL_SURFACE ( 'NONE', #39651, 0.05000000000000000971, 0.2000000000000000111 ) ;
#6147 = CARTESIAN_POINT ( 'NONE',  ( 0.1726184415752066714, -1.824553594176122617, -0.6822955034825700649 ) ) ;
#6148 = CARTESIAN_POINT ( 'NONE',  ( 0.2059273467974227778, -1.283046334493782803, -0.2869361388274796476 ) ) ;
#6149 = ORIENTED_EDGE ( 'NONE', *, *, #26795, .T. ) ;
#6150 = AXIS2_PLACEMENT_3D ( 'NONE', #19812, #36053, #7453 ) ;
#6151 = EDGE_LOOP ( 'NONE', ( #27999, #15134, #14648, #22133, #3974 ) ) ;
#6152 = AXIS2_PLACEMENT_3D ( 'NONE', #3345, #38309, #9529 ) ;
#6153 = CARTESIAN_POINT ( 'NONE',  ( -0.1208103506584059517, -0.5051587313117206213, 0.1401839043133220331 ) ) ;
#6154 = ORIENTED_EDGE ( 'NONE', *, *, #16072, .T. ) ;
#6155 = CARTESIAN_POINT ( 'NONE',  ( 0.03113248654051816583, -0.2793841226333812489, -0.1799682156082512696 ) ) ;
#6156 = DIRECTION ( 'NONE',  ( 0.4999551463232373427, -0.8660512985181134660, 0.000000000000000000 ) ) ;
#6157 = CARTESIAN_POINT ( 'NONE',  ( 0.4850466889450024688, -1.276291303272052646, 0.8070895406851786857 ) ) ;
#6159 = ORIENTED_EDGE ( 'NONE', *, *, #20846, .T. ) ;
#6158 = CARTESIAN_POINT ( 'NONE',  ( 0.009593988611378652040, -0.5674229550368337094, 0.04256757953983118098 ) ) ;
#6160 = VECTOR ( 'NONE', #31393, 39.37007874015748143 ) ;
#6161 = EDGE_LOOP ( 'NONE', ( #8569, #3636, #19069, #27869 ) ) ;
#6162 = CYLINDRICAL_SURFACE ( 'NONE', #22545, 0.6114999999999938263 ) ;
#6163 = ORIENTED_EDGE ( 'NONE', *, *, #28999, .F. ) ;
#6164 = VECTOR ( 'NONE', #39498, 39.37007874015748143 ) ;
#6165 = CARTESIAN_POINT ( 'NONE',  ( 0.01081953179195768375, -0.5297023241700837826, 0.1548607054831544205 ) ) ;
#6167 = CARTESIAN_POINT ( 'NONE',  ( 0.08350584784635078917, -1.306523181150644364, 0.5696879678309485495 ) ) ;
#6166 = CARTESIAN_POINT ( 'NONE',  ( 0.4349570274192550712, -1.230519544206422733, 0.5941052033352403061 ) ) ;
#6168 = DIRECTION ( 'NONE',  ( 0.8660512985181135770, 0.4999551463232370652, 0.000000000000000000 ) ) ;
#6169 = CARTESIAN_POINT ( 'NONE',  ( 0.4109281692855286106, -1.716037778611097409, -0.4237749387638956033 ) ) ;
#6171 = VERTEX_POINT ( 'NONE', #9939 ) ;
#6170 = ORIENTED_EDGE ( 'NONE', *, *, #510, .F. ) ;
#6172 = DIRECTION ( 'NONE',  ( -1.000000000000000000, -2.341930812374887555E-31, 1.664003471950578127E-31 ) ) ;
#6173 = CARTESIAN_POINT ( 'NONE',  ( 0.4159916692016358830, -1.069406866067976081, -0.5155029497116575543 ) ) ;
#6174 = CARTESIAN_POINT ( 'NONE',  ( -0.04947837552028811620, -0.4418396724781367690, 0.1804413675089040769 ) ) ;
#6175 = EDGE_CURVE ( 'NONE', #15591, #3151, #7434, .T. ) ;
#6176 = CARTESIAN_POINT ( 'NONE',  ( 0.5399288831475632655, -1.362507449995920217, 0.7674847699393548828 ) ) ;
#6177 = CARTESIAN_POINT ( 'NONE',  ( 0.6984993753693692353, -1.438786077763939852, 0.5682417262808782121 ) ) ;
#6178 = LINE ( 'NONE', #27593, #17194 ) ;
#6179 = VECTOR ( 'NONE', #20544, 39.37007874015748143 ) ;
#6180 = EDGE_CURVE ( 'NONE', #25148, #39255, #38117, .T. ) ;
#6181 = CARTESIAN_POINT ( 'NONE',  ( 0.3195334067233912001, -1.760651528094834939, 0.5793234143701277983 ) ) ;
#6182 = EDGE_CURVE ( 'NONE', #16401, #20994, #13227, .T. ) ;
#6183 = AXIS2_PLACEMENT_3D ( 'NONE', #11677, #2620, #27327 ) ;
#6184 = CARTESIAN_POINT ( 'NONE',  ( 0.07592650758779409537, -1.323220219138284026, 0.5682417262808779901 ) ) ;
#6185 = CARTESIAN_POINT ( 'NONE',  ( 0.2698036132048247104, -0.9625005881386677897, 0.7146062034794288254 ) ) ;
#6186 = CIRCLE ( 'NONE', #10127, 0.03000000000000000583 ) ;
#6187 = CARTESIAN_POINT ( 'NONE',  ( 0.3830853140175753957, -1.124506747416974761, 0.7559036875749386430 ) ) ;
#6188 = DIRECTION ( 'NONE',  ( 0.000000000000000000, 0.000000000000000000, -1.000000000000000000 ) ) ;
#6189 = DIRECTION ( 'NONE',  ( -0.4460749976721554155, -0.2575107168754576792, 0.8571495360472840552 ) ) ;
#6190 = APPROVAL_PERSON_ORGANIZATION ( #21402, #13213, #18092 ) ;
#6191 = CARTESIAN_POINT ( 'NONE',  ( 0.05076679145662076759, -0.2374648372614181491, 0.4099810879409593878 ) ) ;
#6192 = DIRECTION ( 'NONE',  ( -7.771561172376107616E-16, 7.170354002788761615E-17, -1.000000000000000000 ) ) ;
#6193 = VECTOR ( 'NONE', #5209, 39.37007874015748854 ) ;
#6194 = CARTESIAN_POINT ( 'NONE',  ( 0.03991172363000938111, -1.025282391162960938, 0.7023476162170446679 ) ) ;
#6195 = APPROVAL_ROLE ( '' ) ;
#6196 = CARTESIAN_POINT ( 'NONE',  ( 0.2870953417136587471, -0.7492508933039718766, 0.6466144559156578042 ) ) ;
#6197 = EDGE_CURVE ( 'NONE', #38396, #26954, #23679, .T. ) ;
#6198 = CARTESIAN_POINT ( 'NONE',  ( 0.01548846960707524721, 0.000000000000000000, 0.000000000000000000 ) ) ;
#6199 = FACE_OUTER_BOUND ( 'NONE', #29864, .T. ) ;
#6200 = CARTESIAN_POINT ( 'NONE',  ( -0.02000000000000000042, -2.320036485105098301, -0.2941690811493925528 ) ) ;
#6201 = CARTESIAN_POINT ( 'NONE',  ( 0.3706793757908085074, -1.615012852715396408, -0.4172838525897036854 ) ) ;
#6202 = ORIENTED_EDGE ( 'NONE', *, *, #6065, .F. ) ;
#6203 = CARTESIAN_POINT ( 'NONE',  ( 0.03113248654051816583, 0.1997995745459845707, -0.008951536808938304751 ) ) ;
#6204 = CARTESIAN_POINT ( 'NONE',  ( 0.2532909672037780280, -1.579627038668091732, 0.8749452808108927337 ) ) ;
#6205 = CIRCLE ( 'NONE', #29214, 0.1946589359789743512 ) ;
#6206 = CARTESIAN_POINT ( 'NONE',  ( 0.4608701369652646318, -1.284683416556681390, 0.8202635153794951561 ) ) ;
#6208 = ORIENTED_EDGE ( 'NONE', *, *, #17546, .T. ) ;
#6207 = DIRECTION ( 'NONE',  ( 0.000000000000000000, 0.000000000000000000, -1.000000000000000000 ) ) ;
#6209 = VECTOR ( 'NONE', #5460, 39.37007874015748143 ) ;
#6210 = B_SPLINE_CURVE_WITH_KNOTS ( 'NONE', 3,
 ( #25430, #9770, #12644, #571, #38150, #9973, #22543, #7646, #29655, #22752, #8252, #20824, #36224, #23513, #14014, #26586, #35833, #8447, #26974, #8038, #39127, #38348, #10951, #23697, #36028, #14842, #11138, #23909, #32735, #4956, #10183, #39508, #20210, #20614, #29867, #17906, #30070, #33148, #17520, #11558, #7832, #20403, #17107, #11339, #32935, #1899 ),
 .UNSPECIFIED., .F., .F.,
 ( 4, 2, 2, 2, 2, 2, 2, 2, 2, 2, 2, 2, 2, 2, 2, 2, 2, 2, 2, 2, 2, 2, 4 ),
 ( -6.000000007858409836E-08, 0.003552629519589487611, 0.007105319039179053796, 0.008881663798973832985, 0.01065800855876861478, 0.01154618093866600914, 0.01243435331856340177, 0.01421069807835819744, 0.01509887045825559528, 0.01598704283815299138, 0.01776338759794778357, 0.01865155997784517794, 0.01953973235774257231, 0.02131607711753736104, 0.02309242187733215323, 0.02398059425722953719, 0.02486876663712692115, 0.02575693901702430857, 0.02664511139692169253, 0.02753328377681907649, 0.02797736996676776153, 0.02819941306174210405, 0.02842145615671644310 ),
 .UNSPECIFIED. ) ;
#6211 = CARTESIAN_POINT ( 'NONE',  ( 0.2003179398552689949, -0.7109237300142917659, 0.3290305662194804026 ) ) ;
#6213 = ORIENTED_EDGE ( 'NONE', *, *, #18563, .F. ) ;
#6212 = VERTEX_POINT ( 'NONE', #4377 ) ;
#6214 = CARTESIAN_POINT ( 'NONE',  ( 0.5289566482161313088, -1.159595167906385393, 0.8177397053652041281 ) ) ;
#6215 = AXIS2_PLACEMENT_3D ( 'NONE', #35485, #7289, #32008 ) ;
#6216 = VECTOR ( 'NONE', #1891, 39.37007874015748854 ) ;
#6217 = CARTESIAN_POINT ( 'NONE',  ( 0.05283102792148738902, 0.4315398646667468197, -0.1819478359276330837 ) ) ;
#6218 = LOCAL_TIME ( 0, 53, 7.000000000000000000, #21684 ) ;
#6219 = DIRECTION ( 'NONE',  ( -0.4999551463232372317, 0.8660512985181135770, -0.000000000000000000 ) ) ;
#6220 = PERSON_AND_ORGANIZATION ( #21591, #7624 ) ;
#6221 = CARTESIAN_POINT ( 'NONE',  ( 0.3047812724409711960, -1.756857659564785568, 0.5654036402351543256 ) ) ;
#6222 = ORIENTED_EDGE ( 'NONE', *, *, #26367, .F. ) ;
#6223 = CARTESIAN_POINT ( 'NONE',  ( 0.09832617150614605950, -0.7626014107058197711, 0.3272609970532458501 ) ) ;
#6224 = AXIS2_PLACEMENT_3D ( 'NONE', #18857, #18029, #18237 ) ;
#6225 = CARTESIAN_POINT ( 'NONE',  ( 0.3254386620852590672, -1.747205596724848986, 0.7223889833057646204 ) ) ;
#6226 = CARTESIAN_POINT ( 'NONE',  ( 0.5259394649249050646, -1.526850962987742255, 0.5868731501866165656 ) ) ;
#6227 = CARTESIAN_POINT ( 'NONE',  ( 0.6421235886874124832, -1.453936924866673364, -0.6328608320660102926 ) ) ;
#6228 = CARTESIAN_POINT ( 'NONE',  ( -0.1631308187679522681, 0.4729065765976254165, 0.1187908002253836859 ) ) ;
#6229 = ORIENTED_EDGE ( 'NONE', *, *, #26883, .F. ) ;
#6230 = EDGE_CURVE ( 'NONE', #40011, #39872, #11625, .T. ) ;
#6231 = DIRECTION ( 'NONE',  ( -0.9848077530122080203, 0.000000000000000000, -0.1736481776669303589 ) ) ;
#6232 = CARTESIAN_POINT ( 'NONE',  ( 0.6631499315851888676, -1.372742098333818772, 0.7573330281475406656 ) ) ;
#6233 = B_SPLINE_CURVE_WITH_KNOTS ( 'NONE', 3,
 ( #26073, #25244, #35106, #28318 ),
 .UNSPECIFIED., .F., .F.,
 ( 4, 4 ),
 ( 2.914079691781330694E-05, 0.001162144789400721811 ),
 .UNSPECIFIED. ) ;
#6234 = CARTESIAN_POINT ( 'NONE',  ( 0.1061812928925085775, -1.412809043690689492, 0.5685481090398675219 ) ) ;
#6235 = CARTESIAN_POINT ( 'NONE',  ( 0.1914385470493136510, -0.8272674967231937737, 0.2680172446836712741 ) ) ;
#6236 = AXIS2_PLACEMENT_3D ( 'NONE', #17613, #39823, #21108 ) ;
#6237 = CARTESIAN_POINT ( 'NONE',  ( 0.3210085668004670767, -1.182910313946810010, 0.5197417262808780025 ) ) ;
#6238 = CIRCLE ( 'NONE', #25975, 0.1249999999999999584 ) ;
#6239 = CYLINDRICAL_SURFACE ( 'NONE', #11466, 0.1000000000000000194 ) ;
#6240 = CARTESIAN_POINT ( 'NONE',  ( 1.365923996832131609E-16, -0.9481888444201336252, 0.1622877746734860682 ) ) ;
#6241 = CARTESIAN_POINT ( 'NONE',  ( 0.1876168051218740918, -0.6873969840233377093, 0.1659352930446481023 ) ) ;
#6242 = VECTOR ( 'NONE', #9549, 39.37007874015748143 ) ;
#6243 = DATE_TIME_ROLE ( 'classification_date' ) ;
#6244 = CARTESIAN_POINT ( 'NONE',  ( 0.1905436384893574864, -0.5945559727383912252, 0.3046096357648204189 ) ) ;
#6245 = APPROVAL_PERSON_ORGANIZATION ( #21237, #36280, #37266 ) ;
#6246 = ADVANCED_FACE ( 'NONE', ( #10548 ), #19811, .F. ) ;
#6247 = EDGE_CURVE ( 'NONE', #8621, #20383, #10152, .T. ) ;
#6248 = CARTESIAN_POINT ( 'NONE',  ( 0.4899975086607765151, -1.544818463987469803, 0.5363230707130959285 ) ) ;
#6249 = CONICAL_SURFACE ( 'NONE', #9546, 0.1599999999999999201, 1.047197551196601406 ) ;
#6250 = CARTESIAN_POINT ( 'NONE',  ( -0.04140212552917823391, 0.01694508110950332727, 0.4702784328063239760 ) ) ;
#6251 = ORIENTED_EDGE ( 'NONE', *, *, #22501, .F. ) ;
#6252 = CARTESIAN_POINT ( 'NONE',  ( 0.4776788183558685064, -1.117332377667354049, 0.5554309925805337445 ) ) ;
#6253 = DIRECTION ( 'NONE',  ( -1.000000000000000000, -6.779273404243070203E-32, -4.314083075427408311E-32 ) ) ;
#6254 = CARTESIAN_POINT ( 'NONE',  ( 0.1854355241872554794, -0.8269808566380300041, 0.2443189868772147610 ) ) ;
#6255 = ORIENTED_EDGE ( 'NONE', *, *, #37358, .T. ) ;
#6256 = CARTESIAN_POINT ( 'NONE',  ( -0.01548846960707421332, 0.07651041855119253277, -0.5222379212568226681 ) ) ;
#6257 = CARTESIAN_POINT ( 'NONE',  ( -0.01106515159914605619, -0.8690226371807162620, 0.4019604355119212324 ) ) ;
#6259 = ORIENTED_EDGE ( 'NONE', *, *, #35088, .T. ) ;
#6258 = ORIENTED_EDGE ( 'NONE', *, *, #16789, .T. ) ;
#6260 = LINE ( 'NONE', #15535, #11978 ) ;
#6261 = CARTESIAN_POINT ( 'NONE',  ( -0.3000000000000000999, -3.194091454214595949, -0.5766534813907828738 ) ) ;
#6262 = CARTESIAN_POINT ( 'NONE',  ( 0.3592281729446684113, -1.923857150176657260, -0.3319732337371206765 ) ) ;
#6263 = AXIS2_PLACEMENT_3D ( 'NONE', #28848, #312, #38706 ) ;
#6265 = CARTESIAN_POINT ( 'NONE',  ( 0.4805029911762458417, -1.677157326917623648, 0.5488390883013556376 ) ) ;
#6264 = FACE_OUTER_BOUND ( 'NONE', #17105, .T. ) ;
#6266 = VERTEX_POINT ( 'NONE', #7238 ) ;
#6267 = AXIS2_PLACEMENT_3D ( 'NONE', #3808, #31799, #580 ) ;
#6268 = CARTESIAN_POINT ( 'NONE',  ( 0.2063381384019259968, -0.8323430845776256248, 0.6661612056125681969 ) ) ;
#6269 = ORIENTED_EDGE ( 'NONE', *, *, #2435, .T. ) ;
#6270 = EDGE_LOOP ( 'NONE', ( #9050, #40098, #24235, #27073 ) ) ;
#6271 = CARTESIAN_POINT ( 'NONE',  ( -0.1455608194604307570, -0.5249067277714107860, 0.3032895567580802809 ) ) ;
#6272 = CARTESIAN_POINT ( 'NONE',  ( 0.07288528088268256266, -0.5428011791350080273, 0.1723887882660675164 ) ) ;
#6274 = CARTESIAN_POINT ( 'NONE',  ( 0.5705380599090917881, -1.624401057953443361, 0.4891858033826676500 ) ) ;
#6273 = DIRECTION ( 'NONE',  ( 0.000000000000000000, 0.4798762827498445072, -0.8773361688966159200 ) ) ;
#6275 = CARTESIAN_POINT ( 'NONE',  ( -0.1969433606228592482, 0.5138636982738209458, 0.3032895567580813356 ) ) ;
#6276 = CARTESIAN_POINT ( 'NONE',  ( 0.2865981181406410117, -0.9694992659984323913, 0.5430900387768758941 ) ) ;
#6277 = CARTESIAN_POINT ( 'NONE',  ( 0.5184883810048313002, -1.679943727288017552, -0.5950377653840827064 ) ) ;
#6278 = ORIENTED_EDGE ( 'NONE', *, *, #13655, .T. ) ;
#6279 = EDGE_CURVE ( 'NONE', #14928, #7855, #10986, .T. ) ;
#6280 = CARTESIAN_POINT ( 'NONE',  ( 0.1180522936230993386, -1.414511114437261297, 0.5471422669605355837 ) ) ;
#6281 = CARTESIAN_POINT ( 'NONE',  ( 0.3925781617411475133, -1.721137056870122750, -0.3057750134661929020 ) ) ;
#6282 = CARTESIAN_POINT ( 'NONE',  ( 0.5806409787221022967, -1.495190593209716701, 0.5680879804946280531 ) ) ;
#6283 = CIRCLE ( 'NONE', #39126, 0.01499999999999995434 ) ;
#6284 = CARTESIAN_POINT ( 'NONE',  ( -0.04285534776242241189, 0.3459954891507885377, -0.3537381284079011423 ) ) ;
#6285 = LINE ( 'NONE', #27696, #8052 ) ;
#6286 = CARTESIAN_POINT ( 'NONE',  ( -0.01548846960707490547, 0.5198120922912040642, 0.07362328916749247276 ) ) ;
#6287 = CARTESIAN_POINT ( 'NONE',  ( 0.6394081393571972027, -1.397021802722361095, -0.6249999999999998890 ) ) ;
#6288 = PLANE ( 'NONE',  #13537 ) ;
#6289 = CARTESIAN_POINT ( 'NONE',  ( 0.2173028089842584942, -0.6047810126270140030, 0.4525757583899530645 ) ) ;
#6290 = CARTESIAN_POINT ( 'NONE',  ( -0.05269191099235786407, 0.2790572191958478054, 0.3764802596566349524 ) ) ;
#6291 = CARTESIAN_POINT ( 'NONE',  ( 0.04296213034915628143, -1.142534290635602856, 0.6595617262123023572 ) ) ;
#6292 = CIRCLE ( 'NONE', #35848, 0.1033070866141732880 ) ;
#6293 = CARTESIAN_POINT ( 'NONE',  ( 0.6436032348275867454, -1.487421782847565321, -0.4117819510330663624 ) ) ;
#6294 = AXIS2_PLACEMENT_3D ( 'NONE', #7274, #38973, #7489 ) ;
#6295 = CARTESIAN_POINT ( 'NONE',  ( 0.3986316166335497901, -2.053829379683854039, -0.4777570796616223414 ) ) ;
#6296 = DIRECTION ( 'NONE',  ( 0.000000000000000000, 0.000000000000000000, 1.000000000000000000 ) ) ;
#6297 = CARTESIAN_POINT ( 'NONE',  ( -0.05464101615137770263, -2.320036485105098301, -0.2941690811493925528 ) ) ;
#6298 = DIRECTION ( 'NONE',  ( 0.000000000000000000, 0.000000000000000000, -1.000000000000000000 ) ) ;
#6299 = LOCAL_TIME ( 0, 53, 7.000000000000000000, #4998 ) ;
#6300 = ORIENTED_EDGE ( 'NONE', *, *, #12169, .T. ) ;
#6301 = CARTESIAN_POINT ( 'NONE',  ( 0.3630210457930825307, -1.758320821885930751, -0.4950703529717556117 ) ) ;
#6302 = CARTESIAN_POINT ( 'NONE',  ( 0.4001970250685381592, -1.597972868323746187, -0.4118702688307778192 ) ) ;
#6303 = CARTESIAN_POINT ( 'NONE',  ( 0.6581239352572101353, -1.508981307375261371, 0.4182417262808776903 ) ) ;
#6304 = DIRECTION ( 'NONE',  ( 1.000000000000000000, 2.280301054154495132E-31, -1.664003471950577689E-31 ) ) ;
#6305 = DIRECTION ( 'NONE',  ( 1.060606950627616773E-16, 6.122684696619993730E-17, 1.000000000000000000 ) ) ;
#6306 = AXIS2_PLACEMENT_3D ( 'NONE', #9832, #7550, #31855 ) ;
#6307 = VERTEX_POINT ( 'NONE', #29477 ) ;
#6308 = CARTESIAN_POINT ( 'NONE',  ( 0.3795613398208534384, -1.760143698493221942, -0.5723197561600823491 ) ) ;
#6309 = CARTESIAN_POINT ( 'NONE',  ( -0.2399999999999999079, -3.253611865733782693, -0.3464478357516359575 ) ) ;
#6310 = DIRECTION ( 'NONE',  ( 0.000000000000000000, 0.000000000000000000, 1.000000000000000000 ) ) ;
#6311 = CARTESIAN_POINT ( 'NONE',  ( 0.5264113014007612001, -1.640729993778266893, -0.5166151207188711680 ) ) ;
#6312 = CARTESIAN_POINT ( 'NONE',  ( 0.4916533138082907484, -1.278983340569261884, 0.6751784830682899807 ) ) ;
#6314 = ORIENTED_EDGE ( 'NONE', *, *, #6683, .T. ) ;
#6313 = DIRECTION ( 'NONE',  ( 0.4999999999999979461, -0.03026636220570700850, -0.8654963589286988057 ) ) ;
#6315 = CARTESIAN_POINT ( 'NONE',  ( 0.1854168535569865883, -0.8697360073808750869, 0.1550939566555308846 ) ) ;
#6316 = ORIENTED_EDGE ( 'NONE', *, *, #14046, .F. ) ;
#6317 = PERSON_AND_ORGANIZATION ( #28500, #32463 ) ;
#6318 = CARTESIAN_POINT ( 'NONE',  ( 0.03830788332888396264, -1.018305589505236863, 0.6966598605597207339 ) ) ;
#6319 = ORIENTED_EDGE ( 'NONE', *, *, #15310, .T. ) ;
#6320 = CARTESIAN_POINT ( 'NONE',  ( 0.3853907798681502350, -1.605660261670780020, 0.5762609820462575305 ) ) ;
#6322 = CARTESIAN_POINT ( 'NONE',  ( 0.1124781747783372837, -0.7882225145822692181, -0.07339066647304182123 ) ) ;
#6321 = FACE_OUTER_BOUND ( 'NONE', #15826, .T. ) ;
#6323 = CARTESIAN_POINT ( 'NONE',  ( 0.3543078412078040085, -1.629008732304762397, -0.3717187814789204570 ) ) ;
#6324 = ORIENTED_EDGE ( 'NONE', *, *, #13749, .T. ) ;
#6325 = VERTEX_POINT ( 'NONE', #934 ) ;
#6326 = ORIENTED_EDGE ( 'NONE', *, *, #32447, .F. ) ;
#6327 = CARTESIAN_POINT ( 'NONE',  ( 0.4351293263873937667, -1.231514889939106849, 0.5832342842089121016 ) ) ;
#6328 = CARTESIAN_POINT ( 'NONE',  ( 0.1365985329653890135, -0.6540515576326647595, 0.4294670187197495714 ) ) ;
#6329 = ORIENTED_EDGE ( 'NONE', *, *, #28767, .F. ) ;
#6330 = CARTESIAN_POINT ( 'NONE',  ( 0.1860814369969508164, -0.7839612642874815851, 0.05803861901368200654 ) ) ;
#6331 = CIRCLE ( 'NONE', #8328, 0.06000000000000031697 ) ;
#6332 = DIRECTION ( 'NONE',  ( 0.000000000000000000, 0.000000000000000000, -1.000000000000000000 ) ) ;
#6333 = CARTESIAN_POINT ( 'NONE',  ( 0.05999999999999990757, 0.7171888913565960255, -0.3575238883388469069 ) ) ;
#6334 = APPROVAL_PERSON_ORGANIZATION ( #17699, #4473, #36820 ) ;
#6335 = CARTESIAN_POINT ( 'NONE',  ( 0.07251299243635034308, -1.415239065497081006, -0.3692912077930444736 ) ) ;
#6336 = CARTESIAN_POINT ( 'NONE',  ( 0.5872629042297322632, -1.489983250153556815, -0.4326885114256821541 ) ) ;
#6337 = CARTESIAN_POINT ( 'NONE',  ( -0.2399999999999999079, -3.941790907013290823, -0.4709369376873030477 ) ) ;
#6338 = CIRCLE ( 'NONE', #11613, 0.2500000000000000000 ) ;
#6339 = CARTESIAN_POINT ( 'NONE',  ( 1.530770926392632502E-17, 0.06117178301711245075, 0.1249999999999993477 ) ) ;
#6340 = CARTESIAN_POINT ( 'NONE',  ( 0.2110034642138055860, -1.187742706213460453, -0.5155029497116575543 ) ) ;
#6341 = CARTESIAN_POINT ( 'NONE',  ( 0.01548846960712797240, 0.07651041855115807422, 0.5222379212567064277 ) ) ;
#6342 = DIRECTION ( 'NONE',  ( -0.8660512985181141321, -0.4999551463232362325, 0.000000000000000000 ) ) ;
#6343 = DIRECTION ( 'NONE',  ( -1.000000000000000000, -0.000000000000000000, -0.000000000000000000 ) ) ;
#6344 = PERSON_AND_ORGANIZATION_ROLE ( 'classification_officer' ) ;
#6345 = CARTESIAN_POINT ( 'NONE',  ( 0.4383612739836618144, -1.052766492039166391, 0.6342478131430038246 ) ) ;
#6346 = DIRECTION ( 'NONE',  ( 1.000000000000000000, 2.280301054154495132E-31, -1.664003471950577689E-31 ) ) ;
#6347 = CARTESIAN_POINT ( 'NONE',  ( 0.5494029794155456115, -1.165490604795236029, 0.6057417262810063097 ) ) ;
#6348 = VERTEX_POINT ( 'NONE', #13442 ) ;
#6349 = CARTESIAN_POINT ( 'NONE',  ( 0.1512804210101734992, -1.367800832853933501, 0.8372142429942934783 ) ) ;
#6350 = FACE_OUTER_BOUND ( 'NONE', #13855, .T. ) ;
#6351 = CARTESIAN_POINT ( 'NONE',  ( 0.1945550857237052511, -2.003382580491667841, -0.7031198838846081101 ) ) ;
#6352 = AXIS2_PLACEMENT_3D ( 'NONE', #21083, #27053, #5420 ) ;
#6353 = CARTESIAN_POINT ( 'NONE',  ( 0.3218706003014081274, -1.643225927452630852, 0.4993898684233093466 ) ) ;
#6354 = EDGE_CURVE ( 'NONE', #31920, #6106, #38530, .T. ) ;
#6355 = ADVANCED_FACE ( 'NONE', ( #1135 ), #13635, .T. ) ;
#6356 = ORIENTED_EDGE ( 'NONE', *, *, #7687, .T. ) ;
#6357 = AXIS2_PLACEMENT_3D ( 'NONE', #25111, #34361, #8862 ) ;
#6358 = ORIENTED_EDGE ( 'NONE', *, *, #11992, .T. ) ;
#6359 = CARTESIAN_POINT ( 'NONE',  ( 0.01548846960707524721, 0.000000000000000000, 0.000000000000000000 ) ) ;
#6360 = ORIENTED_EDGE ( 'NONE', *, *, #37822, .T. ) ;
#6361 = CARTESIAN_POINT ( 'NONE',  ( 0.5215316005982619796, -1.181669392490712456, -0.6250000000000000000 ) ) ;
#6362 = CARTESIAN_POINT ( 'NONE',  ( -0.05634301242525809744, -0.4396003943662958324, -0.1320237143668771818 ) ) ;
#6363 = EDGE_CURVE ( 'NONE', #14915, #6802, #30009, .T. ) ;
#6364 = CARTESIAN_POINT ( 'NONE',  ( 0.4600226136112777198, -1.237287929595064062, 0.8135617580924977554 ) ) ;
#6366 = ORIENTED_EDGE ( 'NONE', *, *, #5165, .T. ) ;
#6365 = CARTESIAN_POINT ( 'NONE',  ( 0.001804213231561386209, -0.5433067823503371363, 0.07704719339775437104 ) ) ;
#6367 = ADVANCED_FACE ( 'NONE', ( #5368 ), #21478, .T. ) ;
#6368 = ORIENTED_EDGE ( 'NONE', *, *, #17280, .T. ) ;
#6369 = CARTESIAN_POINT ( 'NONE',  ( 0.5737921459139804226, -1.611029524247286293, 0.4522236539011413869 ) ) ;
#6370 = EDGE_LOOP ( 'NONE', ( #25420, #4478, #33032 ) ) ;
#6371 = CARTESIAN_POINT ( 'NONE',  ( 0.1840027845416183361, -1.200052452841920303, 0.9022922089355089881 ) ) ;
#6373 = CARTESIAN_POINT ( 'NONE',  ( 0.3695052819757340123, -1.758428263776099287, -0.4278193900811940176 ) ) ;
#6372 = CARTESIAN_POINT ( 'NONE',  ( 0.2800658575624323521, -1.022046468236217143, 0.7264731327323665777 ) ) ;
#6374 = CARTESIAN_POINT ( 'NONE',  ( 0.5849095050029387011, -1.491341823319836335, -0.5960747874205124530 ) ) ;
#6375 = DIRECTION ( 'NONE',  ( -1.000000000000000000, -7.857794173099924470E-32, -8.628166150854818811E-32 ) ) ;
#6376 = CARTESIAN_POINT ( 'NONE',  ( 0.4100456123093286775, -1.725225710419908243, -0.4268450903248972028 ) ) ;
#6378 = ORIENTED_EDGE ( 'NONE', *, *, #28608, .F. ) ;
#6377 = ORIENTED_EDGE ( 'NONE', *, *, #12396, .T. ) ;
#6379 = FACE_OUTER_BOUND ( 'NONE', #9022, .T. ) ;
#6380 = CARTESIAN_POINT ( 'NONE',  ( -0.05464101615137766793, -2.548345659627495596, -0.2263512047145338490 ) ) ;
#6381 = CARTESIAN_POINT ( 'NONE',  ( -0.01548846960707318636, -0.5203207976467986162, 0.08861466064781882424 ) ) ;
#6382 = LINE ( 'NONE', #35192, #29275 ) ;
#6383 = ADVANCED_FACE ( 'NONE', ( #4978 ), #26914, .F. ) ;
#6384 = CARTESIAN_POINT ( 'NONE',  ( 0.1592870015680986351, -0.8540808306954126294, 0.4623900724923409311 ) ) ;
#6385 = DIRECTION ( 'NONE',  ( -1.000000000000000000, -0.000000000000000000, -0.000000000000000000 ) ) ;
#6386 = PRODUCT_DEFINITION ( 'UNKNOWN', '', #24016, #39289 ) ;
#6387 = CARTESIAN_POINT ( 'NONE',  ( 0.1938292101578000248, -1.228094556586287300, 1.021854484236047522 ) ) ;
#6388 = LINE ( 'NONE', #28010, #25162 ) ;
#6389 = CARTESIAN_POINT ( 'NONE',  ( 0.07556315841227354002, -1.331191507351498160, 0.4849083929475443422 ) ) ;
#6390 = CARTESIAN_POINT ( 'NONE',  ( 0.3704697912810950289, -1.166474544107111599, 0.4282417262808793090 ) ) ;
#6391 = DIRECTION ( 'NONE',  ( -0.000000000000000000, 0.9679004486746793923, 0.2513338844154409668 ) ) ;
#6392 = CARTESIAN_POINT ( 'NONE',  ( -0.07999999999999996003, -3.941790907013290823, -0.4709369376873033253 ) ) ;
#6393 = DIRECTION ( 'NONE',  ( -6.162975822039154046E-33, 0.000000000000000000, -1.000000000000000000 ) ) ;
#6394 = CARTESIAN_POINT ( 'NONE',  ( 0.3098984767712536503, -1.765718780359063267, 0.5682417262808785452 ) ) ;
#6395 = CARTESIAN_POINT ( 'NONE',  ( 0.05438524155173456165, -1.080864667231560716, 0.7434867514774906594 ) ) ;
#6396 = PERSON_AND_ORGANIZATION ( #28500, #32463 ) ;
#6397 = CARTESIAN_POINT ( 'NONE',  ( -0.03174060074381365032, 0.4701996045334384533, 0.2325360656123088010 ) ) ;
#6398 = CARTESIAN_POINT ( 'NONE',  ( 0.7030074634613492357, -1.521190031500555317, 0.5774844009317151583 ) ) ;
#6399 = EDGE_CURVE ( 'NONE', #37899, #839, #5026, .T. ) ;
#6400 = CARTESIAN_POINT ( 'NONE',  ( 0.3402612271582353687, -1.674021245575775696, -0.3988557406434431463 ) ) ;
#6401 = ORIENTED_EDGE ( 'NONE', *, *, #21504, .F. ) ;
#6402 = DIRECTION ( 'NONE',  ( 0.8660512985181129109, 0.4999551463232381199, 0.000000000000000000 ) ) ;
#6403 = CARTESIAN_POINT ( 'NONE',  ( 0.2664482867961980306, -1.636644802795437892, 0.8064424891061348077 ) ) ;
#6404 = ADVANCED_FACE ( 'NONE', ( #17129 ), #14643, .F. ) ;
#6405 = CARTESIAN_POINT ( 'NONE',  ( 0.2204199330889215214, -0.8297487780498332688, 0.6443566085987398884 ) ) ;
#6407 = ORIENTED_EDGE ( 'NONE', *, *, #32103, .T. ) ;
#6406 = CARTESIAN_POINT ( 'NONE',  ( 0.5433647090050529593, -1.169020713861581129, 0.5880578810646379662 ) ) ;
#6408 = EDGE_CURVE ( 'NONE', #8492, #25716, #18287, .T. ) ;
#6410 = EDGE_LOOP ( 'NONE', ( #17000, #9465, #9950, #3582 ) ) ;
#6409 = ORIENTED_EDGE ( 'NONE', *, *, #13256, .T. ) ;
#6411 = CARTESIAN_POINT ( 'NONE',  ( 0.4391485520781965302, -1.022841741781851388, 0.7808255053512450639 ) ) ;
#6412 = CARTESIAN_POINT ( 'NONE',  ( -0.3000000000000000999, -2.289343986263487896, -0.6686455968847019316 ) ) ;
#6413 = DIRECTION ( 'NONE',  ( 1.000000000000000000, -0.000000000000000000, -0.000000000000000000 ) ) ;
#6414 = COORDINATED_UNIVERSAL_TIME_OFFSET ( 0, 0, .AHEAD. ) ;
#6415 = CARTESIAN_POINT ( 'NONE',  ( 0.3186747540252977684, -1.760357293763689546, 0.5625916045222835171 ) ) ;
#6416 = ORIENTED_EDGE ( 'NONE', *, *, #9925, .F. ) ;
#6417 = CARTESIAN_POINT ( 'NONE',  ( 0.1078177687349250041, -0.7744679009142783066, 0.3837020403678208513 ) ) ;
#6418 = CARTESIAN_POINT ( 'NONE',  ( 0.1757500541653520820, -1.230771478115229245, -0.2869361388274796476 ) ) ;
#6419 = CARTESIAN_POINT ( 'NONE',  ( 0.5252367033251564843, -1.526871148930892153, 0.5736917532057838054 ) ) ;
#6420 = CARTESIAN_POINT ( 'NONE',  ( 0.5802494246892667684, -1.607235576111437636, -0.5644493929225152806 ) ) ;
#6421 = EDGE_CURVE ( 'NONE', #28686, #17786, #39529, .T. ) ;
#6422 = CARTESIAN_POINT ( 'NONE',  ( 0.02953079040095728247, 0.000000000000000000, 0.000000000000000000 ) ) ;
#6423 = ORIENTED_EDGE ( 'NONE', *, *, #15220, .T. ) ;
#6424 = CARTESIAN_POINT ( 'NONE',  ( 0.4140281424214005135, -1.705551847233233831, 0.6094650255398795791 ) ) ;
#6425 = CARTESIAN_POINT ( 'NONE',  ( 0.6658116889046563625, -1.561543021530046094, 0.5673474868851250408 ) ) ;
#6426 = CARTESIAN_POINT ( 'NONE',  ( 0.2101951102887192890, -1.233953443661628846, 0.5631135429232324574 ) ) ;
#6427 = CARTESIAN_POINT ( 'NONE',  ( 0.6053889014930310397, -1.470157484751941634, 0.6617915113480205003 ) ) ;
#6428 = DIRECTION ( 'NONE',  ( -0.4999551463232362325, 0.8660512985181140211, 0.000000000000000000 ) ) ;
#6429 = SHAPE_REPRESENTATION_RELATIONSHIP ( 'NONE' , 'NONE' ,  #9349, #33372 ) ;
#6430 = DIRECTION ( 'NONE',  ( 0.000000000000000000, 0.000000000000000000, -1.000000000000000000 ) ) ;
#6431 = CARTESIAN_POINT ( 'NONE',  ( 0.2642159376432997031, -1.676617828451314907, 0.5053660846951645302 ) ) ;
#6432 = CARTESIAN_POINT ( 'NONE',  ( 0.07801557919154505916, -1.344960384177054546, 0.6336995499099050688 ) ) ;
#6433 = CARTESIAN_POINT ( 'NONE',  ( 0.2316395767834320274, -0.8375294501127626967, 0.4569101180231894821 ) ) ;
#6434 = APPROVAL_DATE_TIME ( #13224, #23269 ) ;
#6435 = DIRECTION ( 'NONE',  ( -7.771561172376107616E-16, 7.170354002788761615E-17, -1.000000000000000000 ) ) ;
#6436 = CARTESIAN_POINT ( 'NONE',  ( 0.5374399095249312586, -1.518357447092129497, 0.5359417805910808852 ) ) ;
#6437 = AXIS2_PLACEMENT_3D ( 'NONE', #25429, #16764, #19039 ) ;
#6438 = CARTESIAN_POINT ( 'NONE',  ( -0.03674260963082575521, 0.04074834683009517095, 0.4790483961530583312 ) ) ;
#6439 = EDGE_CURVE ( 'NONE', #28686, #7245, #12275, .T. ) ;
#6440 = ORIENTED_EDGE ( 'NONE', *, *, #10499, .F. ) ;
#6441 = LINE ( 'NONE', #938, #14798 ) ;
#6442 = CARTESIAN_POINT ( 'NONE',  ( 2.185478394931410575E-15, -0.2949999999999994293, -9.902948977032954413E-16 ) ) ;
#6443 = ADVANCED_FACE ( 'NONE', ( #8473 ), #34616, .T. ) ;
#6444 = CARTESIAN_POINT ( 'NONE',  ( 0.1920071873703446952, -0.8110264159798785677, 0.2735051980380693304 ) ) ;
#6445 = ORIENTED_EDGE ( 'NONE', *, *, #33421, .F. ) ;
#6446 = CARTESIAN_POINT ( 'NONE',  ( 0.000000000000000000, -0.6872203660140440151, 0.1457185332388702681 ) ) ;
#6447 = EDGE_CURVE ( 'NONE', #35222, #10169, #10313, .T. ) ;
#6448 = CARTESIAN_POINT ( 'NONE',  ( 0.1442265625138574037, -1.313102518721056100, 0.7083091578507269004 ) ) ;
#6450 = ORIENTED_EDGE ( 'NONE', *, *, #29933, .T. ) ;
#6449 = ORIENTED_EDGE ( 'NONE', *, *, #22513, .T. ) ;
#6451 = CARTESIAN_POINT ( 'NONE',  ( -0.08000000000000000167, -1.622350287959229087, -0.08960079202753243321 ) ) ;
#6452 = EDGE_LOOP ( 'NONE', ( #31543, #15427, #26564, #3095 ) ) ;
#6453 = CARTESIAN_POINT ( 'NONE',  ( 0.09972103128818979312, -1.308064159787032832, 0.4441314049251992024 ) ) ;
#6454 = B_SPLINE_CURVE_WITH_KNOTS ( 'NONE', 3,
 ( #32299, #22267, #10501, #25748 ),
 .UNSPECIFIED., .F., .F.,
 ( 4, 4 ),
 ( 3.576224061345491846E-18, 0.003042297940109665259 ),
 .UNSPECIFIED. ) ;
#6455 = CARTESIAN_POINT ( 'NONE',  ( 0.2655705318850531960, -1.562522136089427471, -0.3463398766974524201 ) ) ;
#6457 = CARTESIAN_POINT ( 'NONE',  ( -0.05464101615137770263, -2.183180860297908144, -0.4937760292030871079 ) ) ;
#6456 = CARTESIAN_POINT ( 'NONE',  ( 0.04047161733259613953, 0.4536038223829707006, 0.2133268955647583121 ) ) ;
#6458 = CARTESIAN_POINT ( 'NONE',  ( 0.04229974373173535362, -0.2824305679197178232, -0.3740363831607549927 ) ) ;
#6459 = ORIENTED_EDGE ( 'NONE', *, *, #6660, .F. ) ;
#6460 = CARTESIAN_POINT ( 'NONE',  ( -0.02000000000000000042, -2.212972691094449385, -0.5913464432512408608 ) ) ;
#6461 = ORIENTED_EDGE ( 'NONE', *, *, #9883, .F. ) ;
#6462 = VERTEX_POINT ( 'NONE', #31104 ) ;
#6463 = CARTESIAN_POINT ( 'NONE',  ( 0.1370807591037170314, -0.7115665574697015439, 0.5098665575104406322 ) ) ;
#6464 = ORIENTED_EDGE ( 'NONE', *, *, #31027, .F. ) ;
#6465 = ORIENTED_EDGE ( 'NONE', *, *, #24649, .T. ) ;
#6466 = DIRECTION ( 'NONE',  ( 8.881784197001246407E-16, -2.361472542561082612E-16, 1.000000000000000000 ) ) ;
#6467 = CARTESIAN_POINT ( 'NONE',  ( 0.08383286731608259601, -0.6201591115495469486, 0.3831915389127222848 ) ) ;
#6468 = EDGE_CURVE ( 'NONE', #34414, #6462, #38538, .T. ) ;
#6470 = DIRECTION ( 'NONE',  ( -0.2147743920926310501, -0.9766636885342062646, -4.525659028955483907E-15 ) ) ;
#6469 = CARTESIAN_POINT ( 'NONE',  ( 0.002464792031906918451, -0.5324439718320103099, 0.2218667994837078550 ) ) ;
#6471 = CARTESIAN_POINT ( 'NONE',  ( 0.4173105138104912237, -1.590421242443905037, -0.4142386051757726007 ) ) ;
#6472 = CARTESIAN_POINT ( 'NONE',  ( 0.3880537965025097624, -1.025164508700765031, 0.6277837196461664160 ) ) ;
#6473 = EDGE_CURVE ( 'NONE', #29444, #38406, #37065, .T. ) ;
#6474 = DIRECTION ( 'NONE',  ( 0.8660512985181134660, 0.4999551463232371207, 0.000000000000000000 ) ) ;
#6475 = ADVANCED_FACE ( 'NONE', ( #28028 ), #31341, .T. ) ;
#6476 = CARTESIAN_POINT ( 'NONE',  ( 0.4298148400247139844, -1.697909782648775678, -0.5124330163259216420 ) ) ;
#6477 = CARTESIAN_POINT ( 'NONE',  ( 0.1262144102814217184, -0.5727411025276200052, 0.2466681503346596915 ) ) ;
#6478 = CARTESIAN_POINT ( 'NONE',  ( -0.04293701532779567454, 0.2295363440003043154, 0.4381116105132950023 ) ) ;
#6479 = FACE_BOUND ( 'NONE', #12469, .T. ) ;
#6480 = CARTESIAN_POINT ( 'NONE',  ( -0.03642997641689288413, -0.4544357765433681418, -0.2357005667431724405 ) ) ;
#6481 = CARTESIAN_POINT ( 'NONE',  ( 0.07565767122873574835, -0.5864987862812711672, 0.3100368675900313509 ) ) ;
#6482 = FACE_OUTER_BOUND ( 'NONE', #18724, .T. ) ;
#6483 = CARTESIAN_POINT ( 'NONE',  ( 0.2790103250938448243, -0.7681568326658522183, 0.6036499921438334137 ) ) ;
#6484 = CARTESIAN_POINT ( 'NONE',  ( 0.4738611546896250859, -1.197946575156342286, 0.3905537834340729320 ) ) ;
#6485 = CARTESIAN_POINT ( 'NONE',  ( 0.02686770367197182513, -1.121034573699498216, 0.6519664731740556496 ) ) ;
#6486 = CARTESIAN_POINT ( 'NONE',  ( 0.5936523516255933774, -1.587486488880259339, -0.4320271970693849717 ) ) ;
#6487 = DIRECTION ( 'NONE',  ( 0.000000000000000000, 4.966996352116840709E-15, -1.000000000000000000 ) ) ;
#6488 = CARTESIAN_POINT ( 'NONE',  ( 0.1407851177556478373, -0.8464084508146803021, 0.4976936549835760948 ) ) ;
#6489 = CARTESIAN_POINT ( 'NONE',  ( 0.04230188431063448828, 0.2683773510969753029, -0.3842417364743022090 ) ) ;
#6490 = CARTESIAN_POINT ( 'NONE',  ( 0.1909286924077255587, -1.257064795538239022, -0.6485234391946320676 ) ) ;
#6491 = ORIENTED_EDGE ( 'NONE', *, *, #27622, .F. ) ;
#6492 = PLANE ( 'NONE',  #12804 ) ;
#6493 = CARTESIAN_POINT ( 'NONE',  ( 0.3606017550323884491, -1.088889236884987843, 0.7735338957822750494 ) ) ;
#6494 = CARTESIAN_POINT ( 'NONE',  ( 0.3660575152562974277, -2.015971804995021710, -0.5197529562823309801 ) ) ;
#6495 = ADVANCED_FACE ( 'NONE', ( #40557 ), #30039, .F. ) ;
#6496 = DIRECTION ( 'NONE',  ( 1.000000000000000000, 0.000000000000000000, 0.000000000000000000 ) ) ;
#6497 = DIRECTION ( 'NONE',  ( 0.000000000000000000, 0.000000000000000000, -1.000000000000000000 ) ) ;
#6498 = EDGE_CURVE ( 'NONE', #24445, #27427, #17556, .T. ) ;
#6499 = VERTEX_POINT ( 'NONE', #5985 ) ;
#6500 = CARTESIAN_POINT ( 'NONE',  ( 0.3903816190474082570, -1.614399842932418894, -0.6685306478358077342 ) ) ;
#6501 = DIRECTION ( 'NONE',  ( 0.4999551463232372317, -0.8660512985181135770, 0.000000000000000000 ) ) ;
#6502 = CARTESIAN_POINT ( 'NONE',  ( -0.8248651029816859159, -3.413936256264365647E-16, 0.6154198107346400271 ) ) ;
#6503 = CARTESIAN_POINT ( 'NONE',  ( 0.03301162916268060576, 0.3732432789822053287, -0.3635092914618242577 ) ) ;
#6504 = CARTESIAN_POINT ( 'NONE',  ( 0.3632630838000410756, -1.100250190083209789, 0.7354547643755756647 ) ) ;
#6506 = CARTESIAN_POINT ( 'NONE',  ( 0.3959972151391356610, -1.707195898057176642, 0.4182417262808776903 ) ) ;
#6505 = DIRECTION ( 'NONE',  ( 0.000000000000000000, 3.330669073875469621E-16, 1.000000000000000000 ) ) ;
#6507 = CARTESIAN_POINT ( 'NONE',  ( 0.4929465528686912679, -1.082715557938388029, 0.5639242819095140469 ) ) ;
#6508 = ORIENTED_EDGE ( 'NONE', *, *, #29068, .F. ) ;
#6509 = COORDINATED_UNIVERSAL_TIME_OFFSET ( 0, 0, .AHEAD. ) ;
#6510 = CARTESIAN_POINT ( 'NONE',  ( 0.6498387395261642219, -1.464631408770378451, 0.4282417262808778102 ) ) ;
#6511 = EDGE_LOOP ( 'NONE', ( #11984, #18840, #1998, #25969 ) ) ;
#6512 = EDGE_LOOP ( 'NONE', ( #29644, #31212, #38895, #20689, #19181, #3503, #25850, #15181, #28480 ) ) ;
#6513 = CARTESIAN_POINT ( 'NONE',  ( 0.3875464983679292041, -1.604953645996557432, 0.6166661730678868469 ) ) ;
#6515 = CARTESIAN_POINT ( 'NONE',  ( 0.1129260651966456502, -0.7196690655787660873, -0.09367555582725564656 ) ) ;
#6514 = CARTESIAN_POINT ( 'NONE',  ( 4.898587196579362494E-18, -0.3899999999999999578, -0.03999999999999947348 ) ) ;
#6516 = CARTESIAN_POINT ( 'NONE',  ( 0.3475531016022769815, -1.635599610428785766, -0.3752212724818577705 ) ) ;
#6517 = ORIENTED_EDGE ( 'NONE', *, *, #19111, .F. ) ;
#6518 = ORIENTED_EDGE ( 'NONE', *, *, #31034, .F. ) ;
#6519 = ORIENTED_EDGE ( 'NONE', *, *, #10978, .T. ) ;
#6520 = DIRECTION ( 'NONE',  ( 0.000000000000000000, 0.1725921171157359935, 0.9849933812516245002 ) ) ;
#6521 = CARTESIAN_POINT ( 'NONE',  ( 0.5435177775687849433, -1.464638892555605754, 0.7383152199638944868 ) ) ;
#6522 = ORIENTED_EDGE ( 'NONE', *, *, #16568, .F. ) ;
#6523 = CARTESIAN_POINT ( 'NONE',  ( 0.1873417209643421233, -0.6975452635715222449, 0.03245562858311761001 ) ) ;
#6524 = DIRECTION ( 'NONE',  ( 0.000000000000000000, 0.000000000000000000, -1.000000000000000000 ) ) ;
#6525 = DIRECTION ( 'NONE',  ( 1.000000000000000000, 2.341930812374887555E-31, -1.664003471950578127E-31 ) ) ;
#6526 = DIRECTION ( 'NONE',  ( 1.000000000000000000, 1.118011712966791197E-31, -7.771561172376107616E-16 ) ) ;
#6527 = EDGE_LOOP ( 'NONE', ( #27167, #1812, #25820, #2784 ) ) ;
#6528 = DIRECTION ( 'NONE',  ( 1.060606950627616897E-16, 6.122684696619992497E-17, 1.000000000000000000 ) ) ;
#6529 = CARTESIAN_POINT ( 'NONE',  ( 0.4527140395159202080, -1.709300500385005250, 0.5182417262812423209 ) ) ;
#6530 = CARTESIAN_POINT ( 'NONE',  ( 0.3795613398208533273, -1.760143698493221942, -0.5723197561600822381 ) ) ;
#6531 = LINE ( 'NONE', #12718, #40272 ) ;
#6532 = DIRECTION ( 'NONE',  ( -1.000000000000000000, -7.857794173099924470E-32, -8.628166150854818811E-32 ) ) ;
#6533 = LINE ( 'NONE', #226, #827 ) ;
#6534 = CARTESIAN_POINT ( 'NONE',  ( 0.4167140344599875590, -1.721376155575082612, -0.4397180493288434522 ) ) ;
#6535 = CARTESIAN_POINT ( 'NONE',  ( 0.3402623241359036266, -1.675594047157907163, -0.3998012311158237742 ) ) ;
#6536 = CALENDAR_DATE ( 2026, 13, 10 ) ;
#6537 = CARTESIAN_POINT ( 'NONE',  ( 0.4471380481896147785, -1.057582006303192657, 0.6325253032963528144 ) ) ;
#6538 = DIRECTION ( 'NONE',  ( 0.000000000000000000, 0.000000000000000000, -1.000000000000000000 ) ) ;
#6539 = CARTESIAN_POINT ( 'NONE',  ( 0.5145696469471491286, -1.185649477150961806, 0.5856983068964181083 ) ) ;
#6540 = CARTESIAN_POINT ( 'NONE',  ( 0.2623806002910373247, -1.682816372174909203, 0.5558257937731609921 ) ) ;
#6541 = CARTESIAN_POINT ( 'NONE',  ( -0.002083146443013344888, -0.8967360763018595859, 0.09758087637170891060 ) ) ;
#6542 = CARTESIAN_POINT ( 'NONE',  ( -0.0002645986387457673820, -0.8856723859976365354, -0.006055055896265703307 ) ) ;
#6543 = B_SPLINE_CURVE_WITH_KNOTS ( 'NONE', 3,
 ( #32065, #5987, #28966, #16424, #832, #37268, #3873, #18549, #15476, #28031, #40558, #12379, #9280, #35541, #24934, #13341, #9085, #12575 ),
 .UNSPECIFIED., .F., .F.,
 ( 4, 2, 2, 2, 2, 2, 2, 2, 4 ),
 ( -0.003133633995111254067, -0.002350221109836764244, -0.001566808224562274855, -0.0007833953392877854652, 1.754598670435786323E-08, 0.0007834304312611941809, 0.001566843316535683137, 0.002350256201810172960, 0.003133669087084662783 ),
 .UNSPECIFIED. ) ;
#6544 = CARTESIAN_POINT ( 'NONE',  ( 0.1747054245739551037, -1.734794744728702653, -0.6813247353107599880 ) ) ;
#6545 = CARTESIAN_POINT ( 'NONE',  ( 0.2320387611536686712, -1.233193230799448203, 0.4282290774773019337 ) ) ;
#6546 = ORIENTED_EDGE ( 'NONE', *, *, #28124, .T. ) ;
#6547 = ORIENTED_EDGE ( 'NONE', *, *, #30034, .T. ) ;
#6548 = DIRECTION ( 'NONE',  ( -1.000000000000000000, -0.000000000000000000, -0.000000000000000000 ) ) ;
#6549 = ORIENTED_EDGE ( 'NONE', *, *, #34328, .F. ) ;
#6550 = CARTESIAN_POINT ( 'NONE',  ( -0.03662792686184423302, -0.04111994379180376746, 0.4792679903722390500 ) ) ;
#6551 = DIRECTION ( 'NONE',  ( 0.000000000000000000, 0.000000000000000000, -1.000000000000000000 ) ) ;
#6552 = DIRECTION ( 'NONE',  ( -0.4999551463232372317, 0.8660512985181134660, 0.000000000000000000 ) ) ;
#6553 = AXIS2_PLACEMENT_3D ( 'NONE', #37137, #701, #19593 ) ;
#6555 = VERTEX_POINT ( 'NONE', #9493 ) ;
#6554 = FACE_OUTER_BOUND ( 'NONE', #22465, .T. ) ;
#6556 = ORIENTED_EDGE ( 'NONE', *, *, #28608, .T. ) ;
#6557 = CARTESIAN_POINT ( 'NONE',  ( 0.1995338205807487553, -0.7602668576148212676, 0.3267161968192467403 ) ) ;
#6558 = EDGE_LOOP ( 'NONE', ( #9389, #18727, #7621 ) ) ;
#6559 = CIRCLE ( 'NONE', #20384, 0.009999999999999993269 ) ;
#6560 = CARTESIAN_POINT ( 'NONE',  ( 0.2985895772694463490, -1.656929904383750873, 0.5927621635699326097 ) ) ;
#6562 = CARTESIAN_POINT ( 'NONE',  ( 0.4264202721361134985, -1.467519734074643534, -0.5166151207188711680 ) ) ;
#6561 = CARTESIAN_POINT ( 'NONE',  ( 0.2085664583100847180, -0.9408741989701879804, 0.6570105467478477568 ) ) ;
#6563 = CARTESIAN_POINT ( 'NONE',  ( 0.3857322640002042169, -1.760817745270522039, -0.4634799128580170957 ) ) ;
#6564 = CARTESIAN_POINT ( 'NONE',  ( -0.2399999999999999079, -4.098813193844367042, -0.6491724279539748954 ) ) ;
#6565 = CARTESIAN_POINT ( 'NONE',  ( -0.1126900943574665054, -0.5191528599708419289, 0.3032895567580775609 ) ) ;
#6567 = EDGE_LOOP ( 'NONE', ( #32803, #39043, #32309, #2441 ) ) ;
#6566 = ORIENTED_EDGE ( 'NONE', *, *, #24850, .F. ) ;
#6568 = CARTESIAN_POINT ( 'NONE',  ( 0.4724132931814642444, -1.077943426954374395, -0.4216967736820900203 ) ) ;
#6569 = CARTESIAN_POINT ( 'NONE',  ( 0.1862143093560919282, -0.9153542374866575626, 0.1443021394692982906 ) ) ;
#6570 = CARTESIAN_POINT ( 'NONE',  ( 0.3558114376875948781, -1.251414176327350525, 0.5182417262812423209 ) ) ;
#6571 = CARTESIAN_POINT ( 'NONE',  ( 0.5698248817562774349, -1.454081016919124281, 0.7261892429133063320 ) ) ;
#6572 = CARTESIAN_POINT ( 'NONE',  ( 0.1882935783789653206, -0.8844134358759655479, 0.5622750411365140533 ) ) ;
#6573 = CARTESIAN_POINT ( 'NONE',  ( 0.2339608829160596815, -1.489014943295124294, 0.9134659781549987478 ) ) ;
#6574 = CARTESIAN_POINT ( 'NONE',  ( 0.1275022910136354160, -0.9890455054698116255, 0.9358088192774665082 ) ) ;
#6575 = CARTESIAN_POINT ( 'NONE',  ( 0.4042633028796379646, -1.711240744074478570, 0.4220515681607872605 ) ) ;
#6576 = CARTESIAN_POINT ( 'NONE',  ( -0.01548846960707524721, 0.000000000000000000, 0.000000000000000000 ) ) ;
#6577 = CARTESIAN_POINT ( 'NONE',  ( -0.2399999999999999079, -3.579933075828129141, -0.2145427270617869253 ) ) ;
#6578 = DIRECTION ( 'NONE',  ( 0.3468893892380794930, 0.7396492646830054030, 0.5767033179095832907 ) ) ;
#6579 = VECTOR ( 'NONE', #37421, 39.37007874015748143 ) ;
#6580 = CARTESIAN_POINT ( 'NONE',  ( 0.000000000000000000, 0.1428018198284763673, -0.2638325989215043466 ) ) ;
#6581 = CARTESIAN_POINT ( 'NONE',  ( 0.1587139193017044758, -1.140357826010188314, 1.006504499293092714 ) ) ;
#6582 = CARTESIAN_POINT ( 'NONE',  ( 0.09896627915743715087, -1.366272486005550180, 0.6737215609984372744 ) ) ;
#6583 = APPROVAL_DATE_TIME ( #25742, #19210 ) ;
#6584 = CARTESIAN_POINT ( 'NONE',  ( -0.04308558661660367994, 0.4494156853470179791, 0.2058346122081028406 ) ) ;
#6585 = CARTESIAN_POINT ( 'NONE',  ( 0.7004187681061331272, -1.489996274278563071, 0.4963418890236395709 ) ) ;
#6586 = EDGE_CURVE ( 'NONE', #27450, #24506, #7032, .T. ) ;
#6587 = ORIENTED_EDGE ( 'NONE', *, *, #15550, .F. ) ;
#6588 = CARTESIAN_POINT ( 'NONE',  ( 0.1895845073671591496, -0.5861495762347013194, 0.2988846075130171531 ) ) ;
#6589 = EDGE_LOOP ( 'NONE', ( #29954, #12841, #27071, #12966 ) ) ;
#6590 = FACE_BOUND ( 'NONE', #21583, .T. ) ;
#6591 = APPLIED_PERSON_AND_ORGANIZATION_ASSIGNMENT ( #7111, #32976, ( #445 ) ) ;
#6592 = CARTESIAN_POINT ( 'NONE',  ( 0.2367319421433582705, -1.498621928344235910, 0.9091324809083795033 ) ) ;
#6593 = CARTESIAN_POINT ( 'NONE',  ( 0.5007062318473965989, -1.350239968012811209, 0.8060270520129010352 ) ) ;
#6595 = ORIENTED_EDGE ( 'NONE', *, *, #27787, .F. ) ;
#6594 = CARTESIAN_POINT ( 'NONE',  ( 0.5024525556466100662, -1.651954489456844533, -0.4338784509423143088 ) ) ;
#6596 = B_SPLINE_CURVE_WITH_KNOTS ( 'NONE', 3,
 ( #19845, #13664, #4407, #26229 ),
 .UNSPECIFIED., .F., .F.,
 ( 4, 4 ),
 ( 3.127317220692750759E-18, 0.0003263726155883022958 ),
 .UNSPECIFIED. ) ;
#6598 = VERTEX_POINT ( 'NONE', #18146 ) ;
#6597 = EDGE_LOOP ( 'NONE', ( #12900, #2488, #13690, #27536, #28097, #11735, #13854, #29456, #17517, #4447, #27727, #12541, #26582, #3434 ) ) ;
#6599 = CARTESIAN_POINT ( 'NONE',  ( 0.5122377810313424318, -1.683552081238520293, -0.5849915292415723833 ) ) ;
#6600 = ORIENTED_EDGE ( 'NONE', *, *, #16291, .T. ) ;
#6601 = CARTESIAN_POINT ( 'NONE',  ( 0.6129759397991038083, -1.613544640311175948, -0.5428363245105037871 ) ) ;
#6602 = CALENDAR_DATE ( 2026, 13, 10 ) ;
#6603 = CIRCLE ( 'NONE', #11872, 0.01499999999999995434 ) ;
#6604 = CARTESIAN_POINT ( 'NONE',  ( 0.6129335297421601991, -1.616808798314981921, 0.5182417262812423209 ) ) ;
#6605 = ORIENTED_EDGE ( 'NONE', *, *, #18805, .T. ) ;
#6606 = CARTESIAN_POINT ( 'NONE',  ( 0.1266283464120225577, -0.7967538953625531439, 0.4596558820756620478 ) ) ;
#6607 = CARTESIAN_POINT ( 'NONE',  ( 0.08990536851188075940, -0.5646295468556798980, 0.1370866209488758869 ) ) ;
#6608 = TOROIDAL_SURFACE ( 'NONE', #15174, 0.9237847906030132172, 0.01499999999999999944 ) ;
#6609 = CARTESIAN_POINT ( 'NONE',  ( 0.1056960294869904032, -0.5719007525085089139, 0.2557726251434392362 ) ) ;
#6610 = CARTESIAN_POINT ( 'NONE',  ( 0.6248336632338993279, -1.524278534507916172, -0.6328788536102397666 ) ) ;
#6611 = CARTESIAN_POINT ( 'NONE',  ( -0.1688425296110704910, 0.4915895952456253437, 0.1316117873487812617 ) ) ;
#6612 = AXIS2_PLACEMENT_3D ( 'NONE', #39154, #26406, #17731 ) ;
#6613 = ORIENTED_EDGE ( 'NONE', *, *, #30356, .T. ) ;
#6614 = AXIS2_PLACEMENT_3D ( 'NONE', #37148, #15551, #21326 ) ;
#6615 = CARTESIAN_POINT ( 'NONE',  ( 0.4032474725367772295, -1.711818401373710108, 0.6107726817123948493 ) ) ;
#6616 = CARTESIAN_POINT ( 'NONE',  ( 0.6494194904526725542, -1.505054641034485163, 0.7731478513741499858 ) ) ;
#6617 = EDGE_CURVE ( 'NONE', #36330, #37905, #21856, .T. ) ;
#6618 = DIRECTION ( 'NONE',  ( 0.8660512985181131329, 0.4999551463232377313, 0.000000000000000000 ) ) ;
#6619 = ADVANCED_FACE ( 'NONE', ( #6199 ), #4543, .F. ) ;
#6620 = CARTESIAN_POINT ( 'NONE',  ( 0.6085670229761270811, -1.478915227102408414, 0.5633428062726970609 ) ) ;
#6621 = LINE ( 'NONE', #31353, #8116 ) ;
#6622 =( NAMED_UNIT ( * ) PLANE_ANGLE_UNIT ( ) SI_UNIT ( $, .RADIAN. ) );
#6623 = EDGE_CURVE ( 'NONE', #23460, #35126, #35288, .T. ) ;
#6624 = CARTESIAN_POINT ( 'NONE',  ( -0.2600000000000008415, 0.5182417262804733804, 0.08500000000000006162 ) ) ;
#6625 = EDGE_CURVE ( 'NONE', #34849, #17560, #29018, .T. ) ;
#6626 = CARTESIAN_POINT ( 'NONE',  ( 2.077341244938675305E-16, 0.2900000000000004796, 0.04249999999999943406 ) ) ;
#6627 = EDGE_CURVE ( 'NONE', #32971, #38598, #6454, .T. ) ;
#6628 = CARTESIAN_POINT ( 'NONE',  ( 0.08075236803977006717, -1.368778601871594836, 0.5682417262808778791 ) ) ;
#6629 = B_SPLINE_CURVE_WITH_KNOTS ( 'NONE', 3,
 ( #31788, #6471, #34461, #37531 ),
 .UNSPECIFIED., .F., .F.,
 ( 4, 4 ),
 ( 0.0009402988323797356694, 0.001215464345533929895 ),
 .UNSPECIFIED. ) ;
#6630 = CARTESIAN_POINT ( 'NONE',  ( 0.5117280326951013647, -1.115088012504228621, 0.5923667439031021775 ) ) ;
#6631 = APPROVAL_STATUS ( 'not_yet_approved' ) ;
#6632 = CARTESIAN_POINT ( 'NONE',  ( -0.09908070219615711105, -0.09959325338431362917, 0.09550516381870158278 ) ) ;
#6633 = AXIS2_PLACEMENT_3D ( 'NONE', #38601, #1984, #14507 ) ;
#6634 = CARTESIAN_POINT ( 'NONE',  ( 0.4660507111952964521, -1.558206335128884845, 0.5363334130509328501 ) ) ;
#6635 = CIRCLE ( 'NONE', #8607, 0.5399999999999999245 ) ;
#6636 = CARTESIAN_POINT ( 'NONE',  ( -0.05252359774140137605, 0.009047791085684511042, 0.4689872004378276005 ) ) ;
#6637 = AXIS2_PLACEMENT_3D ( 'NONE', #35667, #19637, #4576 ) ;
#6638 = EDGE_CURVE ( 'NONE', #16250, #38006, #31706, .T. ) ;
#6639 = ORIENTED_EDGE ( 'NONE', *, *, #27778, .T. ) ;
#6640 = CARTESIAN_POINT ( 'NONE',  ( 0.4475777147736147987, -1.570831683793988187, 0.5814946475837428075 ) ) ;
#6641 = AXIS2_PLACEMENT_3D ( 'NONE', #11314, #10709, #14387 ) ;
#6642 = DIRECTION ( 'NONE',  ( -1.000000000000000000, -7.857794173099924470E-32, -8.628166150854818811E-32 ) ) ;
#6643 = CIRCLE ( 'NONE', #24416, 0.5614999999999926716 ) ;
#6644 = CARTESIAN_POINT ( 'NONE',  ( 0.08839720336850717675, -0.6253492388939145830, 0.03921914501878817627 ) ) ;
#6645 = ORIENTED_EDGE ( 'NONE', *, *, #24745, .F. ) ;
#6646 = CARTESIAN_POINT ( 'NONE',  ( 0.4090604450045443596, -1.131420581850358653, 0.3667417262808778666 ) ) ;
#6647 = CARTESIAN_POINT ( 'NONE',  ( 0.04292188072724165138, -1.133578733677452099, 0.7617704846099633276 ) ) ;
#6649 = ORIENTED_EDGE ( 'NONE', *, *, #1971, .F. ) ;
#6648 = EDGE_LOOP ( 'NONE', ( #34442, #32987, #10522, #23931 ) ) ;
#6650 = FACE_OUTER_BOUND ( 'NONE', #2673, .T. ) ;
#6651 = CARTESIAN_POINT ( 'NONE',  ( 0.1536596445529307131, -1.277574755431481579, 0.4245438548657216038 ) ) ;
#6652 = CARTESIAN_POINT ( 'NONE',  ( 0.2190497394446654089, -1.621418830003412692, -0.3569805845145136436 ) ) ;
#6654 = CARTESIAN_POINT ( 'NONE',  ( -0.2746410161513779258, -2.595429044015121534, -0.5484989581857646623 ) ) ;
#6653 = CARTESIAN_POINT ( 'NONE',  ( -0.2399999999999999079, -4.292451985131092940, -0.8428112192407016812 ) ) ;
#6655 = CARTESIAN_POINT ( 'NONE',  ( -2.112273405726188513E-14, -1.835409001655643690, -0.3543101909453316156 ) ) ;
#6656 = EDGE_LOOP ( 'NONE', ( #10429, #1146, #18255, #40302 ) ) ;
#6657 = CARTESIAN_POINT ( 'NONE',  ( -0.01895494625228198032, 0.2428766181966292015, -0.4598657641708846500 ) ) ;
#6658 = ORIENTED_EDGE ( 'NONE', *, *, #15821, .F. ) ;
#6659 = ORIENTED_EDGE ( 'NONE', *, *, #15454, .T. ) ;
#6660 = EDGE_CURVE ( 'NONE', #23858, #24493, #23171, .T. ) ;
#6661 = CARTESIAN_POINT ( 'NONE',  ( 0.1537277655112500585, -0.7413063141131301936, 0.5573565750015010423 ) ) ;
#6662 = ORIENTED_EDGE ( 'NONE', *, *, #12452, .F. ) ;
#6663 = EDGE_CURVE ( 'NONE', #22491, #24257, #5059, .T. ) ;
#6664 = EDGE_LOOP ( 'NONE', ( #9055, #3697, #9148, #26214, #9021, #23750 ) ) ;
#6665 = DIRECTION ( 'NONE',  ( 1.000000000000000000, 0.000000000000000000, 0.000000000000000000 ) ) ;
#6666 = CARTESIAN_POINT ( 'NONE',  ( 0.07297943341930077099, -0.5464194006479311527, 0.1919652695815136645 ) ) ;
#6668 = CARTESIAN_POINT ( 'NONE',  ( -0.1068374249684608812, -0.4867512985521031954, 0.3606502370888775011 ) ) ;
#6667 = CARTESIAN_POINT ( 'NONE',  ( -0.1443375672974067936, 0.05141091571461216952, 0.000000000000000000 ) ) ;
#6669 = CARTESIAN_POINT ( 'NONE',  ( -0.08000000000000000167, -1.546789565643408304, -0.06332195561662114225 ) ) ;
#6670 = CARTESIAN_POINT ( 'NONE',  ( 0.2020865016433360528, -0.9231306475095830688, 0.3258051546269021825 ) ) ;
#6671 = CARTESIAN_POINT ( 'NONE',  ( 0.1996203293408511381, -2.065051801937105136, -0.7178016293569640105 ) ) ;
#6672 = CARTESIAN_POINT ( 'NONE',  ( 0.1897112079047655053, -0.5340520988484990239, 0.1385946963835808510 ) ) ;
#6673 = CARTESIAN_POINT ( 'NONE',  ( 0.2166550137285412070, -0.8304811269046187272, 0.6463872802090209202 ) ) ;
#6674 = CARTESIAN_POINT ( 'NONE',  ( -0.03474824846560518876, 0.3591470389155430598, -0.3712557345097572403 ) ) ;
#6675 = EDGE_CURVE ( 'NONE', #24795, #7643, #20858, .T. ) ;
#6676 = AXIS2_PLACEMENT_3D ( 'NONE', #18944, #31479, #3287 ) ;
#6677 = AXIS2_PLACEMENT_3D ( 'NONE', #7276, #26439, #29716 ) ;
#6678 = CARTESIAN_POINT ( 'NONE',  ( -0.04574984450154874482, -0.4390502118250590446, -0.2110542068117175485 ) ) ;
#6679 = VECTOR ( 'NONE', #19169, 39.37007874015748854 ) ;
#6680 = ADVANCED_FACE ( 'NONE', ( #19579 ), #10340, .T. ) ;
#6681 = CARTESIAN_POINT ( 'NONE',  ( 0.08296493955445416457, -0.6173275490175130775, 0.3808511444712925353 ) ) ;
#6682 = FACE_OUTER_BOUND ( 'NONE', #34141, .T. ) ;
#6683 = EDGE_CURVE ( 'NONE', #20307, #8639, #15593, .T. ) ;
#6684 = CARTESIAN_POINT ( 'NONE',  ( 0.4605766076693431632, -1.054687064863744750, 0.7953974510635947182 ) ) ;
#6685 = DIRECTION ( 'NONE',  ( 0.8057988841560899118, 0.4797014836779449065, -0.3472385993088597522 ) ) ;
#6686 = CARTESIAN_POINT ( 'NONE',  ( 0.05596281731547365912, -1.307106975853646658, 0.6186298968216493721 ) ) ;
#6688 = AXIS2_PLACEMENT_3D ( 'NONE', #6062, #19451, #9573 ) ;
#6687 = CARTESIAN_POINT ( 'NONE',  ( 0.02872242845530422264, 0.4768947642620191552, -0.2371557650701889286 ) ) ;
#6689 = CARTESIAN_POINT ( 'NONE',  ( 0.1914801911188975247, -0.6027644909819236396, 0.3101999008291455029 ) ) ;
#6690 = CARTESIAN_POINT ( 'NONE',  ( 0.1007139418999222075, -0.8573875874287576471, 0.4354917424624366040 ) ) ;
#6691 = CARTESIAN_POINT ( 'NONE',  ( -0.01548846960707524721, 0.000000000000000000, 0.000000000000000000 ) ) ;
#6692 = CARTESIAN_POINT ( 'NONE',  ( 0.6627797186572951249, -1.546517967009319205, 0.4296449949859427742 ) ) ;
#6693 = EDGE_CURVE ( 'NONE', #31055, #33631, #9009, .T. ) ;
#6694 = ORIENTED_EDGE ( 'NONE', *, *, #14506, .F. ) ;
#6695 = DIRECTION ( 'NONE',  ( 0.4999551463232372317, -0.8660512985181135770, 0.000000000000000000 ) ) ;
#6696 = CARTESIAN_POINT ( 'NONE',  ( 0.1454652487279074757, -0.7477097220224196983, 0.5302102881989955163 ) ) ;
#6697 = DIRECTION ( 'NONE',  ( 0.8660512985181135770, 0.4999551463232370652, 0.000000000000000000 ) ) ;
#6698 = CARTESIAN_POINT ( 'NONE',  ( 0.1016010970546381426, -1.316932408029475532, 0.4414108731151945575 ) ) ;
#6699 = ADVANCED_FACE ( 'NONE', ( #13177 ), #38273, .T. ) ;
#6700 = EDGE_LOOP ( 'NONE', ( #17042, #6605, #14826, #1637, #26228, #39614, #12098, #5502 ) ) ;
#6701 = CARTESIAN_POINT ( 'NONE',  ( -0.03662792686184342811, -0.2484399233013400432, -0.4119056456069905003 ) ) ;
#6702 = VECTOR ( 'NONE', #31083, 39.37007874015748143 ) ;
#6703 =( BOUNDED_SURFACE ( )  B_SPLINE_SURFACE ( 3, 2, ( 
 ( #8152, #38803, #39235 ),
 ( #13716, #32650, #4455 ),
 ( #23427, #1815, #35945 ),
 ( #11057, #7751, #20315 ),
 ( #32836, #4643, #17217 ),
 ( #23615, #29762, #7939 ),
 ( #20514, #4852, #39422 ),
 ( #11243, #23815, #36335 ) ),
 .UNSPECIFIED., .F., .F., .T. ) 
 B_SPLINE_SURFACE_WITH_KNOTS ( ( 4, 2, 2, 4 ),
 ( 3, 3 ),
 ( 0.000000000000000000, 0.0009689511937531078639, 0.001453426790629661850, 0.001937902387506215728 ),
 ( 0.000000000000000000, 1.000000000000000000 ),
 .UNSPECIFIED. ) 
 GEOMETRIC_REPRESENTATION_ITEM ( )  RATIONAL_B_SPLINE_SURFACE ( (
 ( 1.000000000000000000, 0.7071067811865507924, 1.000000000000000000),
 ( 1.000000000000000000, 0.7661883050553089936, 1.000000000000000000),
 ( 1.000000000000000000, 0.8090289802883275927, 1.000000000000000000),
 ( 1.000000000000000000, 0.8549856046166490753, 1.000000000000000000),
 ( 1.000000000000000000, 0.8668418550465033512, 1.000000000000000000),
 ( 1.000000000000000000, 0.8822522463525879211, 1.000000000000000000),
 ( 1.000000000000000000, 0.8856360263997571369, 1.000000000000000000),
 ( 1.000000000000000000, 0.8847557669246132184, 1.000000000000000000) ) ) 
 REPRESENTATION_ITEM ( '' )  SURFACE ( )  );
#6704 = AXIS2_PLACEMENT_3D ( 'NONE', #13980, #7188, #7609 ) ;
#6705 = CARTESIAN_POINT ( 'NONE',  ( 0.1802350563441833808, -0.5022327775090948965, 0.1477559389858786043 ) ) ;
#6706 = CARTESIAN_POINT ( 'NONE',  ( 0.4516520847856119181, -1.680408577508558210, 0.4354989228371364818 ) ) ;
#6707 = DIRECTION ( 'NONE',  ( 1.000000000000000000, 0.000000000000000000, 0.000000000000000000 ) ) ;
#6708 = CARTESIAN_POINT ( 'NONE',  ( 0.4751785028721121629, -1.252254961389827503, 0.6770357329939598046 ) ) ;
#6710 = CARTESIAN_POINT ( 'NONE',  ( 0.3197311927886214988, -1.759354868725874432, 0.4922608866671225880 ) ) ;
#6709 = CARTESIAN_POINT ( 'NONE',  ( -0.05464101615137785528, -2.631664041040912227, -0.5119035495255163104 ) ) ;
#6711 = CARTESIAN_POINT ( 'NONE',  ( 0.3924682913416943086, -1.027586590250060272, 0.6289202682814357681 ) ) ;
#6712 = ORIENTED_EDGE ( 'NONE', *, *, #37142, .T. ) ;
#6713 = APPROVAL_STATUS ( 'not_yet_approved' ) ;
#6714 = CARTESIAN_POINT ( 'NONE',  ( 0.08560287521161533131, -1.284824326520781490, 0.7328930470927262908 ) ) ;
#6715 = ORIENTED_EDGE ( 'NONE', *, *, #766, .T. ) ;
#6716 = ORIENTED_EDGE ( 'NONE', *, *, #8003, .F. ) ;
#6717 = CARTESIAN_POINT ( 'NONE',  ( 0.3854321820439991497, -1.605669856351402691, 0.5768392551633937382 ) ) ;
#6719 = CARTESIAN_POINT ( 'NONE',  ( 0.1734973056165642902, -1.209394307038482497, -0.5155029497116575543 ) ) ;
#6718 = CARTESIAN_POINT ( 'NONE',  ( 0.08509577109033511499, -0.8106501036565759710, 0.1481698590609797916 ) ) ;
#6720 = CARTESIAN_POINT ( 'NONE',  ( 0.06739064528196411774, -0.6397219464422030377, 0.005700442802499041187 ) ) ;
#6721 = ORIENTED_EDGE ( 'NONE', *, *, #30625, .F. ) ;
#6722 = ORIENTED_EDGE ( 'NONE', *, *, #12462, .T. ) ;
#6723 = EDGE_LOOP ( 'NONE', ( #35718, #29968, #27829, #22475, #6326, #16896, #12801 ) ) ;
#6724 = CARTESIAN_POINT ( 'NONE',  ( 0.3245308759113119113, -1.295391163961464365, 0.5682442948123348492 ) ) ;
#6725 = CARTESIAN_POINT ( 'NONE',  ( 0.5669662277262230710, -1.503240378328975613, 0.5737068391451652927 ) ) ;
#6726 = ORIENTED_EDGE ( 'NONE', *, *, #14539, .T. ) ;
#6727 = FACE_OUTER_BOUND ( 'NONE', #18780, .T. ) ;
#6728 = CARTESIAN_POINT ( 'NONE',  ( 0.4974456442574050619, -1.184401136727558868, 0.4224083929475309640 ) ) ;
#6729 = DIRECTION ( 'NONE',  ( 5.546678239835219551E-32, 0.9849933812516251663, -0.1725921171157328571 ) ) ;
#6730 = CARTESIAN_POINT ( 'NONE',  ( 0.4159916692016358830, -1.069406866067976081, -0.5155029497116575543 ) ) ;
#6731 = CARTESIAN_POINT ( 'NONE',  ( 0.1840771369943047242, -0.8547796389794056759, 0.1590146724173516768 ) ) ;
#6732 = AXIS2_PLACEMENT_3D ( 'NONE', #40127, #8654, #20626 ) ;
#6733 = EDGE_CURVE ( 'NONE', #2349, #38034, #37257, .T. ) ;
#6734 = CARTESIAN_POINT ( 'NONE',  ( -0.2746410161513776482, -3.941790907013290823, -0.2762780017083287243 ) ) ;
#6735 = CARTESIAN_POINT ( 'NONE',  ( 0.3827795040295842166, -1.762256314311558603, -0.5556587900919752743 ) ) ;
#6736 = CARTESIAN_POINT ( 'NONE',  ( 0.6551261771431925451, -1.361944467462807395, 0.8444247977208539924 ) ) ;
#6737 = AXIS2_PLACEMENT_3D ( 'NONE', #22957, #17927, #7280 ) ;
#6738 = CARTESIAN_POINT ( 'NONE',  ( 0.3967399397739009292, -2.017252274505498821, -0.7078152146948345491 ) ) ;
#6739 = CARTESIAN_POINT ( 'NONE',  ( 0.4138729472876766513, -1.128955312352843965, 0.5470489658417444501 ) ) ;
#6740 = DIRECTION ( 'NONE',  ( 0.000000000000000000, 0.8090169943749455639, -0.5877852522924756906 ) ) ;
#6741 = COORDINATED_UNIVERSAL_TIME_OFFSET ( 0, 0, .AHEAD. ) ;
#6742 = AXIS2_PLACEMENT_3D ( 'NONE', #1440, #13954, #14360 ) ;
#6743 = LINE ( 'NONE', #35149, #3485 ) ;
#6744 = DIRECTION ( 'NONE',  ( 0.3468893892380652821, -0.3199132558032009022, -0.8816593788960893630 ) ) ;
#6745 = CARTESIAN_POINT ( 'NONE',  ( 0.4580278197616229896, -1.241383277718457911, 0.6057417262809816627 ) ) ;
#6746 = CARTESIAN_POINT ( 'NONE',  ( 0.1499999999999989120, -0.3880410510314797334, -0.3755318131854984420 ) ) ;
#6747 = CARTESIAN_POINT ( 'NONE',  ( 0.01179864804857342665, -0.6562760587974182380, 0.4561945812754703011 ) ) ;
#6748 = CARTESIAN_POINT ( 'NONE',  ( 0.0004433609336470854898, -0.4385931729850870431, 0.1292661587538940227 ) ) ;
#6749 = EDGE_CURVE ( 'NONE', #3992, #20653, #6559, .T. ) ;
#6750 = LINE ( 'NONE', #21803, #23887 ) ;
#6751 = DIRECTION ( 'NONE',  ( -1.000000000000000000, 0.000000000000000000, -1.138269997360103659E-15 ) ) ;
#6752 = EDGE_CURVE ( 'NONE', #9135, #30000, #11352, .T. ) ;
#6753 = ORIENTED_EDGE ( 'NONE', *, *, #14535, .F. ) ;
#6754 = ORIENTED_EDGE ( 'NONE', *, *, #1477, .F. ) ;
#6755 = DIRECTION ( 'NONE',  ( 0.000000000000000000, 0.000000000000000000, 1.000000000000000000 ) ) ;
#6756 = ORIENTED_EDGE ( 'NONE', *, *, #15580, .T. ) ;
#6757 = CARTESIAN_POINT ( 'NONE',  ( 0.3606884409928574620, -1.747583433209421333, 0.4408685289531725227 ) ) ;
#6758 = CYLINDRICAL_SURFACE ( 'NONE', #36400, 0.01000000000000005398 ) ;
#6759 = AXIS2_PLACEMENT_3D ( 'NONE', #10046, #7139, #22828 ) ;
#6760 = CARTESIAN_POINT ( 'NONE',  ( 0.06682908180107070828, -0.6872203660146791737, -0.001923513761143209400 ) ) ;
#6762 = ORIENTED_EDGE ( 'NONE', *, *, #18805, .F. ) ;
#6761 = LINE ( 'NONE', #19544, #20628 ) ;
#6763 = VERTEX_POINT ( 'NONE', #28633 ) ;
#6764 = DIRECTION ( 'NONE',  ( -1.188678714063518227E-15, 1.000000000000000000, 3.263080277421930985E-16 ) ) ;
#6765 = AXIS2_PLACEMENT_3D ( 'NONE', #38428, #10448, #636 ) ;
#6766 = VERTEX_POINT ( 'NONE', #9893 ) ;
#6767 = CIRCLE ( 'NONE', #21892, 0.1999999999999994837 ) ;
#6768 = CARTESIAN_POINT ( 'NONE',  ( 0.2970029333241409608, -1.656601473353111365, 0.5710316030164380718 ) ) ;
#6770 = CARTESIAN_POINT ( 'NONE',  ( 0.2059273467974226113, -1.283046334493782803, -0.3194715457588298557 ) ) ;
#6769 = CARTESIAN_POINT ( 'NONE',  ( 0.6035974019387861933, -1.594473330473194839, 0.4258042085085226858 ) ) ;
#6771 = CARTESIAN_POINT ( 'NONE',  ( 0.3099480278792562382, -1.763253171224924420, 0.5409204437200131332 ) ) ;
#6772 = CARTESIAN_POINT ( 'NONE',  ( 0.01176869885886682073, -0.6532089530866552751, -0.1114877525985862178 ) ) ;
#6773 = CARTESIAN_POINT ( 'NONE',  ( 0.009624474380123570691, -1.740256400171903861, -0.3645574449919975479 ) ) ;
#6775 = ORIENTED_EDGE ( 'NONE', *, *, #26995, .F. ) ;
#6774 = ORIENTED_EDGE ( 'NONE', *, *, #1200, .T. ) ;
#6776 = DIRECTION ( 'NONE',  ( -6.162975822039154730E-33, 0.000000000000000000, -1.000000000000000000 ) ) ;
#6777 = CARTESIAN_POINT ( 'NONE',  ( 0.1109210135120192453, -0.9286415089466554251, 0.1524864793821099351 ) ) ;
#6778 = CIRCLE ( 'NONE', #2854, 0.4488493849861018292 ) ;
#6779 = CARTESIAN_POINT ( 'NONE',  ( -0.03868649100028198617, -0.03360400204099364685, -0.4753701585314240030 ) ) ;
#6780 = DIRECTION ( 'NONE',  ( -0.4999999999999972800, -0.8563665354314757838, -0.1289820025937487569 ) ) ;
#6781 = AXIS2_PLACEMENT_3D ( 'NONE', #33407, #2553, #30732 ) ;
#6782 = DIRECTION ( 'NONE',  ( 7.114187483500656449E-15, 0.8834504764630435325, -0.4685245517976845409 ) ) ;
#6783 = CYLINDRICAL_SURFACE ( 'NONE', #5367, 0.01500000000000001853 ) ;
#6784 = EDGE_CURVE ( 'NONE', #37319, #35448, #32478, .T. ) ;
#6785 = CARTESIAN_POINT ( 'NONE',  ( 0.1291001614701467459, -0.9254250030040105379, 0.1457122326985881844 ) ) ;
#6786 = DIRECTION ( 'NONE',  ( -8.881784197001246407E-16, 2.361472542561082612E-16, -1.000000000000000000 ) ) ;
#6787 = CARTESIAN_POINT ( 'NONE',  ( 0.1999999999999989564, -0.05999999999999990757, -5.463695987328526437E-16 ) ) ;
#6788 = DIRECTION ( 'NONE',  ( 0.000000000000000000, -0.8090169943749413450, 0.5877852522924816858 ) ) ;
#6789 = CARTESIAN_POINT ( 'NONE',  ( 0.3582910526024343789, -1.180702780429254917, 7.680932115186284060E-13 ) ) ;
#6790 = CIRCLE ( 'NONE', #33078, 0.1999999999999999833 ) ;
#6791 = CARTESIAN_POINT ( 'NONE',  ( -0.0003003500745766487395, -0.9376955769830692677, 0.2168050107958245654 ) ) ;
#6792 = CARTESIAN_POINT ( 'NONE',  ( 0.2750825180155820338, -1.558163865710181728, 0.9909808761736236260 ) ) ;
#6793 = CARTESIAN_POINT ( 'NONE',  ( 0.1778100121041887027, -1.872358142960663496, -0.6552623532412349405 ) ) ;
#6794 = APPROVAL_DATE_TIME ( #287, #8891 ) ;
#6795 = AXIS2_PLACEMENT_3D ( 'NONE', #34597, #21651, #31105 ) ;
#6796 = AXIS2_PLACEMENT_3D ( 'NONE', #21607, #39485, #11528 ) ;
#6797 = CARTESIAN_POINT ( 'NONE',  ( 0.3711309917658967561, -1.727276130344147509, -0.6834503960384243904 ) ) ;
#6798 = CARTESIAN_POINT ( 'NONE',  ( 0.3269961855704987541, -1.756646017944762939, 0.5657241070551874973 ) ) ;
#6799 = DIRECTION ( 'NONE',  ( -6.162975822039154730E-33, 0.000000000000000000, -1.000000000000000000 ) ) ;
#6800 = VECTOR ( 'NONE', #3027, 39.37007874015748854 ) ;
#6801 = AXIS2_PLACEMENT_3D ( 'NONE', #20224, #10963, #23523 ) ;
#6802 = VERTEX_POINT ( 'NONE', #14199 ) ;
#6803 = CARTESIAN_POINT ( 'NONE',  ( 0.1844620385557431963, -0.5656468219106428608, 0.2771782185203255922 ) ) ;
#6804 = ORIENTED_EDGE ( 'NONE', *, *, #37694, .T. ) ;
#6805 = CARTESIAN_POINT ( 'NONE',  ( 0.4463968940846189670, -1.144227781936946409, -0.6446835755021989023 ) ) ;
#6806 = CARTESIAN_POINT ( 'NONE',  ( 0.2572930768252133515, -1.677938012603978013, 0.5362869298745072122 ) ) ;
#6807 = CARTESIAN_POINT ( 'NONE',  ( 0.2478791248605221043, -0.8877234785324099597, 0.6911795992708721359 ) ) ;
#6808 = EDGE_CURVE ( 'NONE', #34195, #3414, #29566, .T. ) ;
#6810 = ORIENTED_EDGE ( 'NONE', *, *, #20367, .T. ) ;
#6809 = CARTESIAN_POINT ( 'NONE',  ( 0.4942350278003149744, -1.646331289742994031, -0.4039250241487104542 ) ) ;
#6812 = ORIENTED_EDGE ( 'NONE', *, *, #3599, .T. ) ;
#6811 = ORIENTED_EDGE ( 'NONE', *, *, #11100, .F. ) ;
#6813 = CARTESIAN_POINT ( 'NONE',  ( -0.01548846960707531660, -0.2372406987223689145, -0.4850946823762606330 ) ) ;
#6814 = ORIENTED_EDGE ( 'NONE', *, *, #30517, .F. ) ;
#6815 = ORIENTED_EDGE ( 'NONE', *, *, #3684, .T. ) ;
#6816 = CARTESIAN_POINT ( 'NONE',  ( 0.3665972292190579074, -1.767090988255677342, -0.5848990675856741150 ) ) ;
#6817 = CARTESIAN_POINT ( 'NONE',  ( -2.115421433687637455E-14, -2.107936428766274073, -0.7005084057759867200 ) ) ;
#6818 = CALENDAR_DATE ( 2026, 13, 10 ) ;
#6819 = AXIS2_PLACEMENT_3D ( 'NONE', #34952, #29191, #19542 ) ;
#6820 = DIRECTION ( 'NONE',  ( 0.8660512985181125778, 0.4999551463232387860, 0.000000000000000000 ) ) ;
#6821 = ORIENTED_EDGE ( 'NONE', *, *, #5942, .T. ) ;
#6822 = CARTESIAN_POINT ( 'NONE',  ( 0.08658218366773377805, -0.7469030435693181369, 0.1915370112333746877 ) ) ;
#6823 = CARTESIAN_POINT ( 'NONE',  ( 0.08990617429856566367, -0.5646418133096463565, 0.1474873524130712044 ) ) ;
#6824 = CIRCLE ( 'NONE', #31802, 0.05000000000000000971 ) ;
#6825 = CARTESIAN_POINT ( 'NONE',  ( 0.4848907914328412505, -1.427831231083330765, 0.7974248085317546808 ) ) ;
#6826 = CARTESIAN_POINT ( 'NONE',  ( 0.6505092258671375527, -1.603730573490085964, -0.4546931408925402041 ) ) ;
#6827 = DIRECTION ( 'NONE',  ( 0.000000000000000000, 1.951319995474460317E-15, -1.000000000000000000 ) ) ;
#6828 = CARTESIAN_POINT ( 'NONE',  ( 0.6537467011358751856, -1.544991604632938609, 0.4236745214088577516 ) ) ;
#6829 = CARTESIAN_POINT ( 'NONE',  ( -0.2900000000000002576, 0.5182417262804744906, 0.3599999999999993761 ) ) ;
#6830 = CARTESIAN_POINT ( 'NONE',  ( 0.6994016379560119567, -1.437929643118011969, 0.6007912156904529066 ) ) ;
#6831 = CIRCLE ( 'NONE', #10787, 0.04500000000000033834 ) ;
#6832 = DIRECTION ( 'NONE',  ( -6.162975822039154046E-33, 0.000000000000000000, -1.000000000000000000 ) ) ;
#6833 = CARTESIAN_POINT ( 'NONE',  ( 0.1412211329182320174, -0.6053832490378043829, 0.3245192810377299231 ) ) ;
#6834 = AXIS2_PLACEMENT_3D ( 'NONE', #3956, #28862, #722 ) ;
#6835 = CARTESIAN_POINT ( 'NONE',  ( -0.002294379339023699775, -0.8554970241181312218, 0.1489098701495673027 ) ) ;
#6836 = DIRECTION ( 'NONE',  ( 7.771561172376107616E-16, -7.170354002788761615E-17, 1.000000000000000000 ) ) ;
#6837 = CARTESIAN_POINT ( 'NONE',  ( 0.4726289841176697371, -1.127529792599587299, -0.3806505246460042957 ) ) ;
#6838 = CARTESIAN_POINT ( 'NONE',  ( 0.1499999999999994948, 0.4730347584886787082, 0.2341461249029790914 ) ) ;
#6839 = CARTESIAN_POINT ( 'NONE',  ( 0.3465599992496842807, -0.9476710551646405634, 0.6409924101657002993 ) ) ;
#6840 = CALENDAR_DATE ( 2026, 13, 10 ) ;
#6841 = DIRECTION ( 'NONE',  ( 0.007367783058131798131, 0.4999457213560383195, -0.8660253988599866393 ) ) ;
#6842 = CIRCLE ( 'NONE', #22660, 0.01000000000000002970 ) ;
#6843 = AXIS2_PLACEMENT_3D ( 'NONE', #5677, #18231, #27905 ) ;
#6844 = CARTESIAN_POINT ( 'NONE',  ( 0.3793181961223202059, -1.724015678557583309, 0.4221277619539304804 ) ) ;
#6845 = CARTESIAN_POINT ( 'NONE',  ( -0.03171893264487783692, 0.07587196131163785606, 0.5190999561769922277 ) ) ;
#6846 = CIRCLE ( 'NONE', #36438, 0.08000000000000000167 ) ;
#6847 = AXIS2_PLACEMENT_3D ( 'NONE', #34240, #5440, #14925 ) ;
#6848 = ORIENTED_EDGE ( 'NONE', *, *, #3020, .T. ) ;
#6849 = DIRECTION ( 'NONE',  ( -1.000000000000000000, 0.000000000000000000, 0.000000000000000000 ) ) ;
#6850 = APPROVAL_PERSON_ORGANIZATION ( #18297, #15957, #37218 ) ;
#6851 = CARTESIAN_POINT ( 'NONE',  ( 0.002367394983758686153, -0.5282119844061595737, 0.1431176680404078472 ) ) ;
#6852 = CARTESIAN_POINT ( 'NONE',  ( 0.08625494239356501502, -0.7682695115869180302, 0.05259860062006292691 ) ) ;
#6853 = ORIENTED_EDGE ( 'NONE', *, *, #14451, .F. ) ;
#6854 = CARTESIAN_POINT ( 'NONE',  ( 0.1436225252650951412, -1.283668529478381393, 0.4687417262808780127 ) ) ;
#6855 = EDGE_CURVE ( 'NONE', #19345, #19020, #22455, .T. ) ;
#6856 = VECTOR ( 'NONE', #29265, 39.37007874015748143 ) ;
#6857 = CARTESIAN_POINT ( 'NONE',  ( 0.1560064421674209612, -1.343171649511100796, 0.6771907574492684878 ) ) ;
#6859 = VERTEX_POINT ( 'NONE', #5319 ) ;
#6858 = EDGE_LOOP ( 'NONE', ( #5989, #20085, #30166, #15106 ) ) ;
#6860 = ADVANCED_FACE ( 'NONE', ( #10921 ), #39696, .F. ) ;
#6861 = CARTESIAN_POINT ( 'NONE',  ( 2.696301922142129510E-33, 0.7171888913565960255, -0.3575238883388469069 ) ) ;
#6862 = DIRECTION ( 'NONE',  ( 0.4999551463232373427, -0.8660512985181134660, 0.000000000000000000 ) ) ;
#6863 = DIRECTION ( 'NONE',  ( 0.000000000000000000, 0.000000000000000000, -1.000000000000000000 ) ) ;
#6864 = EDGE_CURVE ( 'NONE', #17453, #26250, #40070, .T. ) ;
#6865 = CARTESIAN_POINT ( 'NONE',  ( 0.5986388623866938374, -1.596970510946166266, 0.4258794442771735023 ) ) ;
#6866 = CARTESIAN_POINT ( 'NONE',  ( 0.2626070881998294193, -0.6796769646063650638, 0.05684369497733833543 ) ) ;
#6867 = ORIENTED_EDGE ( 'NONE', *, *, #10577, .F. ) ;
#6868 = CARTESIAN_POINT ( 'NONE',  ( 0.09375000000000006939, -0.4427825420493723962, 0.1899451958498858395 ) ) ;
#6869 = EDGE_CURVE ( 'NONE', #18110, #37905, #23488, .T. ) ;
#6870 = CARTESIAN_POINT ( 'NONE',  ( 0.1579683488041129513, -0.7702448364953791149, 0.5611987017360021701 ) ) ;
#6871 = VERTEX_POINT ( 'NONE', #8013 ) ;
#6872 = CARTESIAN_POINT ( 'NONE',  ( 0.05196282386221179328, -0.7503617116158776135, 0.7499995989107329786 ) ) ;
#6873 = CARTESIAN_POINT ( 'NONE',  ( 0.4704130467040563701, -1.558075432898772261, 0.5842460006296394948 ) ) ;
#6875 = DIRECTION ( 'NONE',  ( 0.9766636885342062646, -0.2147743920926303007, 0.000000000000000000 ) ) ;
#6874 = DIRECTION ( 'NONE',  ( 0.4999999999999978351, 0.7308273574226412661, 0.4646411234949410218 ) ) ;
#6876 = CARTESIAN_POINT ( 'NONE',  ( 0.6252332368506442473, -1.468099812651720182, 0.5083331137473884320 ) ) ;
#6877 = CYLINDRICAL_SURFACE ( 'NONE', #21174, 0.08139150547213643005 ) ;
#6878 = AXIS2_PLACEMENT_3D ( 'NONE', #20397, #39501, #13802 ) ;
#6879 = CARTESIAN_POINT ( 'NONE',  ( -0.2399999999999999079, -2.183180860297908144, -0.5562760292030870524 ) ) ;
#6880 = CARTESIAN_POINT ( 'NONE',  ( 0.1153471661800046788, -0.4465907051537519323, 0.1458683203705896103 ) ) ;
#6881 = AXIS2_PLACEMENT_3D ( 'NONE', #10388, #1350, #26432 ) ;
#6882 = CARTESIAN_POINT ( 'NONE',  ( -0.05634490452573035629, 0.2656249956367463527, -0.3742168499391961278 ) ) ;
#6883 = AXIS2_PLACEMENT_3D ( 'NONE', #38173, #35303, #9997 ) ;
#6884 = EDGE_CURVE ( 'NONE', #19865, #40308, #21701, .T. ) ;
#6885 = LOCAL_TIME ( 0, 53, 7.000000000000000000, #24688 ) ;
#6886 = APPROVAL ( #330, 'UNSPECIFIED' ) ;
#6887 = DIRECTION ( 'NONE',  ( 0.000000000000000000, 1.000000000000000000, -2.162712994984206616E-14 ) ) ;
#6888 = DIRECTION ( 'NONE',  ( -2.465190328815661892E-32, -1.000000000000000000, 5.978086547377980964E-31 ) ) ;
#6889 = APPLICATION_CONTEXT ( 'configuration controlled 3d designs of mechanical parts and assemblies' ) ;
#6890 = AXIS2_PLACEMENT_3D ( 'NONE', #1512, #39140, #36042 ) ;
#6891 = CARTESIAN_POINT ( 'NONE',  ( 0.1927699586607699855, -0.5931527414817471255, 0.2350819919684725701 ) ) ;
#6892 = CARTESIAN_POINT ( 'NONE',  ( 0.01548846960706664298, 0.09061086148576029398, -0.5171215251571253946 ) ) ;
#6893 = CARTESIAN_POINT ( 'NONE',  ( 0.06748114818349953969, -1.314123476931967405, 0.6039052066682303321 ) ) ;
#6894 = B_SPLINE_CURVE_WITH_KNOTS ( 'NONE', 3,
 ( #30877, #15652, #12769, #28201, #2694, #21839, #65, #12557, #25117, #15241, #2503, #31488, #3295, #9687, #37044, #21445, #5776, #37255, #40120, #6573, #21635, #273, #25332, #34157, #31084, #37871, #30686, #1076, #19151, #13373, #31901, #7177, #10485, #25947, #6995, #7378, #19745, #3719, #32281, #23050, #13767, #9873, #28616, #35387, #34976, #25532, #23261, #19954, #35195, #10688, #3512, #22870, #866, #13585, #13160, #19565 ),
 .UNSPECIFIED., .F., .F.,
 ( 4, 2, 2, 2, 2, 2, 2, 2, 2, 2, 2, 2, 2, 2, 2, 2, 2, 2, 2, 2, 2, 2, 2, 2, 2, 2, 2, 4 ),
 ( 0.000000000000000000, 0.001448614964254715766, 0.002897229928509431531, 0.004345844892764147947, 0.005070152374891505505, 0.005794459857018863062, 0.006518767339146220620, 0.007243074821273579045, 0.008691689785528287221, 0.01014030474978299540, 0.01158891971403770357, 0.01303753467829241175, 0.01448614964254711819, 0.01738337957105653281, 0.02028060949956596304, 0.02172922446382067468, 0.02317783942807537939, 0.02462645439233009104, 0.02607506935658480268, 0.02897229928509421557, 0.03186952921360363539, 0.03476675914211305174, 0.04056121899913189138, 0.04345844892764130774, 0.04490706389189601244, 0.04563137137402337173, 0.04599352511508705138, 0.04635567885615073103 ),
 .UNSPECIFIED. ) ;
#6895 = CARTESIAN_POINT ( 'NONE',  ( 0.04047170147976451166, 0.4536011460193595246, -0.2133323880731119726 ) ) ;
#6896 = CARTESIAN_POINT ( 'NONE',  ( 0.3923243630925510872, -1.966611948492501316, -0.4968729097670202544 ) ) ;
#6897 = CARTESIAN_POINT ( 'NONE',  ( 0.2755167558405882677, -0.9831624882773356555, 0.7046348054233062541 ) ) ;
#6898 = CARTESIAN_POINT ( 'NONE',  ( 0.03159140494780057068, -0.2432984029592170083, 0.4277399113045166623 ) ) ;
#6899 = CARTESIAN_POINT ( 'NONE',  ( -1.019575837292305609, -0.04310840302198155199, 0.3599999999999999867 ) ) ;
#6900 = ORIENTED_EDGE ( 'NONE', *, *, #13180, .T. ) ;
#6901 = LINE ( 'NONE', #31812, #36465 ) ;
#6902 = CARTESIAN_POINT ( 'NONE',  ( 0.3854517798335491685, -1.606485021356798937, -0.4131913823358430160 ) ) ;
#6903 = CIRCLE ( 'NONE', #22713, 0.1000000000000000194 ) ;
#6904 = DIRECTION ( 'NONE',  ( 0.4999551463232377313, -0.8660512985181132439, -0.000000000000000000 ) ) ;
#6905 = CARTESIAN_POINT ( 'NONE',  ( 0.1282169094755595540, -1.302307706640518203, 0.4238844375282422861 ) ) ;
#6906 = AXIS2_PLACEMENT_3D ( 'NONE', #17220, #29766, #26897 ) ;
#6907 = ORIENTED_EDGE ( 'NONE', *, *, #29276, .F. ) ;
#6908 = EDGE_CURVE ( 'NONE', #10935, #19587, #1472, .T. ) ;
#6909 = CARTESIAN_POINT ( 'NONE',  ( -0.1668894944044049256, 0.4852776769345336638, 0.3312153816179680410 ) ) ;
#6910 = CARTESIAN_POINT ( 'NONE',  ( 0.1842405141775073085, -0.5317127165793841259, 0.2455185872253249635 ) ) ;
#6911 = LOCAL_TIME ( 0, 53, 7.000000000000000000, #32344 ) ;
#6912 = CARTESIAN_POINT ( 'NONE',  ( 0.05999999999999990757, -2.357338251929976383E-33, 0.06250000000000000000 ) ) ;
#6913 = DIRECTION ( 'NONE',  ( 0.4999551463232372317, -0.8660512985181135770, 0.000000000000000000 ) ) ;
#6914 = ADVANCED_FACE ( 'NONE', ( #13987 ), #26766, .F. ) ;
#6915 = CARTESIAN_POINT ( 'NONE',  ( 0.4523950064470654286, -1.218585674146387410, 0.6985505283395704312 ) ) ;
#6917 = DIRECTION ( 'NONE',  ( 0.8660512985181132439, 0.4999551463232376758, 0.000000000000000000 ) ) ;
#6916 = CARTESIAN_POINT ( 'NONE',  ( -0.02000000000000000042, -1.758704040287260018, -0.8825853814972600686 ) ) ;
#6918 = CARTESIAN_POINT ( 'NONE',  ( 0.3689192748036780878, -1.014666054483551294, 0.6186952232919745720 ) ) ;
#6919 = ORIENTED_EDGE ( 'NONE', *, *, #18967, .F. ) ;
#6920 = CONTEXT_DEPENDENT_SHAPE_REPRESENTATION ( #9545, #35734 ) ;
#6921 = EDGE_CURVE ( 'NONE', #24870, #26513, #24324, .T. ) ;
#6922 = AXIS2_PLACEMENT_3D ( 'NONE', #2467, #15001, #40079 ) ;
#6923 = CARTESIAN_POINT ( 'NONE',  ( -0.02000000000000000042, -2.196071624283071788, -0.8624000883860228894 ) ) ;
#6924 = ORIENTED_EDGE ( 'NONE', *, *, #1417, .F. ) ;
#6925 = ORIENTED_EDGE ( 'NONE', *, *, #34633, .F. ) ;
#6926 = CARTESIAN_POINT ( 'NONE',  ( 0.04803225083625260738, -0.5400094135379269744, 0.1831641058994340765 ) ) ;
#6928 = CARTESIAN_POINT ( 'NONE',  ( 0.2028802569692557956, -0.6553668614656892322, 0.3449618718442576393 ) ) ;
#6927 = FACE_OUTER_BOUND ( 'NONE', #8095, .T. ) ;
#6929 = CARTESIAN_POINT ( 'NONE',  ( 0.06889123515197598246, -0.5474947681545639933, 0.09816793099005483025 ) ) ;
#6930 = EDGE_LOOP ( 'NONE', ( #24337, #3927, #17011, #4795, #304 ) ) ;
#6931 = VERTEX_POINT ( 'NONE', #11116 ) ;
#6932 = DIRECTION ( 'NONE',  ( -1.000000000000000000, -0.000000000000000000, -0.000000000000000000 ) ) ;
#6933 = CARTESIAN_POINT ( 'NONE',  ( 0.5667293957721729614, -1.503181826980968472, 0.5693608068383182452 ) ) ;
#6934 = ORIENTED_EDGE ( 'NONE', *, *, #17479, .F. ) ;
#6935 = CARTESIAN_POINT ( 'NONE',  ( 0.3909832130543929307, -1.949124834775286974, -0.5003013863325592725 ) ) ;
#6936 = DIRECTION ( 'NONE',  ( -1.000000000000000000, -2.403560570595279103E-31, 1.725633230170969455E-31 ) ) ;
#6937 = DIRECTION ( 'NONE',  ( 0.9378410757839522605, -0.1072489841977682656, 0.3300784330442477765 ) ) ;
#6938 = ADVANCED_FACE ( 'NONE', ( #8225 ), #36136, .F. ) ;
#6939 = CARTESIAN_POINT ( 'NONE',  ( 0.4334910933930137267, -1.677114403799170317, -0.6121645795958546854 ) ) ;
#6940 = DIRECTION ( 'NONE',  ( 1.188678714063518227E-15, -1.000000000000000000, -3.263080277421930985E-16 ) ) ;
#6941 = CARTESIAN_POINT ( 'NONE',  ( 0.09999999999997892519, -2.097675824466505023, -0.2588528740066098344 ) ) ;
#6942 = CARTESIAN_POINT ( 'NONE',  ( 0.1443375672974070711, 0.000000000000000000, 0.000000000000000000 ) ) ;
#6943 = AXIS2_PLACEMENT_3D ( 'NONE', #33028, #24002, #33239 ) ;
#6944 = AXIS2_PLACEMENT_3D ( 'NONE', #19801, #4370, #7661 ) ;
#6945 = LINE ( 'NONE', #28564, #15964 ) ;
#6946 = CARTESIAN_POINT ( 'NONE',  ( 0.1934531163328969683, -1.995776386748306486, -0.7016548334849427304 ) ) ;
#6947 = DIRECTION ( 'NONE',  ( -7.000205099780314469E-17, -1.000000000000000000, 6.590151126658399604E-16 ) ) ;
#6948 = CARTESIAN_POINT ( 'NONE',  ( 0.3604846637226567507, -1.752356493123346182, -0.4785798120827651769 ) ) ;
#6949 = APPROVAL_STATUS ( 'not_yet_approved' ) ;
#6950 = LOCAL_TIME ( 0, 53, 7.000000000000000000, #35114 ) ;
#6951 = CARTESIAN_POINT ( 'NONE',  ( 0.6409176605149490280, -1.402773510675777935, -0.6244726438235953525 ) ) ;
#6952 = CARTESIAN_POINT ( 'NONE',  ( 0.1676768030379193752, -1.385557720720546060, 0.5132863183250160333 ) ) ;
#6953 = CARTESIAN_POINT ( 'NONE',  ( -0.1126900943355827051, -0.5191528601550228217, 0.3070571034468279059 ) ) ;
#6954 = LINE ( 'NONE', #4060, #38930 ) ;
#6955 = CIRCLE ( 'NONE', #29319, 0.01499999999999995781 ) ;
#6956 = CARTESIAN_POINT ( 'NONE',  ( 0.1499999999999994671, 0.5346638663566671834, 0.07572681171513505338 ) ) ;
#6957 =( BOUNDED_SURFACE ( )  B_SPLINE_SURFACE ( 3, 2, ( 
 ( #29468, #20414, #36236 ),
 ( #4751, #26602, #11349 ),
 ( #39519, #7440, #7656 ),
 ( #20627, #14237, #32545 ) ),
 .UNSPECIFIED., .F., .F., .T. ) 
 B_SPLINE_SURFACE_WITH_KNOTS ( ( 4, 4 ),
 ( 3, 3 ),
 ( -2.862293735361731706E-17, 0.001825051142017924174 ),
 ( 0.000000000000000000, 1.000000000000000000 ),
 .UNSPECIFIED. ) 
 GEOMETRIC_REPRESENTATION_ITEM ( )  RATIONAL_B_SPLINE_SURFACE ( (
 ( 1.000000000000000000, 0.7061763356917307721, 1.000000000000000000),
 ( 1.000000000000000000, 0.7067362331337568859, 1.000000000000000000),
 ( 1.000000000000000000, 0.7071034392571956539, 1.000000000000000000),
 ( 1.000000000000000000, 0.7071067811865460184, 1.000000000000000000) ) ) 
 REPRESENTATION_ITEM ( '' )  SURFACE ( )  );
#6958 = CARTESIAN_POINT ( 'NONE',  ( 0.004299088327612451445, -0.5973376383060815531, 0.3026940496400818970 ) ) ;
#6959 = CARTESIAN_POINT ( 'NONE',  ( -0.0003770264812326959230, -0.9303068966317035171, 0.08922538226795197203 ) ) ;
#6960 = CARTESIAN_POINT ( 'NONE',  ( 0.2410612609043008003, -1.582380839801596828, -0.7041768810579421833 ) ) ;
#6961 = FACE_OUTER_BOUND ( 'NONE', #25555, .T. ) ;
#6962 = LINE ( 'NONE', #10455, #27697 ) ;
#6963 = ORIENTED_EDGE ( 'NONE', *, *, #17686, .F. ) ;
#6964 = ORIENTED_EDGE ( 'NONE', *, *, #11506, .F. ) ;
#6965 = EDGE_CURVE ( 'NONE', #13311, #34957, #32843, .T. ) ;
#6966 = CARTESIAN_POINT ( 'NONE',  ( 0.3770485601393582797, -1.761594279002118402, -0.5750035625930455252 ) ) ;
#6967 = VERTEX_POINT ( 'NONE', #5127 ) ;
#6968 = CARTESIAN_POINT ( 'NONE',  ( 0.1399999999999994582, 0.000000000000000000, 0.000000000000000000 ) ) ;
#6969 = CARTESIAN_POINT ( 'NONE',  ( -0.05464101615137771650, -2.698373762442814350, -0.2370085142459261163 ) ) ;
#6970 = EDGE_CURVE ( 'NONE', #25200, #27922, #34913, .T. ) ;
#6971 = CARTESIAN_POINT ( 'NONE',  ( 0.5725852423738272412, -1.416104505180847850, 0.6504252674398794953 ) ) ;
#6973 = ORIENTED_EDGE ( 'NONE', *, *, #37835, .T. ) ;
#6972 = DIRECTION ( 'NONE',  ( -1.000000000000000000, -0.000000000000000000, -0.000000000000000000 ) ) ;
#6974 = CARTESIAN_POINT ( 'NONE',  ( 0.4220340746365390805, -1.009949560908969035, 0.7308913177996746446 ) ) ;
#6975 = AXIS2_PLACEMENT_3D ( 'NONE', #20769, #33292, #5906 ) ;
#6976 = ORIENTED_EDGE ( 'NONE', *, *, #6617, .T. ) ;
#6977 = DIRECTION ( 'NONE',  ( 0.4220386480983009392, 0.000000000000000000, -0.9065778397420479751 ) ) ;
#6978 = ORIENTED_EDGE ( 'NONE', *, *, #3996, .F. ) ;
#6979 = CARTESIAN_POINT ( 'NONE',  ( 0.2997790868238941475, -1.656668618253792857, 0.6120939283712725221 ) ) ;
#6981 = CARTESIAN_POINT ( 'NONE',  ( -0.02235124290213127279, -0.2417860359143738647, 0.4518977707513324171 ) ) ;
#6980 = CARTESIAN_POINT ( 'NONE',  ( 0.5403448000457757860, -1.667326427136834432, -0.4959994330086619496 ) ) ;
#6982 = CARTESIAN_POINT ( 'NONE',  ( 0.5054609057099638258, -1.017757956463559710, -0.5155029497116575543 ) ) ;
#6983 = SECURITY_CLASSIFICATION ( '', '', #1939 ) ;
#6984 = CARTESIAN_POINT ( 'NONE',  ( 0.1834116704161121436, -0.8266995537623093027, 0.1479976049341028554 ) ) ;
#6985 = CARTESIAN_POINT ( 'NONE',  ( 0.03025250162251530775, -1.950833258820844129, -0.3011725134765823597 ) ) ;
#6987 = ORIENTED_EDGE ( 'NONE', *, *, #29094, .T. ) ;
#6986 = ORIENTED_EDGE ( 'NONE', *, *, #23131, .F. ) ;
#6988 = DIRECTION ( 'NONE',  ( 0.000000000000000000, 0.000000000000000000, -1.000000000000000000 ) ) ;
#6989 = CIRCLE ( 'NONE', #14210, 2.001558204291726373 ) ;
#6990 = CARTESIAN_POINT ( 'NONE',  ( 0.1852697703518005334, -0.8388889655799377509, 0.1443021394693011494 ) ) ;
#6991 = CARTESIAN_POINT ( 'NONE',  ( -0.01896968469604851451, -0.4667670904252342323, 0.2292592343991424197 ) ) ;
#6992 = LINE ( 'NONE', #28613, #28604 ) ;
#6993 = EDGE_CURVE ( 'NONE', #10719, #6859, #37886, .T. ) ;
#6994 = CARTESIAN_POINT ( 'NONE',  ( 0.1033812429324503235, -0.8292951995117538999, 0.2127542378592026939 ) ) ;
#6995 = CARTESIAN_POINT ( 'NONE',  ( 0.09312660137187182829, -1.001924882690514051, 0.8305037475052123863 ) ) ;
#6996 = EDGE_CURVE ( 'NONE', #5340, #2068, #24093, .T. ) ;
#6997 = CARTESIAN_POINT ( 'NONE',  ( 0.1959265899308195724, -1.288818386415671036, -0.7414046965098800568 ) ) ;
#6998 = EDGE_CURVE ( 'NONE', #24800, #38179, #12376, .T. ) ;
#6999 = CARTESIAN_POINT ( 'NONE',  ( -0.1617502512268864101, 0.4682890762661574557, 0.3382895567546906346 ) ) ;
#7000 = CARTESIAN_POINT ( 'NONE',  ( 0.4409894265177971562, -1.112709430993880755, -0.5155029497116575543 ) ) ;
#7001 = EDGE_CURVE ( 'NONE', #19341, #24493, #31029, .T. ) ;
#7002 = DIRECTION ( 'NONE',  ( 7.771561172376107616E-16, -7.170354002788761615E-17, 1.000000000000000000 ) ) ;
#7003 = CARTESIAN_POINT ( 'NONE',  ( -0.2399999999999999079, -3.253611865733782693, -0.3464478357516359575 ) ) ;
#7004 =( CONVERSION_BASED_UNIT ( 'INCH', #18758 ) LENGTH_UNIT ( ) NAMED_UNIT ( #7294 ) );
#7005 = CARTESIAN_POINT ( 'NONE',  ( 0.05634206451479473882, -0.2613530514269480909, 0.3773282889206444057 ) ) ;
#7006 = CARTESIAN_POINT ( 'NONE',  ( -0.2399999999999999079, -2.511040369707300268, -0.4948468226404901804 ) ) ;
#7007 = CARTESIAN_POINT ( 'NONE',  ( 0.1935645654550193218, -1.998378335482414947, -0.6716191072629904557 ) ) ;
#7008 = ORGANIZATION ( 'NAUO-ORG18', 'UNSPECIFIED', 'UNSPECIFIED' ) ;
#7009 = CARTESIAN_POINT ( 'NONE',  ( -0.1212602504878774051, -0.5073146173917495450, 0.3032895567580812246 ) ) ;
#7010 = FACE_OUTER_BOUND ( 'NONE', #2241, .T. ) ;
#7011 = CARTESIAN_POINT ( 'NONE',  ( -0.03647060353176813374, 0.5060729159580379388, 0.07645842516612116890 ) ) ;
#7012 = DIRECTION ( 'NONE',  ( -0.6036887133119795967, -0.3484981542248280495, 0.7170139286803393075 ) ) ;
#7013 = CIRCLE ( 'NONE', #3738, 0.1000000000000000194 ) ;
#7014 = FACE_OUTER_BOUND ( 'NONE', #15885, .T. ) ;
#7015 = EDGE_LOOP ( 'NONE', ( #40483, #19168 ) ) ;
#7016 = DIRECTION ( 'NONE',  ( 0.000000000000000000, -3.330669073875470114E-16, -1.000000000000000000 ) ) ;
#7017 = CARTESIAN_POINT ( 'NONE',  ( 0.2640642850859278856, -1.687144750073774624, 0.5604289873973611336 ) ) ;
#7018 = EDGE_CURVE ( 'NONE', #32180, #5888, #31628, .T. ) ;
#7019 = CARTESIAN_POINT ( 'NONE',  ( 0.5948731947484026117, -1.487188044069185144, 0.5720353766658540229 ) ) ;
#7021 = ORIENTED_EDGE ( 'NONE', *, *, #16097, .T. ) ;
#7020 = CARTESIAN_POINT ( 'NONE',  ( -0.02000000000000000042, -2.177105168660885326, -0.2518349584362399862 ) ) ;
#7022 = EDGE_CURVE ( 'NONE', #22988, #2067, #5539, .T. ) ;
#7024 = VERTEX_POINT ( 'NONE', #27566 ) ;
#7023 = VERTEX_POINT ( 'NONE', #21188 ) ;
#7025 = CARTESIAN_POINT ( 'NONE',  ( 0.6457951246584852090, -1.496021715571339339, 0.7857184687380228683 ) ) ;
#7026 = VERTEX_POINT ( 'NONE', #11919 ) ;
#7027 = CARTESIAN_POINT ( 'NONE',  ( 0.3663209872086246599, -1.109675523170870148, 0.7013152411065209924 ) ) ;
#7028 = CARTESIAN_POINT ( 'NONE',  ( 0.4042633028796379646, -1.711240744074478570, 0.4220515681607872605 ) ) ;
#7029 = COORDINATED_UNIVERSAL_TIME_OFFSET ( 0, 0, .AHEAD. ) ;
#7030 = CARTESIAN_POINT ( 'NONE',  ( -0.004127514673257773846, -0.8469330747986104635, 0.1483282180229327507 ) ) ;
#7031 = ORIENTED_EDGE ( 'NONE', *, *, #1924, .F. ) ;
#7032 = CIRCLE ( 'NONE', #3757, 0.1600000000000006140 ) ;
#7033 = CARTESIAN_POINT ( 'NONE',  ( 0.08599367632086754587, -0.8130461822548644690, 0.1957551766224920053 ) ) ;
#7034 = CARTESIAN_POINT ( 'NONE',  ( 0.08991114079686372829, -0.5436709457187953731, 0.1483399283896538745 ) ) ;
#7035 = CARTESIAN_POINT ( 'NONE',  ( 0.5397793955047566206, -1.519018766216045702, 0.5864989580874288011 ) ) ;
#7036 = ORIENTED_EDGE ( 'NONE', *, *, #7706, .T. ) ;
#7037 = CARTESIAN_POINT ( 'NONE',  ( 0.6299594025232742034, -1.615593600489037884, -0.5387823541095865254 ) ) ;
#7038 = CARTESIAN_POINT ( 'NONE',  ( -0.1613941803225988625, 0.5013693709968661816, 0.1260513636289518347 ) ) ;
#7039 = CARTESIAN_POINT ( 'NONE',  ( -0.05283719472145168711, 0.03966590960886611644, 0.4666299489511758214 ) ) ;
#7040 = CARTESIAN_POINT ( 'NONE',  ( -0.2746410161513779258, -2.068584980338025847, -0.2731141320652225035 ) ) ;
#7041 = CARTESIAN_POINT ( 'NONE',  ( 0.05999999999999990757, -0.4578766358967566452, -0.4053162176620347945 ) ) ;
#7042 = CARTESIAN_POINT ( 'NONE',  ( 0.4955364640417493360, -1.624781976271624462, -0.5908697979789261368 ) ) ;
#7043 = CARTESIAN_POINT ( 'NONE',  ( 0.1634626058761369516, -0.6765147025655514623, 0.4580962369789614019 ) ) ;
#7044 = CARTESIAN_POINT ( 'NONE',  ( -0.0001224597784096040007, -0.7987101862150752796, -0.07726980077153194904 ) ) ;
#7045 = CARTESIAN_POINT ( 'NONE',  ( 0.2316917763911649497, -1.232208891764917880, 0.5707417262808780478 ) ) ;
#7046 = CARTESIAN_POINT ( 'NONE',  ( 0.4546139439372508528, -1.086704419948380851, -0.6194763249030063035 ) ) ;
#7047 = CARTESIAN_POINT ( 'NONE',  ( 0.01226155556033644428, -1.026869578359442370, 0.5617476425356938696 ) ) ;
#7048 = B_SPLINE_CURVE_WITH_KNOTS ( 'NONE', 3,
 ( #11101, #1455, #11707, #8599, #13970, #20366, #4699, #17270, #29823, #30212 ),
 .UNSPECIFIED., .F., .F.,
 ( 4, 2, 2, 2, 4 ),
 ( 0.0002266766535735013997, 0.0007552434839518216026, 0.001283810314330141806, 0.001812377144708462008, 0.002340943975086781995 ),
 .UNSPECIFIED. ) ;
#7049 = CARTESIAN_POINT ( 'NONE',  ( 0.3816662009041032477, -0.9823246188028521564, 0.6672886469660396225 ) ) ;
#7050 = APPROVAL_ROLE ( '' ) ;
#7051 = CARTESIAN_POINT ( 'NONE',  ( 0.4795819664771984736, -1.106247336020415917, -0.4111404562665418871 ) ) ;
#7052 = CARTESIAN_POINT ( 'NONE',  ( -0.02869712619511913601, 0.4519224903895677770, -0.2102851490355765740 ) ) ;
#7053 = CARTESIAN_POINT ( 'NONE',  ( -0.05269191099235946696, 0.004472488327044489738, 0.4686046460979745309 ) ) ;
#7054 = VERTEX_POINT ( 'NONE', #37013 ) ;
#7055 = CARTESIAN_POINT ( 'NONE',  ( 0.5489247571685185179, -1.593093418273787254, -0.5155029497116575543 ) ) ;
#7056 = CARTESIAN_POINT ( 'NONE',  ( 0.01055999354155195448, -0.5296565605740115590, 0.1369805761320318227 ) ) ;
#7057 = DIRECTION ( 'NONE',  ( 0.000000000000000000, -0.8159412518334721032, -0.5781348229923762849 ) ) ;
#7058 = EDGE_LOOP ( 'NONE', ( #14508, #31437, #13961 ) ) ;
#7059 = CARTESIAN_POINT ( 'NONE',  ( 0.3210085668004670767, -1.182910313946810010, 0.5197417262808780025 ) ) ;
#7060 = AXIS2_PLACEMENT_3D ( 'NONE', #6457, #19230, #560 ) ;
#7061 = CARTESIAN_POINT ( 'NONE',  ( 0.5586414499496984432, -1.205790344466990627, 0.8068181458027993136 ) ) ;
#7063 = ORIENTED_EDGE ( 'NONE', *, *, #19478, .T. ) ;
#7062 = ORIENTED_EDGE ( 'NONE', *, *, #20744, .F. ) ;
#7064 = CARTESIAN_POINT ( 'NONE',  ( -0.01548846960707545191, -0.5198120922912100594, 0.07362328916748400731 ) ) ;
#7065 = ORIENTED_EDGE ( 'NONE', *, *, #2465, .F. ) ;
#7066 = DIRECTION ( 'NONE',  ( -0.8660512985181134660, -0.4999551463232372317, 0.000000000000000000 ) ) ;
#7067 = ORIENTED_EDGE ( 'NONE', *, *, #876, .F. ) ;
#7068 = CARTESIAN_POINT ( 'NONE',  ( 0.1891522879705697380, -0.6779850459293743636, 0.7094297601507593143 ) ) ;
#7069 = CARTESIAN_POINT ( 'NONE',  ( 0.08990515874724788747, -0.5631160408504085613, 0.1457185332388709342 ) ) ;
#7070 = CARTESIAN_POINT ( 'NONE',  ( 0.001612557744564022772, -0.4658981512586417018, 0.3165272632837566325 ) ) ;
#7071 = CARTESIAN_POINT ( 'NONE',  ( 0.1678425801914835702, -0.8396823097241469247, 0.6722826835357673669 ) ) ;
#7073 = CARTESIAN_POINT ( 'NONE',  ( -0.1129900121204265445, -0.5167580615070231920, 0.3146079272632528734 ) ) ;
#7072 = CARTESIAN_POINT ( 'NONE',  ( 0.5288925617653345013, -1.600649924176790417, -0.4348607546581709227 ) ) ;
#7074 = CARTESIAN_POINT ( 'NONE',  ( 0.4296888835344449542, -1.088254846990821090, 0.6262898891649716360 ) ) ;
#7075 = VERTEX_POINT ( 'NONE', #40515 ) ;
#7076 = ADVANCED_FACE ( 'NONE', ( #8836 ), #1709, .T. ) ;
#7077 = CARTESIAN_POINT ( 'NONE',  ( 0.3786378199821132107, -1.610465949109882722, 0.5371432465038092907 ) ) ;
#7078 = B_SPLINE_CURVE_WITH_KNOTS ( 'NONE', 3,
 ( #24023, #1602, #24216, #26480 ),
 .UNSPECIFIED., .F., .F.,
 ( 4, 4 ),
 ( 1.063271609842796554E-14, 0.0008871692367504230205 ),
 .UNSPECIFIED. ) ;
#7079 = CARTESIAN_POINT ( 'NONE',  ( 0.1897120355916300793, -0.5340628431043178415, 0.1475512043905171100 ) ) ;
#7080 = CARTESIAN_POINT ( 'NONE',  ( -0.02872242845530505531, 0.3729171224323672984, -0.3802687114177490946 ) ) ;
#7081 = CARTESIAN_POINT ( 'NONE',  ( 0.4741640079579751421, -1.162838329081267830, -0.4122610257295771796 ) ) ;
#7082 = CARTESIAN_POINT ( 'NONE',  ( 0.4165761542997364897, -1.741708882820427906, 0.5182417262812423209 ) ) ;
#7083 = CIRCLE ( 'NONE', #25500, 0.1700000000000001510 ) ;
#7084 = CARTESIAN_POINT ( 'NONE',  ( 0.5289273032196292190, -1.159758851219879094, 0.8099624798310959273 ) ) ;
#7085 = CARTESIAN_POINT ( 'NONE',  ( -0.2399999999999999079, -2.183180860297908144, -0.4937760292030871079 ) ) ;
#7086 = CARTESIAN_POINT ( 'NONE',  ( -0.002288348195439183011, -0.8555288687844084805, 0.1911206019478631501 ) ) ;
#7087 = CARTESIAN_POINT ( 'NONE',  ( 0.03303737228521517327, 0.4610015631984470952, -0.2426019986921478244 ) ) ;
#7088 = CARTESIAN_POINT ( 'NONE',  ( -0.2746410161513779258, -2.457388234162025675, -0.5792354969483111127 ) ) ;
#7089 = ORIENTED_EDGE ( 'NONE', *, *, #35574, .T. ) ;
#7090 = CARTESIAN_POINT ( 'NONE',  ( 0.2388518348206360165, -0.9447629884332594541, 0.6674861025992597785 ) ) ;
#7091 = CARTESIAN_POINT ( 'NONE',  ( 0.01548846960712783535, -0.2450655194479442189, 0.4674710490748163472 ) ) ;
#7092 = DIRECTION ( 'NONE',  ( 0.000000000000000000, 0.000000000000000000, -1.000000000000000000 ) ) ;
#7093 = VERTEX_POINT ( 'NONE', #21608 ) ;
#7094 = DIRECTION ( 'NONE',  ( 0.4999551463232385085, -0.8660512985181127998, 0.000000000000000000 ) ) ;
#7095 = CARTESIAN_POINT ( 'NONE',  ( 0.4165289612193914248, -1.649214957849692187, -0.4090022746516587815 ) ) ;
#7096 = CARTESIAN_POINT ( 'NONE',  ( -0.01548846960707524721, 0.000000000000000000, 0.000000000000000000 ) ) ;
#7097 = CARTESIAN_POINT ( 'NONE',  ( 0.1209954157056817858, -1.306288454297929169, 0.4272974746133751944 ) ) ;
#7098 = CARTESIAN_POINT ( 'NONE',  ( 0.2750207689086996421, -1.313593350392348036, 0.6206863215409638146 ) ) ;
#7099 = ORIENTED_EDGE ( 'NONE', *, *, #34401, .T. ) ;
#7100 = CARTESIAN_POINT ( 'NONE',  ( -0.1542173385434630895, 0.4780076866987719719, 0.3460825593793663835 ) ) ;
#7101 = ADVANCED_FACE ( 'NONE', ( #31268 ), #24278, .T. ) ;
#7102 = DIRECTION ( 'NONE',  ( 1.000000000000000000, 2.280301054154495132E-31, -1.664003471950577689E-31 ) ) ;
#7103 = CARTESIAN_POINT ( 'NONE',  ( 0.4805026040976208002, -1.666128583310215294, 0.5622881460297129985 ) ) ;
#7104 = APPROVAL ( #38724, 'UNSPECIFIED' ) ;
#7105 = CARTESIAN_POINT ( 'NONE',  ( 0.1858317078876725870, -0.7573081918228976583, 0.1167702249826223643 ) ) ;
#7106 = CARTESIAN_POINT ( 'NONE',  ( 0.4598716470225525654, -1.229368431601224110, 0.6930793938347281635 ) ) ;
#7108 = CARTESIAN_POINT ( 'NONE',  ( -0.2746410161513770931, -2.878813263491020180, -0.3823467908819087602 ) ) ;
#7107 = DIRECTION ( 'NONE',  ( -2.563099466555617214E-12, 0.9510565162951502005, -0.3090169943749580539 ) ) ;
#7109 = CARTESIAN_POINT ( 'NONE',  ( 0.4916028908188559421, -1.081978336766327820, 0.5838299722441698814 ) ) ;
#7110 = ORIENTED_EDGE ( 'NONE', *, *, #37358, .F. ) ;
#7111 = PERSON_AND_ORGANIZATION ( #9840, #1075 ) ;
#7112 = CARTESIAN_POINT ( 'NONE',  ( 0.07011823623339116796, -1.185871634737858171, 0.7567465950153516863 ) ) ;
#7113 = ORIENTED_EDGE ( 'NONE', *, *, #16045, .T. ) ;
#7114 = ORIENTED_EDGE ( 'NONE', *, *, #1734, .F. ) ;
#7115 = CARTESIAN_POINT ( 'NONE',  ( 0.08620743421842372300, -0.7306438661145220337, 0.5678638921208791768 ) ) ;
#7117 = CARTESIAN_POINT ( 'NONE',  ( 0.1842589411986597370, -0.8539449830211861547, 0.1384146430135328731 ) ) ;
#7116 = CARTESIAN_POINT ( 'NONE',  ( 0.08513901846483432068, -0.8317911747034616443, 0.1390917317614507875 ) ) ;
#7118 = CARTESIAN_POINT ( 'NONE',  ( 0.06806991437983572757, -0.5898870860155140949, 0.03457737503348648489 ) ) ;
#7119 = ORIENTED_EDGE ( 'NONE', *, *, #34048, .T. ) ;
#7120 = ORIENTED_EDGE ( 'NONE', *, *, #36389, .T. ) ;
#7121 = CARTESIAN_POINT ( 'NONE',  ( 0.5350245160856361704, -1.154637332899181246, 0.6150156329573506220 ) ) ;
#7122 = CARTESIAN_POINT ( 'NONE',  ( 0.2091282673351387011, -0.8319368543454188636, 0.6504350734237481779 ) ) ;
#7123 = ORIENTED_EDGE ( 'NONE', *, *, #21287, .T. ) ;
#7124 = CARTESIAN_POINT ( 'NONE',  ( 0.1874519294469400021, -0.6898179517609425160, 0.05346267245209616881 ) ) ;
#7125 = CARTESIAN_POINT ( 'NONE',  ( 0.4768809664655372926, -1.091612543784717282, -0.6129809598074057453 ) ) ;
#7126 = CARTESIAN_POINT ( 'NONE',  ( -0.3000000000000000999, -3.941790907013290823, -0.4084369376873030477 ) ) ;
#7127 = PRODUCT_DEFINITION_SHAPE ( 'NONE', 'NONE',  #35536 ) ;
#7128 = DIRECTION ( 'NONE',  ( 0.000000000000000000, 0.000000000000000000, 1.000000000000000000 ) ) ;
#7129 = CARTESIAN_POINT ( 'NONE',  ( -0.2399999999999999079, -3.525450504378606187, -0.1357627943591874498 ) ) ;
#7130 = CARTESIAN_POINT ( 'NONE',  ( 0.08807197818943472700, -0.6448060706081871762, 0.02183434420668394632 ) ) ;
#7131 = EDGE_CURVE ( 'NONE', #26308, #19197, #37840, .T. ) ;
#7132 = CARTESIAN_POINT ( 'NONE',  ( 0.7433653656267760201, -1.515745490836327924, 0.5775132586956883696 ) ) ;
#7133 = EDGE_CURVE ( 'NONE', #11981, #19690, #2649, .T. ) ;
#7134 = CARTESIAN_POINT ( 'NONE',  ( 0.3881547982128820684, -1.813545243782807459, -0.6998239732715378913 ) ) ;
#7135 = CYLINDRICAL_SURFACE ( 'NONE', #30605, 0.04330708661417343591 ) ;
#7136 = FACE_OUTER_BOUND ( 'NONE', #25976, .T. ) ;
#7137 = PERSON_AND_ORGANIZATION ( #28500, #32463 ) ;
#7138 = ADVANCED_FACE ( 'NONE', ( #22628 ), #35162, .F. ) ;
#7139 = DIRECTION ( 'NONE',  ( 0.4999551463232372872, -0.8660512985181134660, 0.000000000000000000 ) ) ;
#7140 = CARTESIAN_POINT ( 'NONE',  ( 0.2059273467974224725, -1.283046334493782137, -0.3824824602286829855 ) ) ;
#7141 = CARTESIAN_POINT ( 'NONE',  ( 0.1841294022395738306, -0.8546492471812711100, 0.1354054936157914613 ) ) ;
#7142 = EDGE_CURVE ( 'NONE', #10109, #9291, #6962, .T. ) ;
#7143 = CARTESIAN_POINT ( 'NONE',  ( 0.4229018694943574297, -1.238637407943166791, 0.4882188691235973543 ) ) ;
#7144 = DIRECTION ( 'NONE',  ( -1.000000000000000000, -2.280301054154495132E-31, 1.664003471950577689E-31 ) ) ;
#7145 = CARTESIAN_POINT ( 'NONE',  ( 0.006982617232424345385, -0.7536834681452820872, 0.4384055362127323718 ) ) ;
#7146 = CARTESIAN_POINT ( 'NONE',  ( 0.0001836465996860709934, -0.5357902603937784169, -0.05245457546160120499 ) ) ;
#7147 = LINE ( 'NONE', #7566, #16013 ) ;
#7148 = FACE_OUTER_BOUND ( 'NONE', #26843, .T. ) ;
#7149 = DIRECTION ( 'NONE',  ( -1.000000000000000000, 0.000000000000000000, 0.000000000000000000 ) ) ;
#7150 = ORIENTED_EDGE ( 'NONE', *, *, #10546, .T. ) ;
#7151 = ORIENTED_EDGE ( 'NONE', *, *, #34872, .T. ) ;
#7152 = EDGE_CURVE ( 'NONE', #8912, #39763, #9946, .T. ) ;
#7153 = CARTESIAN_POINT ( 'NONE',  ( 0.1614670899430008522, -0.7569536277469717245, 0.1022936816274460647 ) ) ;
#7154 = ORIENTED_EDGE ( 'NONE', *, *, #39340, .T. ) ;
#7155 = CARTESIAN_POINT ( 'NONE',  ( -0.01548846960712804005, -0.07651041855114824874, 0.5222379212567086482 ) ) ;
#7156 = CARTESIAN_POINT ( 'NONE',  ( -0.1304423469995341367, -0.5262799683630393632, 0.1000000000000000194 ) ) ;
#7157 = CARTESIAN_POINT ( 'NONE',  ( 0.3983136147636711644, -1.144903201110497593, 0.7729865516086456001 ) ) ;
#7159 = ORIENTED_EDGE ( 'NONE', *, *, #15821, .T. ) ;
#7158 = DIRECTION ( 'NONE',  ( -8.881784197001246407E-16, 2.361472542561082612E-16, -1.000000000000000000 ) ) ;
#7160 = CARTESIAN_POINT ( 'NONE',  ( 0.1937691639527174270, -0.6993326081247003279, 0.2764035553309984738 ) ) ;
#7161 = CARTESIAN_POINT ( 'NONE',  ( 0.3798092287356915620, -1.663952012720910867, -0.6129662916473187506 ) ) ;
#7162 = ORIENTED_EDGE ( 'NONE', *, *, #17922, .T. ) ;
#7163 = CARTESIAN_POINT ( 'NONE',  ( 0.5534916983399480461, -1.623563701787261948, 0.5248117263889745532 ) ) ;
#7164 = EDGE_LOOP ( 'NONE', ( #34299, #19924 ) ) ;
#7165 = CARTESIAN_POINT ( 'NONE',  ( 0.3024541409145408144, -1.545329219595432013, 0.8499871361866473407 ) ) ;
#7167 = CARTESIAN_POINT ( 'NONE',  ( 0.1127355578498012850, -0.7499205974406458752, -0.08760834960717918396 ) ) ;
#7166 = DIRECTION ( 'NONE',  ( 0.01455087615875040596, 0.9998941303973200023, 0.000000000000000000 ) ) ;
#7168 = DIRECTION ( 'NONE',  ( -1.000000000000000000, -1.138269997360101095E-15, 1.138269997360101095E-15 ) ) ;
#7169 = B_SPLINE_CURVE_WITH_KNOTS ( 'NONE', 3,
 ( #18569, #40158, #18785, #27440 ),
 .UNSPECIFIED., .F., .F.,
 ( 4, 4 ),
 ( 0.000000000000000000, 0.0002162507978265289883 ),
 .UNSPECIFIED. ) ;
#7170 = CARTESIAN_POINT ( 'NONE',  ( -2.097120186386331940E-14, -2.097675824466503691, -0.2907077406111385764 ) ) ;
#7171 = ORIENTED_EDGE ( 'NONE', *, *, #13249, .T. ) ;
#7172 = DIRECTION ( 'NONE',  ( 1.000000000000000000, 6.779273404243070203E-32, 4.314083075427408311E-32 ) ) ;
#7173 = CARTESIAN_POINT ( 'NONE',  ( 0.1868897438152673229, -0.9157227589292166181, 0.1874177539017474192 ) ) ;
#7174 = CYLINDRICAL_SURFACE ( 'NONE', #19365, 0.1620173459747806799 ) ;
#7175 = CARTESIAN_POINT ( 'NONE',  ( -0.1684323895664684156, 0.5231977504175356897, 0.1528658435937000626 ) ) ;
#7176 = CARTESIAN_POINT ( 'NONE',  ( 0.3865734956547689505, -1.160490560906283219, 0.7180718003458185228 ) ) ;
#7177 = CARTESIAN_POINT ( 'NONE',  ( 0.1102377350431349573, -1.066750407935357359, 0.8659539359857927332 ) ) ;
#7178 = CARTESIAN_POINT ( 'NONE',  ( 0.4395900988209245353, -1.153183135083376998, 0.4182417262808778013 ) ) ;
#7179 = CARTESIAN_POINT ( 'NONE',  ( 0.4753068003148404608, -1.208388544553129496, 0.5281503392817822329 ) ) ;
#7180 = EDGE_CURVE ( 'NONE', #3992, #15271, #13318, .T. ) ;
#7181 =( BOUNDED_SURFACE ( )  B_SPLINE_SURFACE ( 3, 2, ( 
 ( #30373, #15347, #34255 ),
 ( #5459, #18230, #40445 ),
 ( #33649, #31193, #40635 ),
 ( #18020, #2799, #11845 ),
 ( #21941, #3012, #27693 ),
 ( #14944, #6069, #12268 ),
 ( #37348, #30583, #9158 ),
 ( #27496, #24623, #34468 ),
 ( #12061, #2405, #37158 ),
 ( #27904, #40022, #18636 ),
 ( #33871, #24410, #36944 ),
 ( #12454, #5676, #2594 ),
 ( #15559, #8968, #34061 ),
 ( #28107, #8758, #21543 ),
 ( #24824, #5861, #25005 ),
 ( #40226, #18418, #21723 ),
 ( #37538, #21335, #9361 ),
 ( #21120, #30973, #30777 ) ),
 .UNSPECIFIED., .F., .F., .F. ) 
 B_SPLINE_SURFACE_WITH_KNOTS ( ( 4, 2, 2, 2, 2, 2, 2, 2, 4 ),
 ( 3, 3 ),
 ( 0.008382955743108795946, 0.008983498031186799154, 0.009584040319264800628, 0.01018458260734280384, 0.01078512489542080705, 0.01138566718349881025, 0.01198620947157681346, 0.01258675175965481494, 0.01318729404773281814 ),
 ( 0.000000000000000000, 1.000000000000000000 ),
 .UNSPECIFIED. ) 
 GEOMETRIC_REPRESENTATION_ITEM ( )  RATIONAL_B_SPLINE_SURFACE ( (
 ( 1.000000000000000000, 0.6939742941274812393, 1.000000000000000000),
 ( 1.000000000000000000, 0.6959340198092514029, 1.000000000000000000),
 ( 1.000000000000000000, 0.6976516493059798929, 1.000000000000000000),
 ( 1.000000000000000000, 0.7006068099166593566, 1.000000000000000000),
 ( 1.000000000000000000, 0.7018521079552784148, 1.000000000000000000),
 ( 1.000000000000000000, 0.7037991596780079906, 1.000000000000000000),
 ( 1.000000000000000000, 0.7045225278982292227, 1.000000000000000000),
 ( 1.000000000000000000, 0.7055270582749912922, 1.000000000000000000),
 ( 1.000000000000000000, 0.7057932885961764047, 1.000000000000000000),
 ( 1.000000000000000000, 0.7059503901902282053, 1.000000000000000000),
 ( 1.000000000000000000, 0.7058345562627796888, 1.000000000000000000),
 ( 1.000000000000000000, 0.7053003576585554768, 1.000000000000000000),
 ( 1.000000000000000000, 0.7048799844294983963, 1.000000000000000000),
 ( 1.000000000000000000, 0.7038033628364895877, 1.000000000000000000),
 ( 1.000000000000000000, 0.7031605846919154468, 1.000000000000000000),
 ( 1.000000000000000000, 0.7017073847940890063, 1.000000000000000000),
 ( 1.000000000000000000, 0.7008898196324485630, 1.000000000000000000),
 ( 1.000000000000000000, 0.7000494314910841176, 1.000000000000000000) ) ) 
 REPRESENTATION_ITEM ( '' )  SURFACE ( )  );
#7182 = CARTESIAN_POINT ( 'NONE',  ( 0.6404849880159927400, -1.549707582517539484, 0.4182417262808776348 ) ) ;
#7183 = FACE_OUTER_BOUND ( 'NONE', #14095, .T. ) ;
#7184 = APPROVAL_STATUS ( 'not_yet_approved' ) ;
#7185 = EDGE_CURVE ( 'NONE', #10881, #13458, #3874, .T. ) ;
#7186 = PLANE ( 'NONE',  #38317 ) ;
#7187 = ADVANCED_FACE ( 'NONE', ( #16035 ), #16425, .F. ) ;
#7188 = DIRECTION ( 'NONE',  ( 1.188678714063518227E-15, -1.000000000000000000, -3.263080277421930985E-16 ) ) ;
#7189 = B_SPLINE_CURVE_WITH_KNOTS ( 'NONE', 3,
 ( #23881, #2056, #1470, #11114, #39694, #7613, #36409, #20184 ),
 .UNSPECIFIED., .F., .F.,
 ( 4, 2, 2, 4 ),
 ( -5.999999998886577302E-08, 0.0008460481067746681693, 0.001692156213549325357, 0.003384372427098619133 ),
 .UNSPECIFIED. ) ;
#7190 = CARTESIAN_POINT ( 'NONE',  ( 0.2093553890865970102, -1.281067390074186907, -0.7153666112938229515 ) ) ;
#7191 = ORIENTED_EDGE ( 'NONE', *, *, #7412, .F. ) ;
#7192 = DIRECTION ( 'NONE',  ( -0.4999999999999991118, 0.5006794435238204333, -0.7066258520834617363 ) ) ;
#7193 = CARTESIAN_POINT ( 'NONE',  ( 0.4189043378923988370, -1.737431724743732753, -0.5872665585884508932 ) ) ;
#7194 = CARTESIAN_POINT ( 'NONE',  ( -0.05464101615137768181, -2.367354784411275670, -0.3586747285825516718 ) ) ;
#7195 = CARTESIAN_POINT ( 'NONE',  ( 0.6848280183511104013, -1.503484069889266861, 0.4560562289926599622 ) ) ;
#7196 = EDGE_CURVE ( 'NONE', #33728, #26101, #27098, .T. ) ;
#7197 = VERTEX_POINT ( 'NONE', #28584 ) ;
#7198 = CARTESIAN_POINT ( 'NONE',  ( 0.4314124229533453647, -1.133331723961105819, 0.4386204930848898176 ) ) ;
#7199 = ORIENTED_EDGE ( 'NONE', *, *, #40075, .F. ) ;
#7200 = DIRECTION ( 'NONE',  ( 1.445848444424219201E-15, -1.000000000000000000, -2.361472542561095431E-16 ) ) ;
#7201 = ADVANCED_FACE ( 'NONE', ( #28782 ), #238, .T. ) ;
#7202 = CARTESIAN_POINT ( 'NONE',  ( 0.1428682958407643810, -0.6238724032974017897, 0.3658253297163516771 ) ) ;
#7204 = ORIENTED_EDGE ( 'NONE', *, *, #766, .F. ) ;
#7203 = LINE ( 'NONE', #897, #4006 ) ;
#7205 = EDGE_CURVE ( 'NONE', #27945, #24904, #13342, .T. ) ;
#7207 = ORIENTED_EDGE ( 'NONE', *, *, #24228, .F. ) ;
#7206 = EDGE_LOOP ( 'NONE', ( #7571, #31002, #23075, #5323, #29851, #30850 ) ) ;
#7208 = CARTESIAN_POINT ( 'NONE',  ( -0.2399999999999999079, -2.183180860297908144, -0.4937760292030871079 ) ) ;
#7209 = ORIENTED_EDGE ( 'NONE', *, *, #21595, .F. ) ;
#7210 = EDGE_CURVE ( 'NONE', #36294, #20037, #5916, .T. ) ;
#7211 = LINE ( 'NONE', #5842, #21280 ) ;
#7212 = CARTESIAN_POINT ( 'NONE',  ( 0.6099797830822989431, -1.615543353997655585, -0.5095064010331072923 ) ) ;
#7213 = DATE_AND_TIME ( #25984, #29338 ) ;
#7214 = CARTESIAN_POINT ( 'NONE',  ( -0.0006246251967113254687, -0.4210325180397648248, 0.04185307883324617534 ) ) ;
#7215 = VERTEX_POINT ( 'NONE', #32246 ) ;
#7216 = CARTESIAN_POINT ( 'NONE',  ( 0.1776584764503561786, -0.8975873772128478700, 0.5749469949248323664 ) ) ;
#7217 = CARTESIAN_POINT ( 'NONE',  ( -0.2399999999999999079, -2.341127044584462968, -0.9908042926600856282 ) ) ;
#7218 = CARTESIAN_POINT ( 'NONE',  ( 0.3610670237709067143, -1.199828779861834338, 0.8410762739891641804 ) ) ;
#7219 = EDGE_LOOP ( 'NONE', ( #15437, #7642, #1578 ) ) ;
#7220 = CARTESIAN_POINT ( 'NONE',  ( 0.3484951945142048535, -1.627819363848378220, -0.3328913857909800433 ) ) ;
#7221 = CARTESIAN_POINT ( 'NONE',  ( 0.05999999999999990757, 0.7171888913565960255, -0.3575238883388469069 ) ) ;
#7222 = CARTESIAN_POINT ( 'NONE',  ( 0.6724801181750063028, -1.503114220331229323, 0.4114077743496406536 ) ) ;
#7223 = CIRCLE ( 'NONE', #30225, 0.09249999999977555343 ) ;
#7224 = CARTESIAN_POINT ( 'NONE',  ( 0.3974630593302357906, -1.726538153429652889, 0.6106779617088041734 ) ) ;
#7225 = CARTESIAN_POINT ( 'NONE',  ( 0.6893317334094206661, -1.420342506522920489, 0.6035468486318071868 ) ) ;
#7226 = CARTESIAN_POINT ( 'NONE',  ( 0.4992403769284946558, -1.623239255310001683, -0.5868208237444024755 ) ) ;
#7227 = FACE_BOUND ( 'NONE', #4479, .T. ) ;
#7228 = VECTOR ( 'NONE', #40521, 39.37007874015748143 ) ;
#7229 = CARTESIAN_POINT ( 'NONE',  ( 0.6092734426852441931, -1.479046879995318031, 0.5776141568224868461 ) ) ;
#7230 = CARTESIAN_POINT ( 'NONE',  ( -1.913577643379703278E-05, -0.8855436973319782412, -0.02478299547526676208 ) ) ;
#7231 = EDGE_CURVE ( 'NONE', #14919, #33383, #4070, .T. ) ;
#7232 = CARTESIAN_POINT ( 'NONE',  ( 0.008263909818985001182, -0.6872203660130532521, -0.01225013371141639093 ) ) ;
#7233 = CARTESIAN_POINT ( 'NONE',  ( 0.02235124290213229628, -0.4612278572487559236, -0.2234747101372517586 ) ) ;
#7234 = ADVANCED_FACE ( 'NONE', ( #24588 ), #25593, .T. ) ;
#7235 = CARTESIAN_POINT ( 'NONE',  ( 0.08897272204609851798, -1.263855944153051469, 0.7613784839713820807 ) ) ;
#7236 = CARTESIAN_POINT ( 'NONE',  ( 0.2389902554220701691, -0.8445547280628969977, 0.4765619450694277281 ) ) ;
#7237 = PERSON_AND_ORGANIZATION ( #28500, #32463 ) ;
#7238 = CARTESIAN_POINT ( 'NONE',  ( -0.2746410161513779258, -3.747168848490688209, -0.4747258284076885104 ) ) ;
#7239 = DIRECTION ( 'NONE',  ( -0.8660254037844403729, -0.4219433715391017192, -0.2682606777263723541 ) ) ;
#7240 = ORIENTED_EDGE ( 'NONE', *, *, #13433, .T. ) ;
#7241 = CARTESIAN_POINT ( 'NONE',  ( 0.3999999999999786504, -1.973385418564556293, -0.6834611762463905782 ) ) ;
#7242 = CARTESIAN_POINT ( 'NONE',  ( 0.002367446934001495983, -0.5282228851542395409, 0.1479114972776863768 ) ) ;
#7243 = AXIS2_PLACEMENT_3D ( 'NONE', #12851, #25815, #34447 ) ;
#7244 = CARTESIAN_POINT ( 'NONE',  ( -0.2399999999999999079, -2.322955634169589612, -0.9336221289765171960 ) ) ;
#7245 = VERTEX_POINT ( 'NONE', #21908 ) ;
#7246 = EDGE_CURVE ( 'NONE', #40610, #32592, #30978, .T. ) ;
#7247 = CARTESIAN_POINT ( 'NONE',  ( 0.3207148961678939481, -1.182401600646133089, 0.3667417262808778111 ) ) ;
#7248 = CARTESIAN_POINT ( 'NONE',  ( 0.6714320665202346827, -1.386459733509071368, 0.6790741990638067271 ) ) ;
#7250 = ORIENTED_EDGE ( 'NONE', *, *, #14485, .F. ) ;
#7249 = VERTEX_POINT ( 'NONE', #30942 ) ;
#7251 = CYLINDRICAL_SURFACE ( 'NONE', #5379, 1.991674066779348218 ) ;
#7252 = AXIS2_PLACEMENT_3D ( 'NONE', #20949, #4886, #33471 ) ;
#7253 = VERTEX_POINT ( 'NONE', #13044 ) ;
#7254 = CARTESIAN_POINT ( 'NONE',  ( -0.2399999999999999079, -3.268524983732795874, -0.6433364877554555994 ) ) ;
#7255 = CARTESIAN_POINT ( 'NONE',  ( 0.3798059133362846063, -1.714498463400732309, -0.3386984188363488801 ) ) ;
#7256 = CIRCLE ( 'NONE', #28949, 0.01499999999999995434 ) ;
#7257 = CARTESIAN_POINT ( 'NONE',  ( 0.2284923717121199460, -1.304659949875474068, -0.5155029497116575543 ) ) ;
#7258 = ORIENTED_EDGE ( 'NONE', *, *, #17720, .T. ) ;
#7259 = CARTESIAN_POINT ( 'NONE',  ( 0.1406250000000003331, -0.4510478692700826131, 0.1883489205008177791 ) ) ;
#7260 = CARTESIAN_POINT ( 'NONE',  ( 0.08922154937966106369, -0.6455529212171776665, 0.1844887113699342218 ) ) ;
#7261 = CARTESIAN_POINT ( 'NONE',  ( 0.07788054139780381524, -0.8406284514424815502, 0.8421199864423437598 ) ) ;
#7262 = CARTESIAN_POINT ( 'NONE',  ( 0.08912494520596493663, -0.5821696580930801890, 0.2929835240246161376 ) ) ;
#7264 = DIRECTION ( 'NONE',  ( -1.000000000000000000, -2.280301054154495132E-31, 1.664003471950577689E-31 ) ) ;
#7263 = CARTESIAN_POINT ( 'NONE',  ( 0.5092518242376296023, -1.618326942756133979, -0.4583555508459725147 ) ) ;
#7265 = CARTESIAN_POINT ( 'NONE',  ( 0.1334932820914363771, -0.9851919633086514416, 0.5193490242086087338 ) ) ;
#7266 = ORIENTED_EDGE ( 'NONE', *, *, #37914, .F. ) ;
#7267 = ORIENTED_EDGE ( 'NONE', *, *, #10628, .T. ) ;
#7268 = CARTESIAN_POINT ( 'NONE',  ( 0.05999999999999990757, 0.5878163732725504298, -0.1704268771689479434 ) ) ;
#7269 = CARTESIAN_POINT ( 'NONE',  ( 0.1153666297353847375, -0.4471033958673064079, 0.1626010152724407243 ) ) ;
#7270 = CARTESIAN_POINT ( 'NONE',  ( -0.04947837552028722108, 0.2513950290986471381, -0.4056869761633373206 ) ) ;
#7271 = DIRECTION ( 'NONE',  ( 1.000000000000000000, -0.000000000000000000, -0.000000000000000000 ) ) ;
#7272 = AXIS2_PLACEMENT_3D ( 'NONE', #20958, #23242, #32871 ) ;
#7273 = EDGE_CURVE ( 'NONE', #8761, #15212, #40608, .T. ) ;
#7274 = CARTESIAN_POINT ( 'NONE',  ( -0.05464101615137773038, -2.626773565144302935, -0.2726934094652516127 ) ) ;
#7275 = VECTOR ( 'NONE', #34343, 39.37007874015748143 ) ;
#7276 = CARTESIAN_POINT ( 'NONE',  ( 0.000000000000000000, -0.4700000000000001954, 0.000000000000000000 ) ) ;
#7277 = CARTESIAN_POINT ( 'NONE',  ( 0.4241633753480167357, -0.9987333192354345135, 0.7764642562231158784 ) ) ;
#7278 = AXIS2_PLACEMENT_3D ( 'NONE', #13297, #37990, #25868 ) ;
#7279 = CARTESIAN_POINT ( 'NONE',  ( 0.4079890870890051091, -1.708188938037489502, -0.6405138877632798877 ) ) ;
#7280 = DIRECTION ( 'NONE',  ( -1.416619696839556283E-11, 0.5877852522924840173, 0.8090169943749395687 ) ) ;
#7281 = VECTOR ( 'NONE', #8570, 39.37007874015748854 ) ;
#7282 = CARTESIAN_POINT ( 'NONE',  ( 0.02881195911414656183, 0.4889334074056470580, -0.09563129189200189617 ) ) ;
#7283 = CARTESIAN_POINT ( 'NONE',  ( 0.5190464946628291498, -1.673342222487466779, -0.5944019783408716062 ) ) ;
#7284 = ORIENTED_EDGE ( 'NONE', *, *, #36892, .T. ) ;
#7285 = CARTESIAN_POINT ( 'NONE',  ( 0.2826350996111168246, -0.9783784622179060309, 0.7275809683755095625 ) ) ;
#7286 = CARTESIAN_POINT ( 'NONE',  ( 0.04155248107635906019, -0.2901916982059698502, 0.3701002694350353228 ) ) ;
#7287 = CYLINDRICAL_SURFACE ( 'NONE', #33086, 0.1749999999999999889 ) ;
#7288 = ORIENTED_EDGE ( 'NONE', *, *, #2259, .T. ) ;
#7289 = DIRECTION ( 'NONE',  ( -1.000000000000000000, -0.000000000000000000, -0.000000000000000000 ) ) ;
#7290 = DIRECTION ( 'NONE',  ( -1.000000000000000000, -2.280301054154495132E-31, 1.664003471950577689E-31 ) ) ;
#7291 = DIRECTION ( 'NONE',  ( 0.000000000000000000, 0.000000000000000000, 1.000000000000000000 ) ) ;
#7292 = CARTESIAN_POINT ( 'NONE',  ( 0.3713045181390347560, -1.116680715442327942, 0.6055992876344371556 ) ) ;
#7293 = AXIS2_PLACEMENT_3D ( 'NONE', #33640, #24819, #30770 ) ;
#7294 = DIMENSIONAL_EXPONENTS ( 1.000000000000000000, 0.000000000000000000, 0.000000000000000000, 0.000000000000000000, 0.000000000000000000, 0.000000000000000000, 0.000000000000000000 ) ;
#7295 = CARTESIAN_POINT ( 'NONE',  ( 0.2445499268847527441, -1.256775376714664549, 0.7081412490047852559 ) ) ;
#7296 = ORIENTED_EDGE ( 'NONE', *, *, #11295, .F. ) ;
#7297 = CARTESIAN_POINT ( 'NONE',  ( -0.1683849832494421772, 0.4901165368553623281, 0.3263506530379017834 ) ) ;
#7298 = DIRECTION ( 'NONE',  ( -1.000000000000000000, -2.341930812374887555E-31, 1.664003471950578127E-31 ) ) ;
#7299 = CARTESIAN_POINT ( 'NONE',  ( 0.4826365958783261356, -1.664573153218981361, 0.5561147440369655914 ) ) ;
#7300 = CARTESIAN_POINT ( 'NONE',  ( 0.2914323826288400254, -1.233685883474753497, -0.5166151207188711680 ) ) ;
#7301 = CARTESIAN_POINT ( 'NONE',  ( 0.3776575240040908610, -1.119978095218312708, 0.7246888332089733709 ) ) ;
#7302 = AXIS2_PLACEMENT_3D ( 'NONE', #22864, #7172, #859 ) ;
#7303 = CARTESIAN_POINT ( 'NONE',  ( 0.2615233978049238406, -1.678084768816710648, 0.5373352594323992371 ) ) ;
#7304 = B_SPLINE_CURVE_WITH_KNOTS ( 'NONE', 3,
 ( #3887, #3490, #28596, #29199, #6369, #653, #468, #12965, #38045, #22430, #38454, #25097, #7163, #38239, #35174, #10289 ),
 .UNSPECIFIED., .F., .F.,
 ( 4, 2, 2, 2, 2, 2, 2, 4 ),
 ( 0.000000000000000000, 0.0004934348547721647844, 0.0009868697095443295687, 0.001480304564316494570, 0.001973739419088659137, 0.002467174273860823705, 0.002960609128632989140, 0.003947478838177317408 ),
 .UNSPECIFIED. ) ;
#7305 = CARTESIAN_POINT ( 'NONE',  ( 0.5741821450848180186, -1.541683553717290600, -0.4860598978662519221 ) ) ;
#7306 = ORIENTED_EDGE ( 'NONE', *, *, #15369, .T. ) ;
#7307 = COORDINATED_UNIVERSAL_TIME_OFFSET ( 0, 0, .AHEAD. ) ;
#7308 = CARTESIAN_POINT ( 'NONE',  ( -0.02000000000000000042, -2.067054404790649613, -0.8080442508481435748 ) ) ;
#7309 = ORIENTED_EDGE ( 'NONE', *, *, #24826, .F. ) ;
#7310 = AXIS2_PLACEMENT_3D ( 'NONE', #3145, #34801, #18983 ) ;
#7311 = CARTESIAN_POINT ( 'NONE',  ( 0.4136164036920929599, -1.589545870387133908, 0.5737237853280422462 ) ) ;
#7313 = CARTESIAN_POINT ( 'NONE',  ( 0.2017021523379468051, -0.6567308881480256044, 0.3367814055878157187 ) ) ;
#7312 = CARTESIAN_POINT ( 'NONE',  ( 0.06625991551443329020, -0.7353711572464834978, 0.005698596487343925848 ) ) ;
#7314 = FACE_OUTER_BOUND ( 'NONE', #1704, .T. ) ;
#7315 = EDGE_LOOP ( 'NONE', ( #13245, #3189, #33725, #30858 ) ) ;
#7316 = ORIENTED_EDGE ( 'NONE', *, *, #37029, .F. ) ;
#7317 = LINE ( 'NONE', #23202, #15574 ) ;
#7318 = CARTESIAN_POINT ( 'NONE',  ( 0.5711473416986291296, -1.490055735821753435, 0.6671231403163234708 ) ) ;
#7319 = VERTEX_POINT ( 'NONE', #2767 ) ;
#7320 = CARTESIAN_POINT ( 'NONE',  ( 0.07344419321621749319, -1.332345885986941036, 0.4917313231282066655 ) ) ;
#7321 = CARTESIAN_POINT ( 'NONE',  ( 0.04229974373173647079, -0.4430055847546718328, 0.1530238331097731330 ) ) ;
#7322 = CYLINDRICAL_SURFACE ( 'NONE', #34280, 0.04330708661417322775 ) ;
#7323 = ORIENTED_EDGE ( 'NONE', *, *, #29833, .F. ) ;
#7324 = CARTESIAN_POINT ( 'NONE',  ( 0.4093192649698303431, -1.477391824278450061, -0.5625509170971494388 ) ) ;
#7325 = DIRECTION ( 'NONE',  ( 0.000000000000000000, 0.000000000000000000, -1.000000000000000000 ) ) ;
#7326 = SPHERICAL_SURFACE ( 'NONE', #40427, 0.01499999999999999944 ) ;
#7327 = CARTESIAN_POINT ( 'NONE',  ( 0.7437969124434082868, -1.515212563166708604, 0.5942788597236812187 ) ) ;
#7328 = CARTESIAN_POINT ( 'NONE',  ( 0.3896220963715341101, -1.743012515435767407, -0.7180593106334604014 ) ) ;
#7329 = CARTESIAN_POINT ( 'NONE',  ( 0.06805471781164178224, -1.337523778089659610, 0.5185330071074899516 ) ) ;
#7330 = DIRECTION ( 'NONE',  ( 0.8660512985181132439, 0.4999551463232376203, 0.000000000000000000 ) ) ;
#7331 = APPROVAL_STATUS ( 'not_yet_approved' ) ;
#7332 = CIRCLE ( 'NONE', #34313, 0.01500000000000001159 ) ;
#7333 = CARTESIAN_POINT ( 'NONE',  ( 0.6246939234061054114, -1.524535107703195003, -0.6328271379228022075 ) ) ;
#7334 = CARTESIAN_POINT ( 'NONE',  ( 0.03170953572518896840, 0.2433677181033278847, 0.4274019581173342242 ) ) ;
#7335 = CARTESIAN_POINT ( 'NONE',  ( 0.1843448470596803501, -0.5982784986119861204, -0.009472559150814239756 ) ) ;
#7336 = DIRECTION ( 'NONE',  ( -0.3961231183188304583, -5.551115123125781470E-17, -0.9181974053183585838 ) ) ;
#7337 = CARTESIAN_POINT ( 'NONE',  ( 0.1394132134375135335, -1.285647836448881698, 0.4252245862416944577 ) ) ;
#7338 = ADVANCED_BREP_SHAPE_REPRESENTATION ( '', ( #4819, #27819 ), #33713 ) ;
#7339 = AXIS2_PLACEMENT_3D ( 'NONE', #25772, #17103, #14010 ) ;
#7340 = AXIS2_PLACEMENT_3D ( 'NONE', #33712, #14187, #14581 ) ;
#7341 = CARTESIAN_POINT ( 'NONE',  ( 0.2922741047311901985, -1.688215408676643658, 0.8015225518757634893 ) ) ;
#7342 = CARTESIAN_POINT ( 'NONE',  ( 0.5693027582541522191, -1.577552960580653307, -0.4686421343491008473 ) ) ;
#7343 = VECTOR ( 'NONE', #12850, 39.37007874015748143 ) ;
#7344 = CARTESIAN_POINT ( 'NONE',  ( -0.2043922129835736845, -0.5166151207188713901, 0.3749999999999999445 ) ) ;
#7345 = DIRECTION ( 'NONE',  ( -1.000000000000000000, -2.280301054154495132E-31, 1.664003471950577689E-31 ) ) ;
#7346 = CARTESIAN_POINT ( 'NONE',  ( 0.1993688661005383334, -1.286831035182783634, -0.2901530652563581447 ) ) ;
#7347 = ORIENTED_EDGE ( 'NONE', *, *, #16129, .F. ) ;
#7348 = ORIENTED_EDGE ( 'NONE', *, *, #34780, .F. ) ;
#7349 = CARTESIAN_POINT ( 'NONE',  ( 0.05567535398968421340, -1.335339640988971288, 0.4687417262808780127 ) ) ;
#7350 = ORIENTED_EDGE ( 'NONE', *, *, #13486, .F. ) ;
#7351 = CARTESIAN_POINT ( 'NONE',  ( 0.3862110256088818194, -1.731934476144515900, 0.4282538419479027247 ) ) ;
#7352 = FACE_OUTER_BOUND ( 'NONE', #4332, .T. ) ;
#7353 = CARTESIAN_POINT ( 'NONE',  ( 0.3894655533085423782, -1.132081281638208647, 0.7727388183733103766 ) ) ;
#7355 = ORIENTED_EDGE ( 'NONE', *, *, #3684, .F. ) ;
#7354 = CARTESIAN_POINT ( 'NONE',  ( 0.08978098643734212791, -7.789101598130604663E-17, -0.3698489655877988391 ) ) ;
#7356 = CARTESIAN_POINT ( 'NONE',  ( 0.3725907112986628911, -0.9732892004818366471, 0.6614114956809742374 ) ) ;
#7357 = ADVANCED_FACE ( 'NONE', ( #8936 ), #2732, .T. ) ;
#7358 = DIRECTION ( 'NONE',  ( 0.000000000000000000, 0.000000000000000000, -1.000000000000000000 ) ) ;
#7359 = ORIENTED_EDGE ( 'NONE', *, *, #26983, .T. ) ;
#7360 = DIRECTION ( 'NONE',  ( -0.000000000000000000, 0.8090169943749540016, 0.5877852522924639223 ) ) ;
#7361 = ADVANCED_FACE ( 'NONE', ( #34226 ), #3172, .F. ) ;
#7362 = ORIENTED_EDGE ( 'NONE', *, *, #31902, .T. ) ;
#7363 = CARTESIAN_POINT ( 'NONE',  ( 0.3264869902747437047, -1.638973361554033170, 0.5665452580153856887 ) ) ;
#7365 = CARTESIAN_POINT ( 'NONE',  ( 0.1129301055607959681, -0.7190106171137882196, -0.09375086704596295728 ) ) ;
#7364 = CARTESIAN_POINT ( 'NONE',  ( 0.6355551670791450558, -1.580035597652303281, 0.4260930208334881564 ) ) ;
#7366 = DIRECTION ( 'NONE',  ( -1.000000000000000000, -0.000000000000000000, -0.000000000000000000 ) ) ;
#7367 = EDGE_CURVE ( 'NONE', #23493, #12543, #25735, .T. ) ;
#7368 = CIRCLE ( 'NONE', #29085, 0.1700000000000000400 ) ;
#7369 = CARTESIAN_POINT ( 'NONE',  ( 0.01299436802863446032, -1.701590229751596572, -0.3397165561182163285 ) ) ;
#7370 = ORIENTED_EDGE ( 'NONE', *, *, #15151, .F. ) ;
#7371 = EDGE_CURVE ( 'NONE', #13497, #29847, #26955, .T. ) ;
#7372 = FACE_OUTER_BOUND ( 'NONE', #16441, .T. ) ;
#7373 = CARTESIAN_POINT ( 'NONE',  ( 0.1113455598878015373, -0.9288604395749201492, 0.1798995508551040623 ) ) ;
#7374 = LINE ( 'NONE', #16268, #18018 ) ;
#7375 = CARTESIAN_POINT ( 'NONE',  ( 0.7009661026058806588, -1.563056106223301045, -0.5155029497116575543 ) ) ;
#7376 = CIRCLE ( 'NONE', #23155, 0.06250000000000001388 ) ;
#7377 = CARTESIAN_POINT ( 'NONE',  ( 0.3287827152071736703, -1.178255865141498271, 0.7250580491420484108 ) ) ;
#7378 = CARTESIAN_POINT ( 'NONE',  ( 0.08525625553564522563, -0.9707879525957265887, 0.8108029995381474953 ) ) ;
#7379 = CIRCLE ( 'NONE', #30394, 0.03000000000000005440 ) ;
#7380 = CARTESIAN_POINT ( 'NONE',  ( 0.4656188692126475015, -1.154221074868963415, 0.4228768485321867665 ) ) ;
#7381 = CARTESIAN_POINT ( 'NONE',  ( -0.1699622337672930805, 0.4951791062278213529, 0.3187362200132102807 ) ) ;
#7382 = CARTESIAN_POINT ( 'NONE',  ( -0.2399999999999999079, -2.853330612949663170, -0.6088139570729240724 ) ) ;
#7383 = CARTESIAN_POINT ( 'NONE',  ( -0.1969433606228570832, 0.5138636982738132852, 0.3750000000000001110 ) ) ;
#7384 = CIRCLE ( 'NONE', #30399, 0.03000000000000022787 ) ;
#7385 = EDGE_CURVE ( 'NONE', #38442, #13009, #24972, .T. ) ;
#7386 = CARTESIAN_POINT ( 'NONE',  ( -0.2399999999999999079, -1.835749455202394298, -0.2938319975228648739 ) ) ;
#7387 = DIRECTION ( 'NONE',  ( 1.000000000000000000, 1.169383359989550442E-31, -7.771561172376108602E-16 ) ) ;
#7388 = APPROVAL_STATUS ( 'not_yet_approved' ) ;
#7389 = APPLIED_PERSON_AND_ORGANIZATION_ASSIGNMENT ( #27263, #12019, ( #30575 ) ) ;
#7390 = FACE_OUTER_BOUND ( 'NONE', #40150, .T. ) ;
#7391 = CARTESIAN_POINT ( 'NONE',  ( 0.1890382415369475377, -1.253790046906361422, -0.3976186731358027915 ) ) ;
#7392 = CARTESIAN_POINT ( 'NONE',  ( 0.2332815142676702147, -1.595247443236931462, -0.6698052276397686855 ) ) ;
#7393 = CARTESIAN_POINT ( 'NONE',  ( -0.02000000000000000042, -1.599201040860868339, 0.1642182323853691728 ) ) ;
#7394 = CARTESIAN_POINT ( 'NONE',  ( 0.3783141089212034291, -1.720060367475409135, -0.4893959057094034448 ) ) ;
#7395 = VECTOR ( 'NONE', #12118, 39.37007874015748854 ) ;
#7396 = DIRECTION ( 'NONE',  ( 1.000000000000000000, 1.443840457432242888E-15, -8.250516899612815800E-16 ) ) ;
#7397 = DIRECTION ( 'NONE',  ( 1.702140497302371910E-12, 0.5877852522924655876, -0.8090169943749527803 ) ) ;
#7398 = CIRCLE ( 'NONE', #30425, 0.5302738246768103902 ) ;
#7399 = ORIENTED_EDGE ( 'NONE', *, *, #3993, .T. ) ;
#7400 = ORIENTED_EDGE ( 'NONE', *, *, #23306, .T. ) ;
#7401 = CARTESIAN_POINT ( 'NONE',  ( -0.02000000000000000042, -2.551729310907437043, -0.5086726180052709712 ) ) ;
#7402 = ORIENTED_EDGE ( 'NONE', *, *, #29814, .T. ) ;
#7403 = CARTESIAN_POINT ( 'NONE',  ( 0.2687115422113643959, -1.674045828432256355, 0.5754129880667321340 ) ) ;
#7404 = VECTOR ( 'NONE', #3299, 39.37007874015748854 ) ;
#7405 = CARTESIAN_POINT ( 'NONE',  ( 0.6020297351734736901, -1.483137940370031327, 0.5741727644973939615 ) ) ;
#7407 = EDGE_LOOP ( 'NONE', ( #40462, #40090, #24567, #1969 ) ) ;
#7406 = DIRECTION ( 'NONE',  ( -1.000000000000000000, -2.276539994720197063E-15, 5.691349986800492658E-16 ) ) ;
#7408 = VECTOR ( 'NONE', #20020, 39.37007874015748143 ) ;
#7410 = EDGE_LOOP ( 'NONE', ( #5544, #23731, #37068 ) ) ;
#7409 = EDGE_LOOP ( 'NONE', ( #35700, #11546, #38204, #30505 ) ) ;
#7411 = CARTESIAN_POINT ( 'NONE',  ( 0.2010011132812319357, -0.7031246823302816917, 0.6588550337264904577 ) ) ;
#7412 = EDGE_CURVE ( 'NONE', #34185, #20959, #3361, .T. ) ;
#7413 = ORIENTED_EDGE ( 'NONE', *, *, #16964, .T. ) ;
#7414 = CARTESIAN_POINT ( 'NONE',  ( -0.01277482466110092980, -0.5582999514612219105, 0.2804546619028133181 ) ) ;
#7415 = CARTESIAN_POINT ( 'NONE',  ( 0.5328454728509273153, -1.654335657659062653, -0.4959994330086620051 ) ) ;
#7416 = CARTESIAN_POINT ( 'NONE',  ( 0.6297115083997322227, -1.615736705109999782, -0.4933022779381483480 ) ) ;
#7417 = PERSON_AND_ORGANIZATION_ROLE ( 'classification_officer' ) ;
#7418 = EDGE_CURVE ( 'NONE', #34759, #27340, #11185, .T. ) ;
#7419 = CARTESIAN_POINT ( 'NONE',  ( -0.004891214258241028887, -0.7404579356088991648, 0.1483282180229323066 ) ) ;
#7421 = VERTEX_POINT ( 'NONE', #15714 ) ;
#7420 = ORIENTED_EDGE ( 'NONE', *, *, #38297, .F. ) ;
#7422 = EDGE_CURVE ( 'NONE', #23907, #3591, #28260, .T. ) ;
#7423 = CARTESIAN_POINT ( 'NONE',  ( 0.2109547519922409242, -0.9305643203978569700, 0.6267875559574144217 ) ) ;
#7424 = APPLICATION_CONTEXT ( 'configuration controlled 3d designs of mechanical parts and assemblies' ) ;
#7425 = B_SPLINE_CURVE_WITH_KNOTS ( 'NONE', 3,
 ( #39617, #17212, #14126, #30168, #32645, #20721 ),
 .UNSPECIFIED., .F., .F.,
 ( 4, 2, 4 ),
 ( 0.002514931666163710763, 0.002746441579761122430, 0.002977951493358533663 ),
 .UNSPECIFIED. ) ;
#7426 = CARTESIAN_POINT ( 'NONE',  ( 0.1499999999999989120, -0.3772621329472692908, -0.3651003739303438911 ) ) ;
#7427 =( BOUNDED_SURFACE ( )  B_SPLINE_SURFACE ( 3, 2, ( 
 ( #8511, #27260, #36899 ),
 ( #39789, #8709, #17769 ),
 ( #11406, #34212, #24575 ),
 ( #37304, #30537, #20888 ),
 ( #31149, #11804, #15516 ),
 ( #2156, #17978, #21285 ),
 ( #2557, #30735, #2362 ),
 ( #40397, #5412, #5219 ),
 ( #14692, #30322, #8318 ),
 ( #11620, #18185, #34018 ),
 ( #24178, #33827, #36703 ),
 ( #23974, #15092, #14900 ),
 ( #27459, #15303, #39982 ),
 ( #30928, #40179, #18594 ),
 ( #12016, #28067, #37108 ),
 ( #8926, #21500, #36507 ) ),
 .UNSPECIFIED., .F., .F., .T. ) 
 B_SPLINE_SURFACE_WITH_KNOTS ( ( 4, 2, 2, 2, 2, 2, 2, 4 ),
 ( 3, 3 ),
 ( -2.352153712789272500E-05, 0.0004694506785108612111, 0.0009624228941496151303, 0.001455395109788369104, 0.001948367325427123077, 0.002441339541065876834, 0.002934311756704631024, 0.003920256187982138971 ),
 ( 0.000000000000000000, 1.000000000000000000 ),
 .UNSPECIFIED. ) 
 GEOMETRIC_REPRESENTATION_ITEM ( )  RATIONAL_B_SPLINE_SURFACE ( (
 ( 1.000000000000000000, 0.7057019905713519670, 1.000000000000000000),
 ( 1.000000000000000000, 0.7055894858937867831, 1.000000000000000000),
 ( 1.000000000000000000, 0.7055144135113683435, 1.000000000000000000),
 ( 1.000000000000000000, 0.7054271390702308020, 1.000000000000000000),
 ( 1.000000000000000000, 0.7054151093076957979, 1.000000000000000000),
 ( 1.000000000000000000, 0.7054386977650431989, 1.000000000000000000),
 ( 1.000000000000000000, 0.7054733622895101863, 1.000000000000000000),
 ( 1.000000000000000000, 0.7055688516086890960, 1.000000000000000000),
 ( 1.000000000000000000, 0.7056302112408742166, 1.000000000000000000),
 ( 1.000000000000000000, 0.7057581921034653538, 1.000000000000000000),
 ( 1.000000000000000000, 0.7058253497257075404, 1.000000000000000000),
 ( 1.000000000000000000, 0.7059550172059571027, 1.000000000000000000),
 ( 1.000000000000000000, 0.7060161488338141389, 1.000000000000000000),
 ( 1.000000000000000000, 0.7061761676825132339, 1.000000000000000000),
 ( 1.000000000000000000, 0.7062536236208033502, 1.000000000000000000),
 ( 1.000000000000000000, 0.7062849495007524903, 1.000000000000000000) ) ) 
 REPRESENTATION_ITEM ( '' )  SURFACE ( )  );
#7428 = CARTESIAN_POINT ( 'NONE',  ( 0.1104829199723380839, -0.5612026451200987642, 0.2208380843409518401 ) ) ;
#7429 = ORIENTED_EDGE ( 'NONE', *, *, #27753, .T. ) ;
#7430 = CARTESIAN_POINT ( 'NONE',  ( 0.03113248654051816583, 0.000000000000000000, 0.2000000000000000111 ) ) ;
#7431 = CARTESIAN_POINT ( 'NONE',  ( 0.2038749045098602886, -1.364881829950852721, 0.4182417262808790226 ) ) ;
#7432 = DIRECTION ( 'NONE',  ( 0.8660512985181135770, 0.4999551463232370652, 0.000000000000000000 ) ) ;
#7433 = CIRCLE ( 'NONE', #12701, 0.9087847906030154244 ) ;
#7434 = B_SPLINE_CURVE_WITH_KNOTS ( 'NONE', 3,
 ( #23122, #13040, #26400, #19621 ),
 .UNSPECIFIED., .F., .F.,
 ( 4, 4 ),
 ( 0.001505104451090290719, 0.001946516628694922859 ),
 .UNSPECIFIED. ) ;
#7435 = CARTESIAN_POINT ( 'NONE',  ( 0.3473585933147235738, -1.744357246013940044, 0.5876618537173693424 ) ) ;
#7436 = CARTESIAN_POINT ( 'NONE',  ( 0.6928118984338402786, -1.426853195981605316, 0.5961107746216205427 ) ) ;
#7437 = DIRECTION ( 'NONE',  ( -0.8660254037844407060, 0.2890674114961861441, -0.4079706259167332760 ) ) ;
#7438 = CIRCLE ( 'NONE', #30449, 0.6443128707267505861 ) ;
#7439 = DIRECTION ( 'NONE',  ( 0.9549552564275718414, 0.000000000000000000, 0.2967498242987692270 ) ) ;
#7440 = CARTESIAN_POINT ( 'NONE',  ( 0.3999999999981719290, -2.080276347128062753, -0.2651857657968351156 ) ) ;
#7441 = VECTOR ( 'NONE', #39039, 39.37007874015748143 ) ;
#7442 = CARTESIAN_POINT ( 'NONE',  ( -0.0002026554222459760483, -0.8535802774609255739, -0.04061330533372662505 ) ) ;
#7443 = ADVANCED_FACE ( 'NONE', ( #25596 ), #16442, .T. ) ;
#7444 = DIRECTION ( 'NONE',  ( 1.000000000000000000, 6.779273404243070203E-32, 4.314083075427408311E-32 ) ) ;
#7445 = CARTESIAN_POINT ( 'NONE',  ( -0.08000000000000000167, -1.758704040287259573, -0.8825853814972599576 ) ) ;
#7446 = CARTESIAN_POINT ( 'NONE',  ( 0.4795062484387999646, -1.112529643762525611, -0.4042499308301856220 ) ) ;
#7447 = CARTESIAN_POINT ( 'NONE',  ( -0.002083146443013344888, -0.8967360763018595859, 0.09758087637170891060 ) ) ;
#7448 = VECTOR ( 'NONE', #27974, 39.37007874015748143 ) ;
#7449 = CARTESIAN_POINT ( 'NONE',  ( 0.3960970180006803121, -1.016137033769514808, 0.6457357589753065508 ) ) ;
#7450 = PERSON_AND_ORGANIZATION ( #28500, #32463 ) ;
#7451 = AXIS2_PLACEMENT_3D ( 'NONE', #37329, #28842, #21921 ) ;
#7452 = CARTESIAN_POINT ( 'NONE',  ( -0.01895494625228186930, 0.4667936258712436226, -0.2292799240428185781 ) ) ;
#7453 = DIRECTION ( 'NONE',  ( 1.000000000000000000, 0.000000000000000000, 0.000000000000000000 ) ) ;
#7454 = ORIENTED_EDGE ( 'NONE', *, *, #23993, .F. ) ;
#7455 = CYLINDRICAL_SURFACE ( 'NONE', #33577, 0.04000000000000000777 ) ;
#7456 = CARTESIAN_POINT ( 'NONE',  ( 0.002465946970083897002, -0.5375442681548233681, 0.2095628591970551957 ) ) ;
#7457 = AXIS2_PLACEMENT_3D ( 'NONE', #648, #29399, #10281 ) ;
#7458 = CARTESIAN_POINT ( 'NONE',  ( 0.3790996791422692747, -1.751796687822255949, 0.5182417262812423209 ) ) ;
#7459 = ORIENTED_EDGE ( 'NONE', *, *, #38310, .T. ) ;
#7460 = DIRECTION ( 'NONE',  ( 0.000000000000000000, 0.8438867430782092116, 0.5365213554527465956 ) ) ;
#7461 = CARTESIAN_POINT ( 'NONE',  ( 0.6326847266287998206, -1.322366380368365180, 0.7606069447649664861 ) ) ;
#7463 = ORIENTED_EDGE ( 'NONE', *, *, #17439, .F. ) ;
#7462 = ORIENTED_EDGE ( 'NONE', *, *, #8783, .T. ) ;
#7464 = AXIS2_PLACEMENT_3D ( 'NONE', #39249, #17835, #35962 ) ;
#7465 = EDGE_CURVE ( 'NONE', #15823, #26063, #19160, .T. ) ;
#7466 = AXIS2_PLACEMENT_3D ( 'NONE', #8507, #21281, #2747 ) ;
#7467 = CARTESIAN_POINT ( 'NONE',  ( -0.1743922129835729085, -0.5166151207188712791, 0.3599999999999990430 ) ) ;
#7468 = CARTESIAN_POINT ( 'NONE',  ( 0.4496398668279690813, -1.226616743782979135, 0.5966018278806392017 ) ) ;
#7469 = EDGE_CURVE ( 'NONE', #2400, #29368, #23707, .T. ) ;
#7470 = CARTESIAN_POINT ( 'NONE',  ( -0.02238765564325672849, 0.5044129532808436789, -0.09031612285224611958 ) ) ;
#7471 = ORIENTED_EDGE ( 'NONE', *, *, #20365, .T. ) ;
#7472 = CARTESIAN_POINT ( 'NONE',  ( 0.4582297113153581125, -1.232395013690232632, 1.043719859503123404 ) ) ;
#7473 = CARTESIAN_POINT ( 'NONE',  ( 0.1819313570110824285, -0.8286255242310253122, 0.6065153366566046200 ) ) ;
#7474 = CIRCLE ( 'NONE', #12749, 0.01499999999999999424 ) ;
#7475 = CARTESIAN_POINT ( 'NONE',  ( 0.09745522806139698957, -0.8755261795257442969, 0.8646684577488064072 ) ) ;
#7476 = CARTESIAN_POINT ( 'NONE',  ( 0.4073001593474919746, -1.370116077848211766, 0.8465991415876540360 ) ) ;
#7477 = AXIS2_PLACEMENT_3D ( 'NONE', #1668, #32890, #10488 ) ;
#7479 = DIRECTION ( 'NONE',  ( 0.8660512985181133550, 0.4999551463232370652, 0.000000000000000000 ) ) ;
#7478 = CARTESIAN_POINT ( 'NONE',  ( 0.1061776879072938579, -1.071297230844371340, 0.8824484360082986978 ) ) ;
#7480 = CARTESIAN_POINT ( 'NONE',  ( 0.3452606047117887655, -1.113321646336553394, 0.6365754745706553308 ) ) ;
#7481 = ORIENTED_EDGE ( 'NONE', *, *, #7022, .F. ) ;
#7482 = ORIENTED_EDGE ( 'NONE', *, *, #25745, .T. ) ;
#7483 = CARTESIAN_POINT ( 'NONE',  ( 0.3339310430327372403, -1.636299247267255286, 0.5510156998079677182 ) ) ;
#7484 = CARTESIAN_POINT ( 'NONE',  ( 0.1173700203642584067, -0.4709408336746424562, 0.2678698260706097178 ) ) ;
#7485 = DIRECTION ( 'NONE',  ( 1.000000000000000000, 0.000000000000000000, 0.000000000000000000 ) ) ;
#7486 = CARTESIAN_POINT ( 'NONE',  ( -0.03171102739523436881, -0.4816844162602763602, -0.09938404130288475136 ) ) ;
#7487 = ADVANCED_FACE ( 'NONE', ( #3362, #25403 ), #24798, .F. ) ;
#7488 = VECTOR ( 'NONE', #3980, 39.37007874015748143 ) ;
#7489 = DIRECTION ( 'NONE',  ( 0.000000000000000000, 0.000000000000000000, -1.000000000000000000 ) ) ;
#7490 = EDGE_CURVE ( 'NONE', #19496, #14090, #28680, .T. ) ;
#7491 = CARTESIAN_POINT ( 'NONE',  ( 0.08989780363036058153, -0.5646359461869331353, 0.1460065308160271857 ) ) ;
#7492 = CARTESIAN_POINT ( 'NONE',  ( 0.5890075386511577360, -1.247786712317649815, 0.6995832148063678702 ) ) ;
#7493 = AXIS2_PLACEMENT_3D ( 'NONE', #19820, #29686, #14254 ) ;
#7494 = AXIS2_PLACEMENT_3D ( 'NONE', #33027, #17401, #10612 ) ;
#7495 = CARTESIAN_POINT ( 'NONE',  ( 0.4911277369064176446, -1.657269195667506967, 0.4283731361201775223 ) ) ;
#7496 = CYLINDRICAL_SURFACE ( 'NONE', #39593, 0.01500000000000004281 ) ;
#7497 = AXIS2_PLACEMENT_3D ( 'NONE', #12370, #34587, #24926 ) ;
#7498 = CARTESIAN_POINT ( 'NONE',  ( 0.04946288932099741908, 0.4418470831553572564, -0.1805342557390068048 ) ) ;
#7499 = CARTESIAN_POINT ( 'NONE',  ( 0.4186432780919984720, -1.612034538517055360, -0.6668481824684697745 ) ) ;
#7500 = ORIENTED_EDGE ( 'NONE', *, *, #32417, .T. ) ;
#7501 = CARTESIAN_POINT ( 'NONE',  ( 0.3511827046531754148, -1.077246269942499612, 0.7624202803643029824 ) ) ;
#7502 = CARTESIAN_POINT ( 'NONE',  ( 0.03662792686184382362, -0.2484399233013401542, 0.4119056456069884464 ) ) ;
#7503 = AXIS2_PLACEMENT_3D ( 'NONE', #10134, #31945, #25782 ) ;
#7504 = CARTESIAN_POINT ( 'NONE',  ( -0.04211471441534227894, -0.2686849334112374477, -0.3844466239331229551 ) ) ;
#7505 = VECTOR ( 'NONE', #25493, 39.37007874015748143 ) ;
#7506 = VERTEX_POINT ( 'NONE', #35443 ) ;
#7507 = FACE_OUTER_BOUND ( 'NONE', #5724, .T. ) ;
#7508 = ORIENTED_EDGE ( 'NONE', *, *, #27330, .T. ) ;
#7509 = DIRECTION ( 'NONE',  ( 0.000000000000000000, 0.000000000000000000, -1.000000000000000000 ) ) ;
#7510 = CARTESIAN_POINT ( 'NONE',  ( -0.2399999999999999079, -2.183180860297908144, -0.4937760292030871079 ) ) ;
#7511 = B_SPLINE_CURVE_WITH_KNOTS ( 'NONE', 3,
 ( #39980, #21283, #18378, #21680, #27457, #30534 ),
 .UNSPECIFIED., .F., .F.,
 ( 4, 2, 4 ),
 ( 0.001203677602004720381, 0.004507238951556864770, 0.007810800301109012411 ),
 .UNSPECIFIED. ) ;
#7512 = CARTESIAN_POINT ( 'NONE',  ( 0.4026621603086822931, -1.135280432806801132, 0.5010831896812795172 ) ) ;
#7513 = CARTESIAN_POINT ( 'NONE',  ( 0.07424435375522935032, -0.8686257631445842842, 0.4612673976281420618 ) ) ;
#7514 = EDGE_LOOP ( 'NONE', ( #29722, #13679, #18682, #14396, #10457, #25759, #15544, #36176, #19896, #30506, #1007, #36866 ) ) ;
#7515 = DIRECTION ( 'NONE',  ( 0.8013552086938348085, 0.4626073089491885559, 0.3792417529835693801 ) ) ;
#7516 = CARTESIAN_POINT ( 'NONE',  ( -0.05464101615137763324, -2.183180860297908144, -0.4937760292030871079 ) ) ;
#7517 = CARTESIAN_POINT ( 'NONE',  ( 0.4227944218364425577, -1.670731094902153213, -0.6342269662369710570 ) ) ;
#7518 = CARTESIAN_POINT ( 'NONE',  ( -0.02000000000000000042, -1.802948570736253586, -0.8420585814095631338 ) ) ;
#7519 = CIRCLE ( 'NONE', #37777, 0.1249999999999999584 ) ;
#7520 = CARTESIAN_POINT ( 'NONE',  ( 0.3640235822487147832, -1.104155517840267775, 0.7181720340464149421 ) ) ;
#7521 = ADVANCED_FACE ( 'NONE', ( #731 ), #22516, .T. ) ;
#7523 = CARTESIAN_POINT ( 'NONE',  ( 0.2648760513428040086, -1.303909466691514973, 0.5182417262812423209 ) ) ;
#7522 = CYLINDRICAL_SURFACE ( 'NONE', #12776, 2.001674066779348227 ) ;
#7524 = CARTESIAN_POINT ( 'NONE',  ( 0.5777362523500105818, -1.534599504986668084, -0.5616871023379128580 ) ) ;
#7525 = ORIENTED_EDGE ( 'NONE', *, *, #20483, .F. ) ;
#7526 = CIRCLE ( 'NONE', #12800, 0.07749999999977547072 ) ;
#7527 = DIRECTION ( 'NONE',  ( 0.000000000000000000, 0.000000000000000000, -1.000000000000000000 ) ) ;
#7528 = EDGE_LOOP ( 'NONE', ( #16645, #29863, #30407, #1852 ) ) ;
#7529 = CIRCLE ( 'NONE', #12127, 0.2000000000000000666 ) ;
#7530 = ORIENTED_EDGE ( 'NONE', *, *, #20237, .T. ) ;
#7531 = CIRCLE ( 'NONE', #27264, 0.02999999999999999195 ) ;
#7532 = CARTESIAN_POINT ( 'NONE',  ( 0.4151474250827118517, -1.589570192129442727, 0.5985126306996821910 ) ) ;
#7534 = CARTESIAN_POINT ( 'NONE',  ( 0.1947297287360276741, -0.6386476969732345355, 0.3263804930690787365 ) ) ;
#7533 = CARTESIAN_POINT ( 'NONE',  ( 0.06774469294687966714, -0.6123281028958347250, 0.01828842993687508287 ) ) ;
#7535 = CARTESIAN_POINT ( 'NONE',  ( 0.1543908734882358524, -1.277778445049856826, 0.4807399974149955679 ) ) ;
#7536 = LOCAL_TIME ( 0, 53, 7.000000000000000000, #2049 ) ;
#7537 = ORIENTED_EDGE ( 'NONE', *, *, #33934, .T. ) ;
#7538 = ORIENTED_EDGE ( 'NONE', *, *, #16685, .T. ) ;
#7539 = CARTESIAN_POINT ( 'NONE',  ( 0.02999999999997886302, -2.183180860297921466, -0.4937760292030871079 ) ) ;
#7540 = CARTESIAN_POINT ( 'NONE',  ( 0.1337456116390407512, -0.6334664691652446278, 0.3892934226950710563 ) ) ;
#7541 = ORIENTED_EDGE ( 'NONE', *, *, #38924, .T. ) ;
#7542 = AXIS2_PLACEMENT_3D ( 'NONE', #2313, #20836, #39941 ) ;
#7543 = CARTESIAN_POINT ( 'NONE',  ( 0.1874400581894105633, -0.6906950488587336734, 0.04510364496225629377 ) ) ;
#7544 = CARTESIAN_POINT ( 'NONE',  ( 0.03170953572518595692, -0.4816881781209783608, 0.09938198567066194866 ) ) ;
#7545 = CARTESIAN_POINT ( 'NONE',  ( 0.6544078563150326211, -1.544269123161558177, 0.4241055859090113733 ) ) ;
#7546 = CARTESIAN_POINT ( 'NONE',  ( 0.1668829993946232826, -1.259189101050422366, 0.4341909677000992951 ) ) ;
#7547 = CARTESIAN_POINT ( 'NONE',  ( -0.1617315581917541378, 0.4682256792068176243, 0.1178658435936995874 ) ) ;
#7548 = CARTESIAN_POINT ( 'NONE',  ( -0.2399999999999999079, -3.807157481699992907, -0.4735579732456337565 ) ) ;
#7549 = CARTESIAN_POINT ( 'NONE',  ( 0.5453389350593388363, -1.184144166247469876, 0.8773366473911075047 ) ) ;
#7550 = DIRECTION ( 'NONE',  ( 1.000000000000000000, 2.532387540469236368E-12, 8.550494110633370620E-14 ) ) ;
#7551 = CARTESIAN_POINT ( 'NONE',  ( -0.3000000000000000999, -2.768941938641841904, -0.5551618215276492574 ) ) ;
#7552 = CALENDAR_DATE ( 2026, 13, 10 ) ;
#7553 = AXIS2_PLACEMENT_3D ( 'NONE', #29819, #10685, #13764 ) ;
#7554 = EDGE_CURVE ( 'NONE', #17499, #4285, #15288, .T. ) ;
#7555 = B_SPLINE_CURVE_WITH_KNOTS ( 'NONE', 3,
 ( #852, #35178, #6981, #3891, #13574, #23041, #19942, #10474, #35566, #11501, #24065, #29810, #21162, #5290, #17854, #1848, #36591, #11285 ),
 .UNSPECIFIED., .F., .F.,
 ( 4, 2, 2, 2, 2, 2, 2, 2, 4 ),
 ( -0.002633528389679711239, -0.001975271857855709877, -0.001317015326031708514, -0.0006587587942077071518, -5.022623837057892116E-07, 0.0006577542694402955734, 0.001316010801264296936, 0.001974267333088298732, 0.002632523864912299661 ),
 .UNSPECIFIED. ) ;
#7556 = FACE_OUTER_BOUND ( 'NONE', #39316, .T. ) ;
#7557 = CIRCLE ( 'NONE', #17405, 0.01500000000000002894 ) ;
#7558 = CARTESIAN_POINT ( 'NONE',  ( 0.05634206451479729927, 0.2780979935378019574, 0.3651623763481127161 ) ) ;
#7559 = CARTESIAN_POINT ( 'NONE',  ( 0.1844024556850973051, -0.8470684581476211061, 0.09518424029853758683 ) ) ;
#7560 = CARTESIAN_POINT ( 'NONE',  ( 0.4111945703227398163, -1.245400387139686815, 0.5084384360591323038 ) ) ;
#7561 = B_SPLINE_CURVE_WITH_KNOTS ( 'NONE', 3,
 ( #5159, #33541, #24127, #36649, #5351, #17913, #12365, #24921, #21446, #2906, #37448, #22057, #25120, #33973, #18953, #3296, #9262, #15852, #5777, #9073, #19153, #18749, #21841, #37046, #34581, #28009, #31302, #6574, #21636, #25333, #28406, #6387, #18333, #37658, #15459, #31489, #34159, #40123, #276, #31694, #3513, #12771, #22256, #27594, #37873, #11953, #37256, #31087, #5970, #28202, #34366, #9474, #9688, #3110, #34767, #27800, #12558, #24517, #67, #2696, #6181, #8868, #30879 ),
 .UNSPECIFIED., .F., .F.,
 ( 4, 2, 1, 2, 2, 2, 2, 2, 2, 2, 2, 2, 2, 2, 2, 2, 2, 2, 2, 2, 2, 2, 2, 2, 2, 2, 2, 2, 2, 2, 2, 4 ),
 ( -5.999999999593325711E-08, 0.0002089317286102376910, 0.0004179234572204712853, 0.0008359069144409385279, 0.001671873828881873013, 0.003343807657763743068, 0.005015741486645609870, 0.006687675315527477106, 0.01003154297329121244, 0.01170347680217307881, 0.01337541063105494692, 0.02006314594658243147, 0.02173507977546430131, 0.02340701360434616768, 0.02675088126210990735, 0.03009474891987364703, 0.03343861657763738671, 0.03511055040651924614, 0.03678248423540111250, 0.03845441806428297887, 0.04012635189316483830, 0.04179828572204669773, 0.04347021955092856410, 0.04514215337981042353, 0.04597812029425134978, 0.04681408720869228296, 0.04848602103757415627, 0.05015795486645601570, 0.05182988869533788207, 0.05266585560977881525, 0.05308383906699928184, 0.05350182252421974149 ),
 .UNSPECIFIED. ) ;
#7562 = CARTESIAN_POINT ( 'NONE',  ( 0.1049860589904711705, -1.308425076921832408, 0.4359114761720587206 ) ) ;
#7563 = SECURITY_CLASSIFICATION ( '', '', #30930 ) ;
#7564 = CARTESIAN_POINT ( 'NONE',  ( 0.1835387414513457993, -1.269102812158692473, 1.002600033288329140 ) ) ;
#7565 = CARTESIAN_POINT ( 'NONE',  ( 0.5892429738200350986, -1.562419363825541918, -0.4777725863729586075 ) ) ;
#7566 = CARTESIAN_POINT ( 'NONE',  ( 0.03113248654051816583, 0.8492681979939306069, -0.2138253033704805295 ) ) ;
#7567 = CARTESIAN_POINT ( 'NONE',  ( -0.01548846960707524721, 0.000000000000000000, 0.000000000000000000 ) ) ;
#7568 = CARTESIAN_POINT ( 'NONE',  ( -0.02872242845530498245, -0.3729171224323651890, 0.3802687114177512040 ) ) ;
#7569 = TOROIDAL_SURFACE ( 'NONE', #37157, 0.04249999999999999611, 0.02499999999999995628 ) ;
#7570 = ORIENTED_EDGE ( 'NONE', *, *, #2407, .F. ) ;
#7571 = ORIENTED_EDGE ( 'NONE', *, *, #38475, .F. ) ;
#7572 = CARTESIAN_POINT ( 'NONE',  ( 0.1438681892407857876, -1.284094082863941111, 0.3157417262808777658 ) ) ;
#7573 = EDGE_LOOP ( 'NONE', ( #31271, #25668, #9806, #477, #39063, #10346, #12761, #36300, #35977, #17559 ) ) ;
#7574 = CARTESIAN_POINT ( 'NONE',  ( 0.6011193747858227798, -1.595581932925101976, 0.4276689662439276396 ) ) ;
#7575 = CARTESIAN_POINT ( 'NONE',  ( -0.2746410161513776482, -3.723902497147952406, 0.1004495357399106253 ) ) ;
#7576 = CARTESIAN_POINT ( 'NONE',  ( 0.5324855789941030926, -1.347847315281903491, 0.7002209793041090924 ) ) ;
#7578 = ORIENTED_EDGE ( 'NONE', *, *, #39452, .F. ) ;
#7577 = CARTESIAN_POINT ( 'NONE',  ( -0.05283102792148799270, 0.4315398646667473193, 0.1819478359276328061 ) ) ;
#7579 = CARTESIAN_POINT ( 'NONE',  ( 0.4100600194349330319, -1.011029760475403494, 0.6817144834752139060 ) ) ;
#7580 = CARTESIAN_POINT ( 'NONE',  ( 0.05634301242525761172, 0.4396003943662958324, -0.1320237143668752666 ) ) ;
#7581 = VERTEX_POINT ( 'NONE', #1139 ) ;
#7582 = CARTESIAN_POINT ( 'NONE',  ( 0.3247353678145296074, -1.174695915522060652, 0.5636564603779772309 ) ) ;
#7583 = ORIENTED_EDGE ( 'NONE', *, *, #28824, .F. ) ;
#7584 = CARTESIAN_POINT ( 'NONE',  ( 0.02592883741220372920, -0.5747094013104246946, 0.3049468829503017564 ) ) ;
#7586 = CARTESIAN_POINT ( 'NONE',  ( 0.5826217342940260835, -1.634307228436295167, 0.5182417262812423209 ) ) ;
#7585 = CARTESIAN_POINT ( 'NONE',  ( 0.6950632297095953316, -1.495237220361341102, 0.4800255380849818287 ) ) ;
#7587 = CARTESIAN_POINT ( 'NONE',  ( 0.05560027925352286488, -1.335209592177159843, 0.5707417262808780478 ) ) ;
#7588 = CARTESIAN_POINT ( 'NONE',  ( 0.07493559420041842611, -1.491955960748385657, -0.3421605232025932142 ) ) ;
#7589 = VERTEX_POINT ( 'NONE', #38122 ) ;
#7590 = AXIS2_PLACEMENT_3D ( 'NONE', #23790, #29540, #8342 ) ;
#7591 = AXIS2_PLACEMENT_3D ( 'NONE', #6337, #33160, #18909 ) ;
#7592 = DIRECTION ( 'NONE',  ( 1.000000000000000000, 3.035386659626936255E-15, -7.588466649067340637E-16 ) ) ;
#7593 = CARTESIAN_POINT ( 'NONE',  ( 0.02333805985610111142, -1.614515438906713118, -0.6389321993329700744 ) ) ;
#7594 = CARTESIAN_POINT ( 'NONE',  ( 0.01895494625228220584, 0.4667936258712425679, 0.2292799240428173291 ) ) ;
#7595 = CARTESIAN_POINT ( 'NONE',  ( 0.4335229873338388717, -1.223245311458436069, 0.6222225527454730010 ) ) ;
#7596 = LOCAL_TIME ( 0, 53, 7.000000000000000000, #28929 ) ;
#7597 = CARTESIAN_POINT ( 'NONE',  ( 0.3253942546199506958, -1.752804466647932546, 0.4715143355759890409 ) ) ;
#7598 = CARTESIAN_POINT ( 'NONE',  ( 0.4618534464035452536, -1.161788201396328546, 0.4182417262808778013 ) ) ;
#7599 = AXIS2_PLACEMENT_3D ( 'NONE', #26052, #26441, #11017 ) ;
#7600 = CARTESIAN_POINT ( 'NONE',  ( -0.1542173385434465194, 0.4780076866987634232, 0.3460825593793592780 ) ) ;
#7601 = DIRECTION ( 'NONE',  ( 0.9378410757839518164, 0.1072489841977738861, 0.3300784330442475545 ) ) ;
#7602 = DIRECTION ( 'NONE',  ( 1.000000000000000000, 0.000000000000000000, 7.762739824594491602E-16 ) ) ;
#7603 = CARTESIAN_POINT ( 'NONE',  ( -0.2399999999999999079, -3.941790907013290823, -0.4709369376873030477 ) ) ;
#7604 = CARTESIAN_POINT ( 'NONE',  ( 0.1678534701465425882, -1.280328660040236377, 0.4182417262808778013 ) ) ;
#7605 = PRODUCT_CONTEXT ( 'NONE', #1170, 'mechanical' ) ;
#7606 = CARTESIAN_POINT ( 'NONE',  ( 0.006374870886235760488, -0.9785717880618779452, 0.4789926383131983822 ) ) ;
#7607 = ADVANCED_FACE ( 'NONE', ( #19625 ), #27159, .T. ) ;
#7608 = EDGE_CURVE ( 'NONE', #31622, #4130, #692, .T. ) ;
#7609 = DIRECTION ( 'NONE',  ( 5.551115123125703816E-17, -5.306893166658304503E-16, -1.000000000000000000 ) ) ;
#7610 = PRODUCT_DEFINITION_CONTEXT ( 'detailed design', #21638, 'design' ) ;
#7611 = CARTESIAN_POINT ( 'NONE',  ( 0.7066109249242027435, -1.499057094600571238, 0.5182417262806440217 ) ) ;
#7612 = CARTESIAN_POINT ( 'NONE',  ( -0.2399999999999999079, -3.941790907013290823, -0.5334369376873030477 ) ) ;
#7613 = CARTESIAN_POINT ( 'NONE',  ( 0.3957164860440396392, -2.010354213676031065, -0.5038375161603109165 ) ) ;
#7614 = EDGE_CURVE ( 'NONE', #11375, #19638, #35810, .T. ) ;
#7615 = CARTESIAN_POINT ( 'NONE',  ( 0.2716900230296190322, -1.558453453380033604, 0.9768685533762022644 ) ) ;
#7616 = CLOSED_SHELL ( 'NONE', ( #13068, #16811, #12641, #39164, #3669, #8238, #13744, #17739, #1369, #19577, #31586, #3472, #32506, #30124, #31794, #16296, #36779, #11253, #4457, #25487, #36815, #26813, #34337, #32524, #28527, #31102, #3631, #24043, #15759, #5498, #28349, #39333, #18031, #23008, #8933, #39435, #972, #39856, #12790, #18428, #38669, #21490, #29047, #33008, #33646, #6007, #24432, #23757, #33558, #18055, #13921, #2943, #30383, #30324, #32562, #32779, #10684, #26034, #5449, #17864, #24310, #10178, #17581, #6355, #9677, #33401, #29025, #16804, #28895, #3945, #34182, #20324, #14214, #30104, #13071, #5356, #8997, #27522, #9263, #4984, #10423, #24986, #8469, #10408, #15753, #18448, #26299, #18491, #12047, #18695, #2601, #30798, #23013, #22342, #40074, #22815, #22842, #36391, #5686, #1208, #6619, #21751, #4674, #25876, #40249, #744, #17988, #34269, #24313, #17229, #13915, #37437, #15272, #3688, #6367, #22871, #11004, #6443, #18551, #24775, #29532, #36627, #4724, #7101, #30330, #2458, #11761, #38541, #22574, #3686, #26373, #11009, #17186, #31532, #12515, #9445, #5207, #133, #29076, #39357, #6128, #9891, #28360, #40331, #12728, #27148, #19984, #11297, #20272, #11070, #17834, #7607, #39947, #8455, #1426, #17679, #13431, #1003, #23904, #31692, #22002, #5878 ) ) ;
#7617 = AXIS2_PLACEMENT_3D ( 'NONE', #16179, #166, #35083 ) ;
#7618 = DIRECTION ( 'NONE',  ( 1.000000000000000000, 0.000000000000000000, 0.000000000000000000 ) ) ;
#7619 = ADVANCED_FACE ( 'NONE', ( #32513 ), #19583, .F. ) ;
#7620 = ORIENTED_EDGE ( 'NONE', *, *, #25842, .T. ) ;
#7621 = ORIENTED_EDGE ( 'NONE', *, *, #20365, .F. ) ;
#7622 = CARTESIAN_POINT ( 'NONE',  ( 0.1877434453300698414, -0.5089539054925988903, 0.1080467165728084405 ) ) ;
#7623 = EDGE_LOOP ( 'NONE', ( #23172, #38094, #24705, #5723, #22197 ) ) ;
#7624 = ORGANIZATION ( 'NAUO-ORG10', 'UNSPECIFIED', 'UNSPECIFIED' ) ;
#7625 = CARTESIAN_POINT ( 'NONE',  ( 0.2603803840244302559, -1.679120311287623624, 0.5759385929908824586 ) ) ;
#7626 = CARTESIAN_POINT ( 'NONE',  ( 0.5066971731404251722, -1.347239037406359197, 0.8035729607927099005 ) ) ;
#7628 = ORIENTED_EDGE ( 'NONE', *, *, #25563, .F. ) ;
#7627 = CARTESIAN_POINT ( 'NONE',  ( -0.001991110985728673961, -0.8396244724827389705, 0.09658552693076032092 ) ) ;
#7629 = AXIS2_PLACEMENT_3D ( 'NONE', #2760, #2971, #9322 ) ;
#7631 = ORIENTED_EDGE ( 'NONE', *, *, #25370, .T. ) ;
#7630 = ORIENTED_EDGE ( 'NONE', *, *, #29180, .T. ) ;
#7632 = CARTESIAN_POINT ( 'NONE',  ( -0.2746410161513782033, -2.289343986263487896, -0.6686455968847019316 ) ) ;
#7633 = ORIENTED_EDGE ( 'NONE', *, *, #34025, .F. ) ;
#7634 = EDGE_CURVE ( 'NONE', #39928, #12063, #25676, .T. ) ;
#7635 = CARTESIAN_POINT ( 'NONE',  ( 0.1820039756314770496, -1.353402374702050048, 0.9460902548477880813 ) ) ;
#7637 = CARTESIAN_POINT ( 'NONE',  ( 0.3984114568195522010, -1.599003643269838904, -0.5155029497116575543 ) ) ;
#7636 = DIRECTION ( 'NONE',  ( -0.4999999999999995559, 0.6123724356957945814, -0.6123724356957945814 ) ) ;
#7638 = PRODUCT_RELATED_PRODUCT_CATEGORY ( 'detail', '', ( #29493 ) ) ;
#7639 = CARTESIAN_POINT ( 'NONE',  ( 0.6215274601157204648, -1.354888019438377444, -0.6250000000000000000 ) ) ;
#7640 = APPROVAL_ROLE ( '' ) ;
#7641 = FACE_OUTER_BOUND ( 'NONE', #2669, .T. ) ;
#7643 = VERTEX_POINT ( 'NONE', #13397 ) ;
#7642 = ORIENTED_EDGE ( 'NONE', *, *, #25092, .F. ) ;
#7644 = CARTESIAN_POINT ( 'NONE',  ( 0.1297863134137367813, -0.8346111980775223760, 0.4665308214793116304 ) ) ;
#7645 = B_SPLINE_CURVE_WITH_KNOTS ( 'NONE', 3,
 ( #5537, #2664, #8834, #40296, #37010, #12527 ),
 .UNSPECIFIED., .F., .F.,
 ( 4, 2, 4 ),
 ( 0.000000000000000000, 0.0005427992237399233491, 0.001085598447479846698 ),
 .UNSPECIFIED. ) ;
#7646 = CARTESIAN_POINT ( 'NONE',  ( 0.01703266676564623230, -0.8936126741228921366, 0.5128946615551410737 ) ) ;
#7647 = CARTESIAN_POINT ( 'NONE',  ( 0.09106748660175942311, -0.5564522452151119403, 0.2171823283136207761 ) ) ;
#7648 = CARTESIAN_POINT ( 'NONE',  ( 0.5372047856502307761, -1.509560927297886934, 0.6722531729593694827 ) ) ;
#7649 = CARTESIAN_POINT ( 'NONE',  ( 0.1978587402095111636, -0.5849795632145003976, 0.3178455878192510409 ) ) ;
#7650 = DIRECTION ( 'NONE',  ( 0.9998941247116546194, -0.01455087607601020239, 0.0001066420868422379362 ) ) ;
#7651 = CARTESIAN_POINT ( 'NONE',  ( 0.6586055134406099132, -1.459595632619679950, 0.4243909478079631037 ) ) ;
#7652 = CARTESIAN_POINT ( 'NONE',  ( 0.3701867111158838042, -1.742907794848391978, 0.6016813899000484911 ) ) ;
#7653 = CIRCLE ( 'NONE', #14883, 0.1033070866141734129 ) ;
#7654 = CARTESIAN_POINT ( 'NONE',  ( 0.4136294883733862005, -1.694877849074643672, 0.4182417262808776903 ) ) ;
#7655 = DIRECTION ( 'NONE',  ( 1.000000000000000000, 2.280301054154495132E-31, -1.664003471950577689E-31 ) ) ;
#7656 = CARTESIAN_POINT ( 'NONE',  ( 0.3999999999999798161, -2.143572916703662123, -0.4549832530184109713 ) ) ;
#7657 = CARTESIAN_POINT ( 'NONE',  ( -6.702082025768050936E-05, -0.7526509584479209591, -0.09479413075768641783 ) ) ;
#7658 = CARTESIAN_POINT ( 'NONE',  ( 0.5817652315481057768, -1.478716734979794944, 0.6771717844549590692 ) ) ;
#7659 = APPLIED_APPROVAL_ASSIGNMENT ( #28650, ( #24771 ) ) ;
#7660 =( CONVERSION_BASED_UNIT ( 'INCH', #39331 ) LENGTH_UNIT ( ) NAMED_UNIT ( #22863 ) );
#7661 = DIRECTION ( 'NONE',  ( 0.5196341416262992841, -0.8543888803444829039, 0.000000000000000000 ) ) ;
#7662 = CARTESIAN_POINT ( 'NONE',  ( 0.5804493474056371394, -1.147657283997232991, -0.5155029497116575543 ) ) ;
#7663 = VECTOR ( 'NONE', #6932, 39.37007874015748143 ) ;
#7664 = CARTESIAN_POINT ( 'NONE',  ( 0.1235390412447300995, -1.439500955437662766, 0.5982358349985300583 ) ) ;
#7665 = CARTESIAN_POINT ( 'NONE',  ( 0.4916028908188559421, -1.081978336766327820, 0.5838299722441698814 ) ) ;
#7666 = EDGE_CURVE ( 'NONE', #24008, #11393, #30229, .T. ) ;
#7667 = PERSON_AND_ORGANIZATION_ROLE ( 'creator' ) ;
#7668 = CARTESIAN_POINT ( 'NONE',  ( 0.5827378505010344378, -1.244973309454295629, 0.8759922176168969399 ) ) ;
#7669 = ADVANCED_FACE ( 'NONE', ( #4123 ), #13604, .T. ) ;
#7670 = EDGE_CURVE ( 'NONE', #35412, #16124, #23076, .T. ) ;
#7671 = DIRECTION ( 'NONE',  ( 0.8660512985181135770, 0.4999551463232372317, 0.000000000000000000 ) ) ;
#7672 = EDGE_CURVE ( 'NONE', #16220, #15882, #40092, .T. ) ;
#7673 = CARTESIAN_POINT ( 'NONE',  ( 0.3136699570144902971, -1.762202131979911712, 0.5691132299474264133 ) ) ;
#7674 = VERTEX_POINT ( 'NONE', #32717 ) ;
#7675 = DIRECTION ( 'NONE',  ( 0.000000000000000000, -0.8090169943749413450, 0.5877852522924816858 ) ) ;
#7676 = CARTESIAN_POINT ( 'NONE',  ( 0.002369698199515762795, -0.5286367086536888360, 0.1583934855509527007 ) ) ;
#7677 = CARTESIAN_POINT ( 'NONE',  ( 0.6472550179972602624, -1.446945511653702443, -0.6249999999999998890 ) ) ;
#7678 = ORIENTED_EDGE ( 'NONE', *, *, #13770, .F. ) ;
#7679 = VECTOR ( 'NONE', #2164, 39.37007874015748143 ) ;
#7680 = CARTESIAN_POINT ( 'NONE',  ( 0.07216878364870175921, 0.05141091571461216952, -0.1249999999999971689 ) ) ;
#7681 = CARTESIAN_POINT ( 'NONE',  ( 0.4763737863547038431, -1.078928959615589100, 0.8012595312036666639 ) ) ;
#7683 = ORIENTED_EDGE ( 'NONE', *, *, #36333, .T. ) ;
#7682 = EDGE_LOOP ( 'NONE', ( #9132, #21417, #27998, #36314, #36221 ) ) ;
#7684 = CARTESIAN_POINT ( 'NONE',  ( 0.0004587754601000432132, -1.956353996556619457, -0.6605311053939741939 ) ) ;
#7685 =( BOUNDED_SURFACE ( )  B_SPLINE_SURFACE ( 3, 2, ( 
 ( #9822, #428, #22601 ),
 ( #35336, #22813, #28943 ),
 ( #32225, #25477, #7320 ),
 ( #16607, #34921, #38012 ) ),
 .UNSPECIFIED., .F., .F., .T. ) 
 B_SPLINE_SURFACE_WITH_KNOTS ( ( 4, 4 ),
 ( 3, 3 ),
 ( -1.198043400596482400E-17, 0.0005284928876949268779 ),
 ( 0.000000000000000000, 1.000000000000000000 ),
 .UNSPECIFIED. ) 
 GEOMETRIC_REPRESENTATION_ITEM ( )  RATIONAL_B_SPLINE_SURFACE ( (
 ( 1.000000000000000000, 0.8671479162384729822, 1.000000000000000000),
 ( 1.000000000000000000, 0.8820622678756920854, 1.000000000000000000),
 ( 1.000000000000000000, 0.8880894362480542537, 1.000000000000000000),
 ( 1.000000000000000000, 0.8864945003981776761, 1.000000000000000000) ) ) 
 REPRESENTATION_ITEM ( '' )  SURFACE ( )  );
#7686 = DIRECTION ( 'NONE',  ( 1.000000000000000000, 0.000000000000000000, 0.000000000000000000 ) ) ;
#7687 = EDGE_CURVE ( 'NONE', #18202, #4342, #10929, .T. ) ;
#7688 = CARTESIAN_POINT ( 'NONE',  ( 0.2898911397524138733, -1.200022992789476328, 0.4282476769854300369 ) ) ;
#7689 = CARTESIAN_POINT ( 'NONE',  ( -0.04211471441534243160, 0.4486586774158433100, -0.1367340165256737128 ) ) ;
#7690 = EDGE_LOOP ( 'NONE', ( #26634, #15973, #16246, #25355 ) ) ;
#7691 = CARTESIAN_POINT ( 'NONE',  ( 0.1406250000000001388, -0.4888214998617192442, 0.3238651926494596767 ) ) ;
#7692 = CARTESIAN_POINT ( 'NONE',  ( 0.2560554501240281389, -0.9391908526076655495, 0.7069755978740671631 ) ) ;
#7693 = CARTESIAN_POINT ( 'NONE',  ( 0.1969934931346632723, -1.289641399371132424, 1.023064179873733659 ) ) ;
#7694 = CARTESIAN_POINT ( 'NONE',  ( 0.1117195309642857459, -0.6771241826238267869, 0.4786975410683091958 ) ) ;
#7696 = DIRECTION ( 'NONE',  ( 0.4999551463232372317, -0.8660512985181135770, 0.000000000000000000 ) ) ;
#7695 = CARTESIAN_POINT ( 'NONE',  ( 0.2713523440619998173, -1.672253707410367829, 0.7222851353733067414 ) ) ;
#7697 = CARTESIAN_POINT ( 'NONE',  ( 0.1521791078991787949, -1.215866141468441963, 0.6421765199397219126 ) ) ;
#7698 = VERTEX_POINT ( 'NONE', #17088 ) ;
#7699 = CARTESIAN_POINT ( 'NONE',  ( 0.6554021398533210752, -1.532257051837409900, -0.6160679160980194746 ) ) ;
#7700 = CARTESIAN_POINT ( 'NONE',  ( 0.1317003362355874119, -0.5351829081616051864, 0.4217891011909937760 ) ) ;
#7701 = DIRECTION ( 'NONE',  ( -0.4999551463232372317, 0.8660512985181135770, -0.000000000000000000 ) ) ;
#7702 = CARTESIAN_POINT ( 'NONE',  ( -0.04139678531769518804, -0.4420204940294896745, -0.1614859807034213779 ) ) ;
#7703 = CARTESIAN_POINT ( 'NONE',  ( 0.002290818369124609372, -0.5198888459286679087, 0.1457185332388686583 ) ) ;
#7704 = CARTESIAN_POINT ( 'NONE',  ( 0.3379549838205658796, -1.287644724967739629, -0.5155029497116575543 ) ) ;
#7705 = CARTESIAN_POINT ( 'NONE',  ( 0.6150013826522254812, -1.299199899150926374, 0.5044333340123036136 ) ) ;
#7706 = EDGE_CURVE ( 'NONE', #19341, #5039, #3307, .T. ) ;
#7707 = CARTESIAN_POINT ( 'NONE',  ( -0.2746410161513770931, -3.194091454214595949, -0.5766534813907827628 ) ) ;
#7708 = EDGE_CURVE ( 'NONE', #28983, #8492, #17885, .T. ) ;
#7709 = CARTESIAN_POINT ( 'NONE',  ( 0.07438451276000504486, -1.494117022116229654, -0.3422791976087487531 ) ) ;
#7710 = CARTESIAN_POINT ( 'NONE',  ( 0.5424528042998149058, -1.629943420504956553, -0.5873670775642777508 ) ) ;
#7711 = VERTEX_POINT ( 'NONE', #26568 ) ;
#7712 = CARTESIAN_POINT ( 'NONE',  ( 0.4411652911884185180, -1.201865629404675229, 0.6973157100092504113 ) ) ;
#7713 = CARTESIAN_POINT ( 'NONE',  ( -0.02000000000000000042, -2.468922287121626091, -0.3957877349972418468 ) ) ;
#7714 = ADVANCED_FACE ( 'NONE', ( #8018 ), #14460, .F. ) ;
#7715 = CARTESIAN_POINT ( 'NONE',  ( -0.04230258372739897216, -0.2788587125276409950, -0.3766249785157098073 ) ) ;
#7716 = VERTEX_POINT ( 'NONE', #20594 ) ;
#7717 = EDGE_CURVE ( 'NONE', #7737, #40210, #17293, .T. ) ;
#7718 = DIRECTION ( 'NONE',  ( -1.000000000000000000, -1.441634041478669458E-15, 8.359771364787550201E-16 ) ) ;
#7719 = CARTESIAN_POINT ( 'NONE',  ( -0.03309058451312549970, 0.08822157290689555675, -0.5132714794726503937 ) ) ;
#7720 = CARTESIAN_POINT ( 'NONE',  ( 0.02999999999990856162, -2.097674344635099608, -0.7286986457865541889 ) ) ;
#7721 = CARTESIAN_POINT ( 'NONE',  ( 0.4321640349418070515, -1.121330984503925876, 0.5310794168832609907 ) ) ;
#7722 = CARTESIAN_POINT ( 'NONE',  ( 0.03247176862405053849, -0.8418478330200259707, 0.2157142965010831193 ) ) ;
#7723 = ORIENTED_EDGE ( 'NONE', *, *, #4859, .F. ) ;
#7724 = DIRECTION ( 'NONE',  ( -0.4999999999999965028, -0.6509737717187625838, 0.5711682313769312902 ) ) ;
#7725 = EDGE_CURVE ( 'NONE', #38276, #3878, #7816, .T. ) ;
#7726 = CARTESIAN_POINT ( 'NONE',  ( 0.6627999150273293782, -1.460136208901648081, -0.4136584506876441747 ) ) ;
#7727 = CARTESIAN_POINT ( 'NONE',  ( 0.1817793365275204021, -1.377674457685613696, 0.4214207381694095589 ) ) ;
#7728 = EDGE_CURVE ( 'NONE', #36370, #28193, #4523, .T. ) ;
#7729 = CARTESIAN_POINT ( 'NONE',  ( 0.6544078563150221850, -1.544269123161552626, 0.4241055859090109292 ) ) ;
#7730 = CARTESIAN_POINT ( 'NONE',  ( 0.4795933240383793428, -1.258180956532618744, 0.5929850450974815113 ) ) ;
#7732 = CARTESIAN_POINT ( 'NONE',  ( 0.4688079631758284016, -1.116561345930851656, 0.5688791344137259509 ) ) ;
#7731 = CARTESIAN_POINT ( 'NONE',  ( -0.1450923023275084156, -0.5230583524814751417, 0.1380392329925462791 ) ) ;
#7733 = CARTESIAN_POINT ( 'NONE',  ( 0.5764814451414584928, -1.536917970227292596, -0.4740999583163317821 ) ) ;
#7734 = ORIENTED_EDGE ( 'NONE', *, *, #31872, .F. ) ;
#7735 = EDGE_CURVE ( 'NONE', #23598, #17175, #34198, .T. ) ;
#7736 = CARTESIAN_POINT ( 'NONE',  ( -0.2399999999999999079, -3.950462929358175668, -0.4586978189098018799 ) ) ;
#7737 = VERTEX_POINT ( 'NONE', #29636 ) ;
#7738 = CARTESIAN_POINT ( 'NONE',  ( 0.1825071904178995619, -0.7337134285967986669, 0.1479976049341028554 ) ) ;
#7739 = CARTESIAN_POINT ( 'NONE',  ( 0.05587308000523566465, -0.6076548949599507310, 0.3685913880743675319 ) ) ;
#7741 = CARTESIAN_POINT ( 'NONE',  ( 0.02953079040095673430, -0.5250338024619264354, 0.07436286310882474215 ) ) ;
#7740 = CARTESIAN_POINT ( 'NONE',  ( 0.06914125879787166862, -0.5405346344223664889, 0.1297049665551865405 ) ) ;
#7742 = CARTESIAN_POINT ( 'NONE',  ( 0.1665044839944595234, -1.270767161555115932, 0.4854677671074156264 ) ) ;
#7743 = VERTEX_POINT ( 'NONE', #1478 ) ;
#7744 = ORIENTED_EDGE ( 'NONE', *, *, #16014, .T. ) ;
#7745 = FACE_OUTER_BOUND ( 'NONE', #27632, .T. ) ;
#7746 = CARTESIAN_POINT ( 'NONE',  ( 0.1193013743603501958, -0.5494898923379011313, 0.1617980040493336713 ) ) ;
#7747 = CIRCLE ( 'NONE', #13672, 0.05000000000000000971 ) ;
#7748 = ORIENTED_EDGE ( 'NONE', *, *, #37298, .T. ) ;
#7749 = DIRECTION ( 'NONE',  ( 1.060606950627616773E-16, 6.122684696619993730E-17, 1.000000000000000000 ) ) ;
#7750 = CARTESIAN_POINT ( 'NONE',  ( 0.03170874437002701302, -0.4481116538287146511, 0.2027256324086040840 ) ) ;
#7751 = CARTESIAN_POINT ( 'NONE',  ( 0.3885448048373752461, -1.754957712888778776, -0.4416481762448698500 ) ) ;
#7752 = CARTESIAN_POINT ( 'NONE',  ( 0.1571803435121711390, -1.276327713282634058, 0.4309217000577236223 ) ) ;
#7753 = CARTESIAN_POINT ( 'NONE',  ( -0.1630577892339038493, 0.4726628520879604944, 0.1187338422647632452 ) ) ;
#7754 = CARTESIAN_POINT ( 'NONE',  ( 0.08989082913961529697, -0.5631763781711711658, 0.1462941165619876527 ) ) ;
#7755 = CARTESIAN_POINT ( 'NONE',  ( 0.1875000000000000833, -0.4595382586000822389, 0.1581505021253525878 ) ) ;
#7756 = CARTESIAN_POINT ( 'NONE',  ( 0.1424029337235096226, -1.400533250147911746, -0.3244367222852112542 ) ) ;
#7757 = DIRECTION ( 'NONE',  ( -0.4999551463232373427, 0.8660512985181134660, -0.000000000000000000 ) ) ;
#7758 = ADVANCED_FACE ( 'NONE', ( #2282 ), #14821, .T. ) ;
#7759 = CARTESIAN_POINT ( 'NONE',  ( 0.5794003230470022858, -1.608195470634162128, -0.5609915163756674650 ) ) ;
#7760 = CARTESIAN_POINT ( 'NONE',  ( 0.2165002020277727868, -1.357372643808337775, 0.4854677670904418152 ) ) ;
#7761 = CARTESIAN_POINT ( 'NONE',  ( 0.1841981897273382851, -0.8536146481143929154, 0.1250772005134268283 ) ) ;
#7762 = ADVANCED_FACE ( 'NONE', ( #17503 ), #19732, .F. ) ;
#7763 = CYLINDRICAL_SURFACE ( 'NONE', #15943, 0.1000000000000000194 ) ;
#7764 = CARTESIAN_POINT ( 'NONE',  ( -0.1049931804392554846, -0.4770575742336289338, 0.3602693336304481075 ) ) ;
#7765 = B_SPLINE_CURVE_WITH_KNOTS ( 'NONE', 3,
 ( #14444, #4990, #20647, #4387, #14052, #10556, #39350, #16747, #10987, #29484 ),
 .UNSPECIFIED., .F., .F.,
 ( 4, 2, 2, 2, 4 ),
 ( 1.734723475976807094E-18, 0.0006437901958235721887, 0.001287580391647142643, 0.001931370587470713097, 0.002575160783294283551 ),
 .UNSPECIFIED. ) ;
#7766 = DIRECTION ( 'NONE',  ( 0.2841200139107300515, 0.1745296787418094686, -0.9427699660753134925 ) ) ;
#7767 = CARTESIAN_POINT ( 'NONE',  ( 0.5858181074991345438, -1.569584648740467214, -0.5056512426634341972 ) ) ;
#7768 = DIRECTION ( 'NONE',  ( 1.000000000000000000, -0.000000000000000000, -0.000000000000000000 ) ) ;
#7769 = CARTESIAN_POINT ( 'NONE',  ( 0.3047917018647445242, -1.756872442562883219, 0.5682425124847924058 ) ) ;
#7770 = CARTESIAN_POINT ( 'NONE',  ( -0.05268850283020223846, -0.2791746226943827569, 0.3764045485075394604 ) ) ;
#7771 = ORIENTED_EDGE ( 'NONE', *, *, #3625, .F. ) ;
#7772 = ORIENTED_EDGE ( 'NONE', *, *, #26909, .T. ) ;
#7773 = CARTESIAN_POINT ( 'NONE',  ( 0.1050286246271734808, -1.410831341392925209, 0.5682417262808875380 ) ) ;
#7774 = CARTESIAN_POINT ( 'NONE',  ( 0.2319960710055803677, -1.232736008543062090, 0.4687417262808780127 ) ) ;
#7775 = EDGE_LOOP ( 'NONE', ( #32510, #24118, #38842, #28894, #26875 ) ) ;
#7776 = DIRECTION ( 'NONE',  ( 8.881784197001246407E-16, -2.361472542561082612E-16, 1.000000000000000000 ) ) ;
#7777 = DIRECTION ( 'NONE',  ( -0.4999999999999978351, -3.389636702121520322E-32, 0.8660254037844398178 ) ) ;
#7778 = CARTESIAN_POINT ( 'NONE',  ( 0.5509096165736990791, -1.379093160209163615, 0.7167504442928195330 ) ) ;
#7780 = ORIENTED_EDGE ( 'NONE', *, *, #16199, .F. ) ;
#7779 = CARTESIAN_POINT ( 'NONE',  ( -0.1603938765018626533, 0.4636889572248046321, 0.1178658435937001703 ) ) ;
#7781 = CARTESIAN_POINT ( 'NONE',  ( 0.2467813525974754951, -0.8519813862200177335, 0.4954293255957377684 ) ) ;
#7782 = CARTESIAN_POINT ( 'NONE',  ( -0.2399999999999999079, -3.840189043187996809, -0.1239867222638698224 ) ) ;
#7783 = ORIENTED_EDGE ( 'NONE', *, *, #8505, .T. ) ;
#7784 = DIRECTION ( 'NONE',  ( 0.4999551463232373427, -0.8660512985181134660, 0.000000000000000000 ) ) ;
#7785 = CARTESIAN_POINT ( 'NONE',  ( 0.04494180016761560592, -0.6777367256777560023, 0.5045707990937741139 ) ) ;
#7787 = CARTESIAN_POINT ( 'NONE',  ( 0.1150990105419666260, -0.4532349895251732708, 0.08714482709981570541 ) ) ;
#7786 = CARTESIAN_POINT ( 'NONE',  ( 0.7013323771326090972, -1.495406364347797279, 0.4952476761773726421 ) ) ;
#7788 = FACE_OUTER_BOUND ( 'NONE', #38636, .T. ) ;
#7789 = CARTESIAN_POINT ( 'NONE',  ( 0.1909286924077255587, -1.257064795538239022, -0.3194715457588295227 ) ) ;
#7790 = ORIENTED_EDGE ( 'NONE', *, *, #4859, .T. ) ;
#7791 = CARTESIAN_POINT ( 'NONE',  ( 0.7009661026058806588, -1.563056106223301045, -0.5155029497116575543 ) ) ;
#7792 = CARTESIAN_POINT ( 'NONE',  ( 0.1781669208264307913, -1.264215222379440506, 0.4272368710745190201 ) ) ;
#7793 = CARTESIAN_POINT ( 'NONE',  ( 0.02231181081520686171, 0.5045902076536099568, 0.09028112709016243576 ) ) ;
#7794 = SHAPE_REPRESENTATION ( 'Lower cage plate', ( #27819 ), #37726 ) ;
#7795 = CARTESIAN_POINT ( 'NONE',  ( 0.2044132264669150933, -0.9676013961680371978, 0.6836346618487517679 ) ) ;
#7796 = FACE_OUTER_BOUND ( 'NONE', #8, .T. ) ;
#7797 = CARTESIAN_POINT ( 'NONE',  ( 0.03309059653085726083, 0.08822156176787604442, -0.5132714489379864853 ) ) ;
#7798 = CARTESIAN_POINT ( 'NONE',  ( 0.1118742967071392064, -0.9291314186530351682, 0.2025174426234049585 ) ) ;
#7799 = CARTESIAN_POINT ( 'NONE',  ( 0.02953079040095700838, 0.4684706630666080063, -0.2484463060367437248 ) ) ;
#7800 = CARTESIAN_POINT ( 'NONE',  ( 0.5467981811930779923, -1.652054351292815637, -0.5405695263049933308 ) ) ;
#7801 = CARTESIAN_POINT ( 'NONE',  ( 0.4265404446467185307, -1.123912635142109817, 0.5182417262812248904 ) ) ;
#7802 = DIRECTION ( 'NONE',  ( 1.000000000000000000, 0.000000000000000000, 0.000000000000000000 ) ) ;
#7803 = APPLICATION_PROTOCOL_DEFINITION ( 'international standard', 'automotive_design', 2000, #1170 ) ;
#7804 = CARTESIAN_POINT ( 'NONE',  ( 0.3698622724915323068, -1.154283567815744149, 0.4343510435345701026 ) ) ;
#7805 = CARTESIAN_POINT ( 'NONE',  ( 0.1792004983600124779, -0.4937710491622425146, 0.1299056045165895845 ) ) ;
#7806 = CARTESIAN_POINT ( 'NONE',  ( 0.000000000000000000, -0.01499999999999997689, 0.000000000000000000 ) ) ;
#7807 = PRODUCT_DEFINITION_SHAPE ( 'NONE', 'NONE',  #40665 ) ;
#7808 = CARTESIAN_POINT ( 'NONE',  ( 0.01548846960707524721, -0.09061086148575756005, -0.5171215251571035232 ) ) ;
#7809 = CARTESIAN_POINT ( 'NONE',  ( 0.5971614065082352374, -1.461417804984935342, 0.6057417262805111502 ) ) ;
#7810 = CARTESIAN_POINT ( 'NONE',  ( 0.1683513884741227873, -1.188089823937052758, 1.006248355024246477 ) ) ;
#7811 = CARTESIAN_POINT ( 'NONE',  ( -0.01548846960707524721, 0.3772621329472709006, 0.3651003739303413931 ) ) ;
#7812 = ORIENTED_EDGE ( 'NONE', *, *, #2958, .F. ) ;
#7813 = ORIENTED_EDGE ( 'NONE', *, *, #20885, .F. ) ;
#7814 = CARTESIAN_POINT ( 'NONE',  ( 0.1871607900928699830, -0.5063091123542899918, 0.1282519021220327460 ) ) ;
#7815 = ORIENTED_EDGE ( 'NONE', *, *, #22056, .F. ) ;
#7816 = LINE ( 'NONE', #14206, #38133 ) ;
#7817 = CARTESIAN_POINT ( 'NONE',  ( 0.6014930981134155585, -1.483010901933850434, 0.5633614063092290403 ) ) ;
#7819 = ORIENTED_EDGE ( 'NONE', *, *, #39675, .T. ) ;
#7818 = CARTESIAN_POINT ( 'NONE',  ( 0.008162182821621307913, -0.6980416593638927303, -0.01224155801182983359 ) ) ;
#7820 = ORIENTED_EDGE ( 'NONE', *, *, #24403, .T. ) ;
#7821 = CARTESIAN_POINT ( 'NONE',  ( 0.1183139781708525268, -0.4784996548529213967, 0.2899008765515939667 ) ) ;
#7822 = EDGE_LOOP ( 'NONE', ( #30313, #24698, #20434, #10232, #6600, #30565, #11796, #37746, #16398, #39406, #33696 ) ) ;
#7823 = CARTESIAN_POINT ( 'NONE',  ( -0.01357511779432049766, -0.5467070939194554891, 0.2476534432211799919 ) ) ;
#7825 = DIRECTION ( 'NONE',  ( 1.188678714063518227E-15, -1.000000000000000000, -3.263080277421930985E-16 ) ) ;
#7824 = CARTESIAN_POINT ( 'NONE',  ( -0.02869712619511821314, -0.4892154842446487240, -0.09550911579582112287 ) ) ;
#7826 = CARTESIAN_POINT ( 'NONE',  ( 0.6143533635013058714, -1.612503925854076536, -0.4829043714737934478 ) ) ;
#7827 = COORDINATED_UNIVERSAL_TIME_OFFSET ( 0, 0, .AHEAD. ) ;
#7828 = CARTESIAN_POINT ( 'NONE',  ( -0.0002183011148504172990, -0.4210325180397647693, 0.09509064842808868934 ) ) ;
#7830 = ORIENTED_EDGE ( 'NONE', *, *, #6421, .T. ) ;
#7829 = ORIENTED_EDGE ( 'NONE', *, *, #19808, .T. ) ;
#7831 = CARTESIAN_POINT ( 'NONE',  ( 0.09767084295088891699, -0.8240199256239116865, 0.3227011382480390878 ) ) ;
#7832 = CARTESIAN_POINT ( 'NONE',  ( 0.1188152677000469254, -1.411957481029216588, 0.5917154036330487532 ) ) ;
#7833 = CARTESIAN_POINT ( 'NONE',  ( 0.1031995293798165930, -0.6385813952848361508, 0.3661202089783873181 ) ) ;
#7834 = CARTESIAN_POINT ( 'NONE',  ( 0.5069166605951295201, -1.436909806687399316, 0.7822455750953455356 ) ) ;
#7835 = CARTESIAN_POINT ( 'NONE',  ( 0.02776779319759564019, -1.047279001274500798, 0.5925557623338770785 ) ) ;
#7836 = CARTESIAN_POINT ( 'NONE',  ( 0.5058599984363495450, -1.583313914148366752, -0.4933326546058600659 ) ) ;
#7837 = CARTESIAN_POINT ( 'NONE',  ( 0.5446855849587005638, -1.168303032256096108, 0.4182417297899396202 ) ) ;
#7838 = DIRECTION ( 'NONE',  ( 0.8660512985181134660, 0.4999551463232372317, 0.000000000000000000 ) ) ;
#7839 = CARTESIAN_POINT ( 'NONE',  ( 0.6935470237484337996, -1.428868995382490237, 0.5856070495622788252 ) ) ;
#7840 = DIRECTION ( 'NONE',  ( 0.8660512985181134660, 0.4999551463232371762, 0.000000000000000000 ) ) ;
#7841 = CARTESIAN_POINT ( 'NONE',  ( -0.1142670043590670176, -0.4723146173917492918, 0.1178658435936998927 ) ) ;
#7842 = CARTESIAN_POINT ( 'NONE',  ( 0.1499999999999996614, -0.09061086148574991339, 0.5171215251571054106 ) ) ;
#7843 = CARTESIAN_POINT ( 'NONE',  ( -2.485268943553615236E-05, -0.9232881051602984668, 0.03311238697358490773 ) ) ;
#7844 = CARTESIAN_POINT ( 'NONE',  ( 0.07442653783876213014, -0.5806215649999981743, 0.2956838457824742528 ) ) ;
#7845 = DIRECTION ( 'NONE',  ( 0.4999551463232377313, -0.8660512985181132439, -0.000000000000000000 ) ) ;
#7846 = CARTESIAN_POINT ( 'NONE',  ( -0.1157108546715163999, -0.4798936717283854292, 0.3382895567580818663 ) ) ;
#7847 = CARTESIAN_POINT ( 'NONE',  ( -0.003124719664520024271, -0.8057675726412024675, 0.09674340762273991867 ) ) ;
#7848 = CARTESIAN_POINT ( 'NONE',  ( 0.4929286275565831765, -1.082705722935900727, 0.5701913825460898089 ) ) ;
#7849 = PERSON_AND_ORGANIZATION_ROLE ( 'design_supplier' ) ;
#7850 = CARTESIAN_POINT ( 'NONE',  ( 0.3632211645871377126, -0.8757803013682723403, 0.7750855204132592879 ) ) ;
#7851 = ADVANCED_FACE ( 'NONE', ( #20387 ), #31122, .F. ) ;
#7852 = APPLIED_PERSON_AND_ORGANIZATION_ASSIGNMENT ( #9011, #34095, ( #5625 ) ) ;
#7853 = CARTESIAN_POINT ( 'NONE',  ( 0.3866201621456603621, -1.651307175440333008, -0.6361171515213966954 ) ) ;
#7854 = LINE ( 'NONE', #4169, #31766 ) ;
#7855 = VERTEX_POINT ( 'NONE', #36206 ) ;
#7856 = DIRECTION ( 'NONE',  ( -0.4999551463232373427, 0.8660512985181134660, -0.000000000000000000 ) ) ;
#7857 = CARTESIAN_POINT ( 'NONE',  ( 0.09587822187434574817, -1.032686032632677886, 0.8621212271250301429 ) ) ;
#7858 = CARTESIAN_POINT ( 'NONE',  ( 0.08510660916195567083, -1.306596824278190905, 0.4649156698885984484 ) ) ;
#7860 = EDGE_LOOP ( 'NONE', ( #22294, #38142, #36932, #23149, #21116, #20476, #1631 ) ) ;
#7859 = LINE ( 'NONE', #27433, #31630 ) ;
#7861 = CARTESIAN_POINT ( 'NONE',  ( 0.3240364041276366236, -1.756843918532213333, 0.4781731194503076043 ) ) ;
#7862 = CARTESIAN_POINT ( 'NONE',  ( 0.1914513227106267590, -0.5214848928147161056, 0.2513073325497693911 ) ) ;
#7864 = ORIENTED_EDGE ( 'NONE', *, *, #2462, .F. ) ;
#7863 = EDGE_LOOP ( 'NONE', ( #17806, #28932, #24293, #3280 ) ) ;
#7865 = CARTESIAN_POINT ( 'NONE',  ( 0.1102165803549850082, -1.338154550093276773, -0.7053715155666281378 ) ) ;
#7866 = VERTEX_POINT ( 'NONE', #1879 ) ;
#7867 = CARTESIAN_POINT ( 'NONE',  ( 0.05082294681498966682, -0.04864283519431490677, -0.4711332289091952896 ) ) ;
#7868 = CARTESIAN_POINT ( 'NONE',  ( 0.5686879079206863530, -1.501072830572683925, 0.5436612324038465616 ) ) ;
#7869 = CONICAL_SURFACE ( 'NONE', #38103, 0.5543128707267515054, 1.047197551196601628 ) ;
#7870 = CARTESIAN_POINT ( 'NONE',  ( -0.05269191099235458198, 0.4442874273374661787, -0.1490603884548157565 ) ) ;
#7871 = VERTEX_POINT ( 'NONE', #24101 ) ;
#7872 = CARTESIAN_POINT ( 'NONE',  ( 0.2101951102887192890, -1.233953443661628846, 0.5631135429232324574 ) ) ;
#7873 = CARTESIAN_POINT ( 'NONE',  ( 0.09953826690698990010, -0.7070161591386062705, 0.3305937928836391593 ) ) ;
#7874 = EDGE_CURVE ( 'NONE', #21489, #5206, #5939, .T. ) ;
#7875 = CARTESIAN_POINT ( 'NONE',  ( 0.1159210378633096922, -0.9846889132052908389, 0.9373222049632897734 ) ) ;
#7876 = VECTOR ( 'NONE', #25696, 39.37007874015748854 ) ;
#7877 = CARTESIAN_POINT ( 'NONE',  ( 0.09775142746979462172, -0.5484789642255779585, 0.1807369083563863665 ) ) ;
#7879 = FACE_OUTER_BOUND ( 'NONE', #39209, .T. ) ;
#7878 = CARTESIAN_POINT ( 'NONE',  ( 0.1842706337052801013, -1.340949179059101715, 0.9498145873395215100 ) ) ;
#7880 = CARTESIAN_POINT ( 'NONE',  ( 0.1802244519888198671, -0.9569834302806377035, 0.4667502891730959114 ) ) ;
#7881 = VERTEX_POINT ( 'NONE', #6155 ) ;
#7882 = ORIENTED_EDGE ( 'NONE', *, *, #16675, .F. ) ;
#7883 = ADVANCED_FACE ( 'NONE', ( #34340 ), #24983, .F. ) ;
#7884 = EDGE_CURVE ( 'NONE', #27951, #15118, #36334, .T. ) ;
#7885 = CARTESIAN_POINT ( 'NONE',  ( 0.6428829812445570058, -1.575050579808648488, -0.6023022189774835944 ) ) ;
#7886 = CARTESIAN_POINT ( 'NONE',  ( 0.1663702205777965182, -0.6275672944780111839, 0.5698197300990445191 ) ) ;
#7887 = EDGE_CURVE ( 'NONE', #14824, #26774, #27981, .T. ) ;
#7888 = LINE ( 'NONE', #23759, #4910 ) ;
#7889 = CARTESIAN_POINT ( 'NONE',  ( -0.02881329448201269683, -0.4889301291947605321, -0.09563270201326828923 ) ) ;
#7890 = DIRECTION ( 'NONE',  ( -1.000000000000000000, 0.000000000000000000, 0.000000000000000000 ) ) ;
#7891 = CARTESIAN_POINT ( 'NONE',  ( 0.1316017208954911588, -1.248059642665102942, 0.5182417262812423209 ) ) ;
#7892 = CARTESIAN_POINT ( 'NONE',  ( 0.6170741104697204937, -1.294989041298300947, 0.6128831306409553425 ) ) ;
#7893 = CARTESIAN_POINT ( 'NONE',  ( -0.3000000000000000999, -3.941790907013290823, -0.4709369376873030477 ) ) ;
#7894 = EDGE_CURVE ( 'NONE', #38375, #29074, #24900, .T. ) ;
#7895 = PRODUCT_DEFINITION ( 'UNKNOWN', '', #4217, #18226 ) ;
#7896 = AXIS2_PLACEMENT_3D ( 'NONE', #26307, #4669, #13944 ) ;
#7897 = B_SPLINE_CURVE_WITH_KNOTS ( 'NONE', 3,
 ( #16793, #22569, #13086, #35099 ),
 .UNSPECIFIED., .F., .F.,
 ( 4, 4 ),
 ( 3.165573288030121783E-17, 0.0002659535996674141744 ),
 .UNSPECIFIED. ) ;
#7898 = LINE ( 'NONE', #14480, #8106 ) ;
#7899 = CARTESIAN_POINT ( 'NONE',  ( 0.5484265422080265573, -1.662660989552970703, -0.5492187312042384750 ) ) ;
#7900 = ORIENTED_EDGE ( 'NONE', *, *, #3141, .T. ) ;
#7901 = CARTESIAN_POINT ( 'NONE',  ( 0.4692393356387120074, -1.241113899949852550, 0.5778994956701821728 ) ) ;
#7902 = CARTESIAN_POINT ( 'NONE',  ( -0.05634304521267782806, -0.01028134608267022333, -0.4588823192046730948 ) ) ;
#7903 = CARTESIAN_POINT ( 'NONE',  ( -0.05252359774140143156, -0.2829835766811571451, -0.3741004571325397543 ) ) ;
#7904 = VERTEX_POINT ( 'NONE', #12744 ) ;
#7905 = CARTESIAN_POINT ( 'NONE',  ( 0.4530287582269867386, -1.054472822262606968, 0.7183272867302393783 ) ) ;
#7906 = CARTESIAN_POINT ( 'NONE',  ( -0.2399999999999999079, -3.941790907013290823, -0.4709369376873030477 ) ) ;
#7907 = CARTESIAN_POINT ( 'NONE',  ( 0.4001462373468676614, -1.136645747884092783, 0.4743659635294404930 ) ) ;
#7908 = EDGE_CURVE ( 'NONE', #18566, #33923, #13818, .T. ) ;
#7909 = EDGE_CURVE ( 'NONE', #37952, #16265, #24348, .T. ) ;
#7910 = CARTESIAN_POINT ( 'NONE',  ( 0.1275181119306449395, -0.9857185180080264564, 0.6886633007003241103 ) ) ;
#7911 = ORIENTED_EDGE ( 'NONE', *, *, #18438, .T. ) ;
#7912 = DIRECTION ( 'NONE',  ( 1.000000000000000000, 2.341930812374887555E-31, -1.664003471950578127E-31 ) ) ;
#7913 = CARTESIAN_POINT ( 'NONE',  ( 0.6378052450953181074, -1.586953600521664010, -0.4356635440277025206 ) ) ;
#7914 = DIRECTION ( 'NONE',  ( 0.000000000000000000, 3.330669073875470114E-16, 1.000000000000000000 ) ) ;
#7915 = DIRECTION ( 'NONE',  ( 0.000000000000000000, 0.000000000000000000, -1.000000000000000000 ) ) ;
#7916 = CARTESIAN_POINT ( 'NONE',  ( 0.4738421150388607006, -1.247722671731417821, 0.6281918974308814407 ) ) ;
#7918 = DIRECTION ( 'NONE',  ( 0.000000000000000000, 3.557598251760403443E-15, -1.000000000000000000 ) ) ;
#7917 = DIRECTION ( 'NONE',  ( -1.848892746611746419E-32, -0.5237184928541297468, 0.8518913899333638851 ) ) ;
#7919 = CARTESIAN_POINT ( 'NONE',  ( 0.1991581284650917050, -0.9215239498232444815, 0.3071336240427082753 ) ) ;
#7920 = ORIENTED_EDGE ( 'NONE', *, *, #27560, .F. ) ;
#7921 = DIRECTION ( 'NONE',  ( -1.000000000000000000, -0.000000000000000000, -0.000000000000000000 ) ) ;
#7922 = ORIENTED_EDGE ( 'NONE', *, *, #2946, .F. ) ;
#7923 = ADVANCED_FACE ( 'NONE', ( #12535 ), #28945, .T. ) ;
#7924 = DIRECTION ( 'NONE',  ( 0.000000000000000000, -3.414809992080318866E-15, -1.000000000000000000 ) ) ;
#7925 = CARTESIAN_POINT ( 'NONE',  ( 0.4122251433979338686, -1.572231246218684264, 0.7147155659639160552 ) ) ;
#7927 = FACE_BOUND ( 'NONE', #40053, .T. ) ;
#7926 = CARTESIAN_POINT ( 'NONE',  ( 0.08908196101633601705, -0.5887339626514037638, 0.07194673905522250279 ) ) ;
#7928 = CARTESIAN_POINT ( 'NONE',  ( 0.2180524034168905279, -1.623376798655958630, -0.3571287730820865702 ) ) ;
#7929 = VERTEX_POINT ( 'NONE', #9051 ) ;
#7930 = EDGE_CURVE ( 'NONE', #35757, #3317, #2670, .T. ) ;
#7931 = ORIENTED_EDGE ( 'NONE', *, *, #39069, .T. ) ;
#7932 = DIRECTION ( 'NONE',  ( 0.000000000000000000, -0.9510565162951566398, -0.3090169943749374593 ) ) ;
#7933 = ADVANCED_FACE ( 'NONE', ( #37423 ), #26987, .T. ) ;
#7934 = CARTESIAN_POINT ( 'NONE',  ( 0.1193505310152233323, -0.5488392675763952289, 0.1457185332388695187 ) ) ;
#7935 = ORIENTED_EDGE ( 'NONE', *, *, #4932, .T. ) ;
#7936 = CARTESIAN_POINT ( 'NONE',  ( 0.3120958685407360100, -1.764432100645553891, 0.5326512185289294932 ) ) ;
#7937 = CARTESIAN_POINT ( 'NONE',  ( 0.03303737228521656105, -0.4610015631984417106, 0.2426019986921502947 ) ) ;
#7938 = AXIS2_PLACEMENT_3D ( 'NONE', #37184, #18882, #15587 ) ;
#7939 = CARTESIAN_POINT ( 'NONE',  ( 0.3717319392551187152, -1.764663464368710910, -0.4441500688334885094 ) ) ;
#7940 = CARTESIAN_POINT ( 'NONE',  ( 0.2251050016842718604, -1.237046649890439554, 0.5037622129130751025 ) ) ;
#7941 = AXIS2_PLACEMENT_3D ( 'NONE', #1901, #35625, #35836 ) ;
#7942 = CARTESIAN_POINT ( 'NONE',  ( -0.1667768525404941804, 0.4849111360356616052, 0.1246604372685278656 ) ) ;
#7943 = B_SPLINE_CURVE_WITH_KNOTS ( 'NONE', 3,
 ( #21547, #6073, #15352, #34067 ),
 .UNSPECIFIED., .F., .F.,
 ( 4, 4 ),
 ( 0.003748439525988024514, 0.004404120170952528258 ),
 .UNSPECIFIED. ) ;
#7944 = CARTESIAN_POINT ( 'NONE',  ( 0.04293324258486896916, -0.07181764475132801362, 0.4893676133895067393 ) ) ;
#7945 = CARTESIAN_POINT ( 'NONE',  ( 0.4910703360858987843, -1.094828989692585575, 0.8654809858424608038 ) ) ;
#7946 = CARTESIAN_POINT ( 'NONE',  ( 0.1809966328114128720, -1.222385076516254054, -0.5155029497116575543 ) ) ;
#7947 = EDGE_CURVE ( 'NONE', #3369, #5616, #19099, .T. ) ;
#7948 = CARTESIAN_POINT ( 'NONE',  ( 0.03868649100028154209, -0.2522293598345311527, -0.4043344736883377477 ) ) ;
#7950 = CIRCLE ( 'NONE', #32273, 0.1400000000000009570 ) ;
#7949 = CARTESIAN_POINT ( 'NONE',  ( 0.5916862240641643789, -1.591472326627963119, -0.5949256914164438026 ) ) ;
#7951 = ADVANCED_FACE ( 'NONE', ( #18931 ), #27572, .F. ) ;
#7952 = DIRECTION ( 'NONE',  ( 1.188678714063518227E-15, -1.000000000000000000, -3.263080277421930985E-16 ) ) ;
#7953 = CARTESIAN_POINT ( 'NONE',  ( 0.5650875398404070493, -1.618990993344825435, 0.5674743467620558812 ) ) ;
#7954 = CARTESIAN_POINT ( 'NONE',  ( -0.02000000000000000042, -2.631664041040912227, -0.5119035495255163104 ) ) ;
#7955 = CARTESIAN_POINT ( 'NONE',  ( -0.05562144613422700945, 0.4316454521248592191, -0.1615915407302009887 ) ) ;
#7956 = CARTESIAN_POINT ( 'NONE',  ( 0.3098984767712536503, -1.765718780359063267, 0.5682417262808785452 ) ) ;
#7957 = CARTESIAN_POINT ( 'NONE',  ( 0.5713982549016157764, -1.545293902939492314, -0.5110934287108533924 ) ) ;
#7958 = CARTESIAN_POINT ( 'NONE',  ( 0.4251784823825139337, -1.612149241703929148, -0.6654675560951863744 ) ) ;
#7959 = DIRECTION ( 'NONE',  ( -1.000000000000000000, -2.280301054154495132E-31, 1.664003471950577689E-31 ) ) ;
#7960 = CARTESIAN_POINT ( 'NONE',  ( -0.05543910610525103894, -0.2873579635174355329, 0.3608851239303187408 ) ) ;
#7961 = AXIS2_PLACEMENT_3D ( 'NONE', #27547, #30632, #40279 ) ;
#7962 = VERTEX_POINT ( 'NONE', #37626 ) ;
#7963 = EDGE_LOOP ( 'NONE', ( #27393, #22287 ) ) ;
#7964 = CARTESIAN_POINT ( 'NONE',  ( 0.4412150601155225282, -1.069325677854658041, 0.5182417262812423209 ) ) ;
#7965 = CIRCLE ( 'NONE', #13231, 0.5400000000000019229 ) ;
#7966 = DIRECTION ( 'NONE',  ( 0.000000000000000000, 0.000000000000000000, 1.000000000000000000 ) ) ;
#7967 = EDGE_LOOP ( 'NONE', ( #20031, #19222, #24335, #11289 ) ) ;
#7968 = AXIS2_PLACEMENT_3D ( 'NONE', #2978, #28079, #12424 ) ;
#7969 = CARTESIAN_POINT ( 'NONE',  ( 0.4165761542997364897, -1.741708882820427906, 0.5182417262812423209 ) ) ;
#7970 = LINE ( 'NONE', #2434, #11450 ) ;
#7971 = AXIS2_PLACEMENT_3D ( 'NONE', #32010, #9180, #21036 ) ;
#7972 = CARTESIAN_POINT ( 'NONE',  ( 0.4551179479963137764, -1.228091501103429461, 0.7657079515373070855 ) ) ;
#7974 = ORIENTED_EDGE ( 'NONE', *, *, #241, .T. ) ;
#7973 = CARTESIAN_POINT ( 'NONE',  ( -0.1683868308082348830, 0.4901225108767969241, 0.1298109267597974403 ) ) ;
#7975 = CARTESIAN_POINT ( 'NONE',  ( 0.2067623920994063613, -0.8133810345767992223, 0.3693416354660131184 ) ) ;
#7976 = DIRECTION ( 'NONE',  ( 1.000000000000000000, 2.341930812374887555E-31, -1.664003471950578127E-31 ) ) ;
#7977 = ORIENTED_EDGE ( 'NONE', *, *, #13758, .F. ) ;
#7978 = CARTESIAN_POINT ( 'NONE',  ( -0.02000000000000000042, -1.598492537578166672, -0.1971380022280825872 ) ) ;
#7979 = CARTESIAN_POINT ( 'NONE',  ( 0.02381802225809039400, -0.5521116243553858549, 0.2426350268205515748 ) ) ;
#7981 = CARTESIAN_POINT ( 'NONE',  ( 0.1768421950620408245, -0.4866590717709783354, 0.03254264443430439357 ) ) ;
#7980 = CARTESIAN_POINT ( 'NONE',  ( 0.7047269641172427823, -1.495525204603480596, 0.5167404914704131214 ) ) ;
#7982 = CARTESIAN_POINT ( 'NONE',  ( 0.4091335057472371695, -1.131547141905885789, 0.4177417262808780229 ) ) ;
#7983 = EDGE_CURVE ( 'NONE', #35098, #23694, #9888, .T. ) ;
#7984 = DIRECTION ( 'NONE',  ( 0.8660254037844381525, 0.3535533905932748966, -0.3535533905932738974 ) ) ;
#7985 = VERTEX_POINT ( 'NONE', #6361 ) ;
#7986 = DIRECTION ( 'NONE',  ( -7.771561172376107616E-16, 7.170354002788761615E-17, -1.000000000000000000 ) ) ;
#7987 = CARTESIAN_POINT ( 'NONE',  ( 0.1788443422962208706, -1.264928261278998711, 0.4182417262808777458 ) ) ;
#7988 = CARTESIAN_POINT ( 'NONE',  ( 0.03868649100028150045, 0.4417196792138944339, 0.1788567627196042398 ) ) ;
#7989 = CARTESIAN_POINT ( 'NONE',  ( 0.2682412565687398165, -1.183332610994965117, 0.7361391146594850055 ) ) ;
#7990 = CYLINDRICAL_SURFACE ( 'NONE', #24462, 0.04000000000000000777 ) ;
#7991 = ADVANCED_FACE ( 'NONE', ( #31466 ), #2674, .T. ) ;
#7992 = B_SPLINE_CURVE_WITH_KNOTS ( 'NONE', 3,
 ( #20095, #11218, #23784, #36305, #10412, #8127, #32206, #35920, #4021, #22972 ),
 .UNSPECIFIED., .F., .F.,
 ( 4, 2, 2, 2, 4 ),
 ( 0.000000000000000000, 0.0004226723285983043500, 0.0008453446571966087000, 0.001268016985794912996, 0.001690689314393217400 ),
 .UNSPECIFIED. ) ;
#7993 = AXIS2_PLACEMENT_3D ( 'NONE', #31894, #31293, #3104 ) ;
#7994 = DIRECTION ( 'NONE',  ( 1.000000000000000000, 0.000000000000000000, 0.000000000000000000 ) ) ;
#7995 = CARTESIAN_POINT ( 'NONE',  ( 0.2770095578784259605, -1.024149721892290810, 0.6102448670827070876 ) ) ;
#7996 = AXIS2_PLACEMENT_3D ( 'NONE', #38051, #34356, #12153 ) ;
#7997 = DIRECTION ( 'NONE',  ( 1.000000000000000000, 0.000000000000000000, 0.000000000000000000 ) ) ;
#7998 = AXIS2_PLACEMENT_3D ( 'NONE', #12939, #38022, #18483 ) ;
#7999 = PLANE ( 'NONE',  #2109 ) ;
#8000 = CARTESIAN_POINT ( 'NONE',  ( 0.4159916692016358830, -1.069406866067976081, -0.5155029497116575543 ) ) ;
#8001 = LINE ( 'NONE', #23268, #22015 ) ;
#8002 = DATE_AND_TIME ( #32704, #21986 ) ;
#8003 = EDGE_CURVE ( 'NONE', #26509, #22200, #30914, .T. ) ;
#8004 = AXIS2_PLACEMENT_3D ( 'NONE', #23588, #20700, #36106 ) ;
#8005 = EDGE_CURVE ( 'NONE', #12964, #38697, #8876, .T. ) ;
#8006 = CARTESIAN_POINT ( 'NONE',  ( 0.03041512172134077860, -1.119424412222147502, 0.6647272771665519997 ) ) ;
#8007 = CARTESIAN_POINT ( 'NONE',  ( 0.3737684249951603865, -1.152107638635602171, 0.5492107935990235834 ) ) ;
#8008 = DIRECTION ( 'NONE',  ( 1.000000000000000000, 0.000000000000000000, 0.000000000000000000 ) ) ;
#8009 = ORIENTED_EDGE ( 'NONE', *, *, #32015, .T. ) ;
#8010 = CARTESIAN_POINT ( 'NONE',  ( 0.01207743823765780947, -0.4534980189049991339, 0.03415917635198321284 ) ) ;
#8011 = CARTESIAN_POINT ( 'NONE',  ( 0.4004245401938955617, -1.732304313445140576, -0.5960862704056979489 ) ) ;
#8012 = DIRECTION ( 'NONE',  ( -1.000000000000000000, -0.000000000000000000, -0.000000000000000000 ) ) ;
#8013 = CARTESIAN_POINT ( 'NONE',  ( 0.05999999999999990757, 0.6655791756086271160, -0.3865134954953678426 ) ) ;
#8014 = ORIENTED_EDGE ( 'NONE', *, *, #14816, .F. ) ;
#8015 = VERTEX_POINT ( 'NONE', #23027 ) ;
#8016 = CARTESIAN_POINT ( 'NONE',  ( 0.1889207857526494783, -0.5233380428592805389, 0.2298431039531494136 ) ) ;
#8017 = VERTEX_POINT ( 'NONE', #12959 ) ;
#8018 = FACE_OUTER_BOUND ( 'NONE', #8355, .T. ) ;
#8019 = AXIS2_PLACEMENT_3D ( 'NONE', #28109, #37542, #34064 ) ;
#8020 = CARTESIAN_POINT ( 'NONE',  ( 0.1345170253128575577, -0.5648217707619066497, 0.2174971669814429742 ) ) ;
#8022 = EDGE_LOOP ( 'NONE', ( #31111, #36812 ) ) ;
#8021 = CARTESIAN_POINT ( 'NONE',  ( -0.001494616128554601903, -0.8154047748197732481, 0.04990360719771039233 ) ) ;
#8023 = ORIENTED_EDGE ( 'NONE', *, *, #22549, .T. ) ;
#8024 = CARTESIAN_POINT ( 'NONE',  ( 0.3416247111477876963, -1.170278351459675514, 0.4404859988295342088 ) ) ;
#8025 = AXIS2_PLACEMENT_3D ( 'NONE', #19192, #28057, #6827 ) ;
#8026 = SHAPE_REPRESENTATION ( 'Lower Pivot Bracket', ( #27819 ), #23225 ) ;
#8027 = ORIENTED_EDGE ( 'NONE', *, *, #12011, .T. ) ;
#8028 = CARTESIAN_POINT ( 'NONE',  ( 0.2651531704851615157, -1.635780466096735219, 0.7914256539850866856 ) ) ;
#8030 = CARTESIAN_POINT ( 'NONE',  ( 0.4882254327172352304, -1.607754588109558069, -0.3920044576893668697 ) ) ;
#8029 = DIRECTION ( 'NONE',  ( -7.771561172376107616E-16, 7.170354002788761615E-17, -1.000000000000000000 ) ) ;
#8031 = FACE_OUTER_BOUND ( 'NONE', #15072, .T. ) ;
#8032 = CALENDAR_DATE ( 2026, 13, 10 ) ;
#8033 = EDGE_CURVE ( 'NONE', #35412, #7881, #9659, .T. ) ;
#8034 = CARTESIAN_POINT ( 'NONE',  ( 0.5479385918970316460, -1.628670924725093005, 0.5682417262808785452 ) ) ;
#8036 = ORIENTED_EDGE ( 'NONE', *, *, #38776, .T. ) ;
#8035 = ORIENTED_EDGE ( 'NONE', *, *, #12984, .F. ) ;
#8037 = CARTESIAN_POINT ( 'NONE',  ( 0.08509544147734100783, -0.8123111742434817595, 0.1457185332388680477 ) ) ;
#8038 = CARTESIAN_POINT ( 'NONE',  ( 0.05658279881179609228, -1.054191643581903426, 0.7314510373715901181 ) ) ;
#8039 = B_SPLINE_SURFACE_WITH_KNOTS ( 'NONE', 3, 1, ( 
 ( #28395, #40534 ),
 ( #19143, #9064 ),
 ( #25321, #37861 ),
 ( #15842, #31290 ) ),
 .UNSPECIFIED., .F., .F., .F.,
 ( 4, 4 ),
 ( 2, 2 ),
 ( 0.000000000000000000, 1.000000000000000000 ),
 ( 0.000000000000000000, 1.000000000000000000 ),
 .UNSPECIFIED. ) ;
#8040 = CARTESIAN_POINT ( 'NONE',  ( 0.1392922804453227692, -0.7568856236203271859, 0.5828328295004829851 ) ) ;
#8041 = CARTESIAN_POINT ( 'NONE',  ( 0.1161639400603292072, -0.5516103353077059790, 0.1797328180798098418 ) ) ;
#8042 = CARTESIAN_POINT ( 'NONE',  ( 0.06217409799684354282, -1.272787436899851521, 0.6404467018060111538 ) ) ;
#8043 = CARTESIAN_POINT ( 'NONE',  ( -0.1157923916715206808, -0.5295015842444287246, 0.3749999999999999445 ) ) ;
#8044 = CARTESIAN_POINT ( 'NONE',  ( 0.06086249397365642300, -1.332142734742585821, 0.5449151288494504808 ) ) ;
#8045 = CARTESIAN_POINT ( 'NONE',  ( 0.3980399496921868674, -1.697909729581410954, -0.4245199042543691403 ) ) ;
#8046 = CARTESIAN_POINT ( 'NONE',  ( 0.3862110256088813198, -1.731934476144515456, 0.4282538419479027803 ) ) ;
#8047 = DIRECTION ( 'NONE',  ( -1.387778780781449423E-15, -6.590151126658397631E-16, -1.000000000000000000 ) ) ;
#8048 = DIRECTION ( 'NONE',  ( 0.4697114767686426107, -0.8828199865158358195, 0.000000000000000000 ) ) ;
#8049 = DIRECTION ( 'NONE',  ( 1.000000000000000000, 2.341930812374887555E-31, -1.664003471950578127E-31 ) ) ;
#8050 = FACE_OUTER_BOUND ( 'NONE', #39718, .T. ) ;
#8051 = CARTESIAN_POINT ( 'NONE',  ( 0.4367417526623164625, -1.230582192281711507, 0.5840196524529203126 ) ) ;
#8052 = VECTOR ( 'NONE', #21724, 39.37007874015748143 ) ;
#8053 = DIRECTION ( 'NONE',  ( 1.000000000000000000, 0.000000000000000000, 0.000000000000000000 ) ) ;
#8054 = CARTESIAN_POINT ( 'NONE',  ( -0.002083146443013336215, -0.8967360763018585867, 0.1624439089914547774 ) ) ;
#8055 = CARTESIAN_POINT ( 'NONE',  ( 0.2957689212018802527, -0.9454471935599602084, 0.5654756054326123271 ) ) ;
#8056 = DATE_TIME_ROLE ( 'classification_date' ) ;
#8057 = CIRCLE ( 'NONE', #888, 0.01500000000000006016 ) ;
#8058 = CARTESIAN_POINT ( 'NONE',  ( 0.2366026829857577063, -0.6283501033379368383, 0.5457308484972661633 ) ) ;
#8059 = AXIS2_PLACEMENT_3D ( 'NONE', #30792, #2613, #34684 ) ;
#8060 = CIRCLE ( 'NONE', #35648, 0.5302738246768091690 ) ;
#8061 = EDGE_CURVE ( 'NONE', #22311, #8287, #14487, .T. ) ;
#8062 = B_SPLINE_CURVE_WITH_KNOTS ( 'NONE', 3,
 ( #35925, #16998, #29963, #20707, #20297, #39217, #20101, #5047 ),
 .UNSPECIFIED., .F., .F.,
 ( 4, 2, 2, 4 ),
 ( -2.312373376517052359E-05, 0.002683137465569600168, 0.004036268065236973783, 0.005389398664904348699 ),
 .UNSPECIFIED. ) ;
#8063 = CARTESIAN_POINT ( 'NONE',  ( 0.3940698435746058381, -1.648959190003135511, -0.6369338832859893218 ) ) ;
#8064 = DIRECTION ( 'NONE',  ( 0.4999551463232372317, -0.8660512985181133550, 0.000000000000000000 ) ) ;
#8065 = VECTOR ( 'NONE', #25894, 39.37007874015748854 ) ;
#8066 = ORIENTED_EDGE ( 'NONE', *, *, #37674, .T. ) ;
#8067 = CARTESIAN_POINT ( 'NONE',  ( 0.1909286924077255032, -1.257064795538239022, -0.7462941026102624109 ) ) ;
#8068 = CARTESIAN_POINT ( 'NONE',  ( 0.08940845291349239221, -0.9873426107426247489, 0.8215244533732848353 ) ) ;
#8069 = CARTESIAN_POINT ( 'NONE',  ( 0.2130735790700678256, -1.295425452470167604, -0.6217217108911923251 ) ) ;
#8070 = AXIS2_PLACEMENT_3D ( 'NONE', #20876, #33397, #4403 ) ;
#8072 = EDGE_LOOP ( 'NONE', ( #10156, #32032, #20482, #6645 ) ) ;
#8071 = DIRECTION ( 'NONE',  ( 0.4999551463232372317, -0.8660512985181135770, 0.000000000000000000 ) ) ;
#8073 = LINE ( 'NONE', #16943, #17953 ) ;
#8074 = CARTESIAN_POINT ( 'NONE',  ( 0.5932568134822767680, -1.254512724160953940, 0.6928994325643027530 ) ) ;
#8076 = EDGE_LOOP ( 'NONE', ( #20147, #33956, #34296, #8797 ) ) ;
#8075 = ORIENTED_EDGE ( 'NONE', *, *, #6970, .T. ) ;
#8077 = CARTESIAN_POINT ( 'NONE',  ( 0.1462602504189297326, -1.332370281534213996, -0.7166700418499228897 ) ) ;
#8078 = ORIENTED_EDGE ( 'NONE', *, *, #36279, .F. ) ;
#8079 = CARTESIAN_POINT ( 'NONE',  ( 0.06486042810549992599, -1.341249661891149803, 0.5682417262808776570 ) ) ;
#8080 = LINE ( 'NONE', #32975, #1626 ) ;
#8081 = APPROVAL_DATE_TIME ( #19678, #31503 ) ;
#8082 = CIRCLE ( 'NONE', #19901, 0.01000000000000002796 ) ;
#8083 = DIRECTION ( 'NONE',  ( -1.000000000000000000, 0.000000000000000000, -7.847494366974319310E-16 ) ) ;
#8084 = ORIENTED_EDGE ( 'NONE', *, *, #11441, .T. ) ;
#8085 = CARTESIAN_POINT ( 'NONE',  ( 0.1999999999999794720, -2.107936428766273629, -0.2870436526301871627 ) ) ;
#8086 = CARTESIAN_POINT ( 'NONE',  ( 0.1263335340626541570, -0.7187389189354154162, 0.4672226359719474642 ) ) ;
#8087 = AXIS2_PLACEMENT_3D ( 'NONE', #11861, #2220, #15363 ) ;
#8088 = CARTESIAN_POINT ( 'NONE',  ( 0.2933737728020890945, -1.643668813008566598, 0.9134582784372499153 ) ) ;
#8089 = AXIS2_PLACEMENT_3D ( 'NONE', #4280, #10657, #22836 ) ;
#8090 = CARTESIAN_POINT ( 'NONE',  ( 0.1001591510775032695, -0.5752251226639683024, 0.2680392064541395891 ) ) ;
#8092 = CARTESIAN_POINT ( 'NONE',  ( 0.3178512907186139547, -1.645949601790900774, 0.6057417262800831592 ) ) ;
#8091 = CARTESIAN_POINT ( 'NONE',  ( 0.2660355233482954440, -1.634181185541991210, 0.8113338639931253482 ) ) ;
#8093 = CARTESIAN_POINT ( 'NONE',  ( 0.04790779036325637508, -0.9421369883270767076, 0.2396295160170733851 ) ) ;
#8094 = ORIENTED_EDGE ( 'NONE', *, *, #16965, .T. ) ;
#8095 = EDGE_LOOP ( 'NONE', ( #18921, #32820, #12196, #2534, #38687 ) ) ;
#8096 = CARTESIAN_POINT ( 'NONE',  ( 0.05634301242525739661, -0.4332457820339863930, -0.1515812001271571730 ) ) ;
#8097 = CARTESIAN_POINT ( 'NONE',  ( 0.1927624843354359963, -0.4933326792414792772, 0.2922951691234880189 ) ) ;
#8098 = AXIS2_PLACEMENT_3D ( 'NONE', #27864, #29016, #501 ) ;
#8099 = CARTESIAN_POINT ( 'NONE',  ( -0.03478556507500174533, 0.2420934825333293239, -0.4561854036929720024 ) ) ;
#8100 = DIRECTION ( 'NONE',  ( -1.000000000000000000, -2.341930812374887555E-31, 1.664003471950578127E-31 ) ) ;
#8101 = CARTESIAN_POINT ( 'NONE',  ( 0.07852099631351548703, -1.320155556401022334, 0.4758808093597276523 ) ) ;
#8102 = CARTESIAN_POINT ( 'NONE',  ( 0.4223102950200747219, -1.705408558797358864, -0.5055542070596241722 ) ) ;
#8103 = CARTESIAN_POINT ( 'NONE',  ( 0.1093271622263137233, -1.419650973723309173, 0.5472839097051169777 ) ) ;
#8104 = CARTESIAN_POINT ( 'NONE',  ( 0.3219050788564604137, -0.8784703629548025194, 0.6443316309767920247 ) ) ;
#8105 = CARTESIAN_POINT ( 'NONE',  ( 0.3699999999999787903, -2.097675824466503691, -0.4857926189863390753 ) ) ;
#8106 = VECTOR ( 'NONE', #36289, 39.37007874015748143 ) ;
#8107 = CARTESIAN_POINT ( 'NONE',  ( 0.1356432309609771070, -1.347689971048232627, -0.3196700151196194550 ) ) ;
#8108 = DIRECTION ( 'NONE',  ( 1.000000000000000000, 6.779273404243070203E-32, 4.314083075427408311E-32 ) ) ;
#8109 = EDGE_CURVE ( 'NONE', #2485, #9135, #34876, .T. ) ;
#8110 = CARTESIAN_POINT ( 'NONE',  ( 0.4330554116054934899, -1.226567635015945568, 0.6177703434090197065 ) ) ;
#8111 = DIRECTION ( 'NONE',  ( -1.000000000000000000, -0.000000000000000000, -0.000000000000000000 ) ) ;
#8112 = EDGE_CURVE ( 'NONE', #37390, #29909, #34221, .T. ) ;
#8113 = CARTESIAN_POINT ( 'NONE',  ( -0.05543910610525095567, -0.2544236545520495163, -0.3848133000241401036 ) ) ;
#8114 = EDGE_CURVE ( 'NONE', #839, #26723, #16043, .T. ) ;
#8115 = VECTOR ( 'NONE', #7345, 39.37007874015748143 ) ;
#8116 = VECTOR ( 'NONE', #9928, 39.37007874015748143 ) ;
#8117 = ORIENTED_EDGE ( 'NONE', *, *, #15028, .T. ) ;
#8118 = CARTESIAN_POINT ( 'NONE',  ( 0.2909422066436382348, -0.9047456369702350232, 0.5718823244560541363 ) ) ;
#8119 = ADVANCED_FACE ( 'NONE', ( #22422 ), #37482, .T. ) ;
#8120 = FACE_OUTER_BOUND ( 'NONE', #3058, .T. ) ;
#8121 = EDGE_CURVE ( 'NONE', #38403, #21612, #30938, .T. ) ;
#8122 = AXIS2_PLACEMENT_3D ( 'NONE', #27464, #11626, #8715 ) ;
#8123 = CARTESIAN_POINT ( 'NONE',  ( 0.07727056149180543121, -0.9554077429465727134, 0.6485806625480800003 ) ) ;
#8124 = ORIENTED_EDGE ( 'NONE', *, *, #22222, .T. ) ;
#8125 = DIRECTION ( 'NONE',  ( 0.0001066307966871704452, -1.551735798909009237E-06, -0.9999999943137325431 ) ) ;
#8126 = AXIS2_PLACEMENT_3D ( 'NONE', #7000, #25535, #19568 ) ;
#8127 = CARTESIAN_POINT ( 'NONE',  ( 0.3840482169485068265, -1.614345010373418488, -0.3632487003279359916 ) ) ;
#8128 = FACE_OUTER_BOUND ( 'NONE', #28519, .T. ) ;
#8129 = CARTESIAN_POINT ( 'NONE',  ( 0.1836898292508203356, -1.885732359905404332, -0.3111683550142131383 ) ) ;
#8130 = CARTESIAN_POINT ( 'NONE',  ( 0.3962101050479742703, -1.143265633725505159, 0.6995449155040951439 ) ) ;
#8132 = DIRECTION ( 'NONE',  ( 0.4999551463232372872, -0.8660512985181134660, 0.000000000000000000 ) ) ;
#8131 = CARTESIAN_POINT ( 'NONE',  ( -2.070754768975505034, -0.09959325338431362917, 0.3749999999999976130 ) ) ;
#8133 = CARTESIAN_POINT ( 'NONE',  ( 0.5846680594243126583, -1.499425989846573382, -0.5926635984244745803 ) ) ;
#8134 = EDGE_LOOP ( 'NONE', ( #5128, #9708, #8671, #19297, #37580, #21829 ) ) ;
#8135 = CARTESIAN_POINT ( 'NONE',  ( 1.480025787077754007, -0.6872203660140440151, 0.1457185332388702959 ) ) ;
#8136 = EDGE_LOOP ( 'NONE', ( #31236, #33995, #2277, #13999 ) ) ;
#8137 = DIRECTION ( 'NONE',  ( 1.000000000000000000, 0.000000000000000000, 0.000000000000000000 ) ) ;
#8138 = CARTESIAN_POINT ( 'NONE',  ( 0.06179390496056682419, -0.5638175360510637724, 0.2559820944390198694 ) ) ;
#8139 = EDGE_CURVE ( 'NONE', #28193, #28482, #38801, .T. ) ;
#8141 = DIRECTION ( 'NONE',  ( -1.387778780781449620E-15, 6.590151126658376924E-16, -1.000000000000000000 ) ) ;
#8140 = CARTESIAN_POINT ( 'NONE',  ( 0.08737269751878998236, -0.6956646054673948365, 0.02271064067933706646 ) ) ;
#8142 = CARTESIAN_POINT ( 'NONE',  ( -0.2746410161513782033, -1.906460133321048911, -0.3231213194042101278 ) ) ;
#8143 = APPLIED_PERSON_AND_ORGANIZATION_ASSIGNMENT ( #28772, #31043, ( #26625 ) ) ;
#8144 = ORIENTED_EDGE ( 'NONE', *, *, #3906, .T. ) ;
#8145 = DIRECTION ( 'NONE',  ( 0.000000000000000000, 0.000000000000000000, -1.000000000000000000 ) ) ;
#8146 = CARTESIAN_POINT ( 'NONE',  ( 0.5632903408051906924, -1.466070610373608529, 0.7198323889707046730 ) ) ;
#8147 = ORIENTED_EDGE ( 'NONE', *, *, #36423, .T. ) ;
#8148 = CARTESIAN_POINT ( 'NONE',  ( 0.3470125293659282462, -1.126547217955315539, -0.5155029497116575543 ) ) ;
#8149 = CARTESIAN_POINT ( 'NONE',  ( 0.04575106512774491235, -0.4390484599015547218, 0.2110503898921168298 ) ) ;
#8150 = CIRCLE ( 'NONE', #26554, 0.06434668806854085266 ) ;
#8151 = CIRCLE ( 'NONE', #11457, 0.1699999999999995126 ) ;
#8152 = CARTESIAN_POINT ( 'NONE',  ( 0.4100456123093288441, -1.725225710419908021, -0.4268450903248970363 ) ) ;
#8153 = AXIS2_PLACEMENT_3D ( 'NONE', #25126, #16080, #12779 ) ;
#8154 = PRODUCT_DEFINITION_SHAPE ( 'NONE', 'NONE',  #40660 ) ;
#8155 = CARTESIAN_POINT ( 'NONE',  ( 0.2036159742448276078, -1.249513165191289632, 0.4424631886055492291 ) ) ;
#8156 = CARTESIAN_POINT ( 'NONE',  ( -0.1710642718812834251, 0.4986889572247755198, 0.1528658435937002014 ) ) ;
#8157 = DIRECTION ( 'NONE',  ( 1.188678714063518227E-15, -1.000000000000000000, -3.263080277421930985E-16 ) ) ;
#8158 = VECTOR ( 'NONE', #8993, 39.37007874015748143 ) ;
#8159 = CARTESIAN_POINT ( 'NONE',  ( 0.3900547927747317067, -0.9231895138380423749, 0.8021268779562266138 ) ) ;
#8160 = AXIS2_PLACEMENT_3D ( 'NONE', #28354, #224, #627 ) ;
#8161 = CARTESIAN_POINT ( 'NONE',  ( 0.05999999999999990757, -0.4204378267473924402, -0.3721750714917929637 ) ) ;
#8162 = DIRECTION ( 'NONE',  ( -7.771561172376107616E-16, 7.170354002788761615E-17, -1.000000000000000000 ) ) ;
#8163 = CARTESIAN_POINT ( 'NONE',  ( 0.6253849347580197060, -1.612577459345563513, -0.5660843253017027177 ) ) ;
#8164 = CARTESIAN_POINT ( 'NONE',  ( 0.04575106512774668177, 0.3363942840372686205, 0.3523417416125865231 ) ) ;
#8165 = CARTESIAN_POINT ( 'NONE',  ( 0.5963566829781479228, -1.601993569060106148, 0.5937315688595193874 ) ) ;
#8166 = CARTESIAN_POINT ( 'NONE',  ( 0.6909971427696186552, -1.441959902340269384, 0.5038514719706568279 ) ) ;
#8167 = CARTESIAN_POINT ( 'NONE',  ( -0.04582889109739281958, 0.4389390569944021658, -0.2108010426992259212 ) ) ;
#8168 = EDGE_CURVE ( 'NONE', #26563, #25089, #19927, .T. ) ;
#8169 = CARTESIAN_POINT ( 'NONE',  ( 0.3165986513250982903, -1.745708308064116920, 0.7545403346239585307 ) ) ;
#8170 = CARTESIAN_POINT ( 'NONE',  ( 0.5905302434980007620, -1.559944958562061723, -0.4720911378474059727 ) ) ;
#8171 = CIRCLE ( 'NONE', #31188, 0.1999999999999994837 ) ;
#8172 = EDGE_CURVE ( 'NONE', #24406, #27585, #647, .T. ) ;
#8173 = CARTESIAN_POINT ( 'NONE',  ( 0.1585823774922599239, -1.275097463791165175, 0.5547567935354530411 ) ) ;
#8174 = CARTESIAN_POINT ( 'NONE',  ( 0.4751248519516730884, -1.681100737592190031, 0.5628962907142390781 ) ) ;
#8175 = AXIS2_PLACEMENT_3D ( 'NONE', #40227, #2800, #21544 ) ;
#8176 = ADVANCED_FACE ( 'NONE', ( #38233 ), #4289, .F. ) ;
#8177 = AXIS2_PLACEMENT_3D ( 'NONE', #39894, #11713, #3074 ) ;
#8178 = EDGE_LOOP ( 'NONE', ( #25717, #11280, #7454, #1481 ) ) ;
#8179 = CARTESIAN_POINT ( 'NONE',  ( 0.4110292600630488513, -1.110406119314346407, 0.6168944177148723007 ) ) ;
#8180 = AXIS2_PLACEMENT_3D ( 'NONE', #34654, #3183, #9960 ) ;
#8181 = CARTESIAN_POINT ( 'NONE',  ( 0.05560027925352286488, -1.335209592177159843, 0.5707417262808780478 ) ) ;
#8182 = APPLIED_APPROVAL_ASSIGNMENT ( #11684, ( #33833 ) ) ;
#8183 = LINE ( 'NONE', #4672, #34873 ) ;
#8184 = DIRECTION ( 'NONE',  ( 0.3468893892380644495, 0.7396492646828584094, -0.5767033179097805773 ) ) ;
#8185 = CARTESIAN_POINT ( 'NONE',  ( 0.5140872677725584206, -1.316639973194089430, 0.6836467266521880637 ) ) ;
#8187 = EDGE_LOOP ( 'NONE', ( #4930, #17730, #26931, #18355 ) ) ;
#8186 = CARTESIAN_POINT ( 'NONE',  ( -0.1608166228772861250, 0.4995225507410082089, 0.1237952727409504516 ) ) ;
#8188 = CARTESIAN_POINT ( 'NONE',  ( 0.1897950977212392309, -0.7957416484119633759, 0.2611131357175326961 ) ) ;
#8189 = CARTESIAN_POINT ( 'NONE',  ( -0.2746410161513779258, -3.667123564397057667, -0.3682398926280779361 ) ) ;
#8190 = ORIENTED_EDGE ( 'NONE', *, *, #5731, .T. ) ;
#8191 = CARTESIAN_POINT ( 'NONE',  ( 0.3616412802241143476, -1.759290408630900693, -0.5212859374495405484 ) ) ;
#8192 = ORIENTED_EDGE ( 'NONE', *, *, #27855, .F. ) ;
#8193 = CARTESIAN_POINT ( 'NONE',  ( 0.3216690679530037622, -1.512854433007727595, 0.8542683157091821577 ) ) ;
#8194 = EDGE_CURVE ( 'NONE', #6499, #39495, #27658, .T. ) ;
#8196 = CARTESIAN_POINT ( 'NONE',  ( 0.1147432612534843299, -0.4767836783747688711, 0.02771918083247308998 ) ) ;
#8195 = CARTESIAN_POINT ( 'NONE',  ( 0.6967942517794997181, -1.491337617863137455, 0.4846308184134556218 ) ) ;
#8197 = DIRECTION ( 'NONE',  ( -1.000000000000000000, -2.280301054154495132E-31, 1.664003471950577689E-31 ) ) ;
#8198 = CARTESIAN_POINT ( 'NONE',  ( 0.1734515873220548177, -1.267154000006108339, -0.3263956774707204023 ) ) ;
#8199 = ORIENTED_EDGE ( 'NONE', *, *, #13739, .T. ) ;
#8200 = EDGE_LOOP ( 'NONE', ( #39620, #10329, #30905, #1951 ) ) ;
#8201 = CARTESIAN_POINT ( 'NONE',  ( 0.1870725001947720623, -1.259290933580937688, -0.7121575810423941277 ) ) ;
#8202 = CARTESIAN_POINT ( 'NONE',  ( 0.03662792686184341423, 0.4685177067346131263, 0.1089945633920604146 ) ) ;
#8203 = CARTESIAN_POINT ( 'NONE',  ( 0.2494758918748508081, -1.148756062240769094, 0.7454965398781205899 ) ) ;
#8204 = CARTESIAN_POINT ( 'NONE',  ( -2.112273405726188513E-14, -2.097675824466503691, -0.6968677163258658602 ) ) ;
#8205 = AXIS2_PLACEMENT_3D ( 'NONE', #35826, #29648, #35615 ) ;
#8206 = CARTESIAN_POINT ( 'NONE',  ( -2.070754768975509474, -0.09959325338431662678, 0.3750000000000004996 ) ) ;
#8207 = AXIS2_PLACEMENT_3D ( 'NONE', #36891, #27851, #2551 ) ;
#8208 = AXIS2_PLACEMENT_3D ( 'NONE', #36101, #26449, #10820 ) ;
#8209 = DIRECTION ( 'NONE',  ( 0.4999551463232372317, -0.8660512985181135770, 0.000000000000000000 ) ) ;
#8210 = CARTESIAN_POINT ( 'NONE',  ( 0.03113248654051816583, 0.000000000000000000, 0.000000000000000000 ) ) ;
#8211 = CARTESIAN_POINT ( 'NONE',  ( 0.3582174290906561254, -1.160725967328684050, 0.4391212506391878323 ) ) ;
#8212 = CARTESIAN_POINT ( 'NONE',  ( 0.5339261027788213543, -1.567111879318243473, -0.5155029497116575543 ) ) ;
#8213 = DIRECTION ( 'NONE',  ( 2.532366176626899733E-12, -0.3090169943749382364, 0.9510565162951566398 ) ) ;
#8214 = APPROVAL_DATE_TIME ( #14584, #30299 ) ;
#8215 = APPLIED_APPROVAL_ASSIGNMENT ( #14697, ( #30575 ) ) ;
#8216 = CARTESIAN_POINT ( 'NONE',  ( 0.06487940854082643871, -1.341257406870441482, 0.5704520789807075998 ) ) ;
#8217 =( REPRESENTATION_RELATIONSHIP ('NONE','NONE', #27514, #40103 ) REPRESENTATION_RELATIONSHIP_WITH_TRANSFORMATION ( #19885 )SHAPE_REPRESENTATION_RELATIONSHIP( ) );
#8218 = AXIS2_PLACEMENT_3D ( 'NONE', #16017, #1025, #435 ) ;
#8219 = DIRECTION ( 'NONE',  ( -0.08441620754382399283, 0.8288655086680465356, -0.5530423785248094193 ) ) ;
#8220 = EDGE_CURVE ( 'NONE', #22200, #20037, #16855, .T. ) ;
#8221 = CARTESIAN_POINT ( 'NONE',  ( 1.547079322592971316E-05, -0.5132440025857009092, -0.04957435040516270514 ) ) ;
#8222 = LINE ( 'NONE', #26949, #13369 ) ;
#8223 = EDGE_CURVE ( 'NONE', #5597, #37863, #26514, .T. ) ;
#8224 = CARTESIAN_POINT ( 'NONE',  ( 0.01078865671634213208, -0.5493393610439523123, 0.4732676844958878526 ) ) ;
#8225 = FACE_OUTER_BOUND ( 'NONE', #7775, .T. ) ;
#8226 = ORIENTED_EDGE ( 'NONE', *, *, #31394, .F. ) ;
#8227 = VERTEX_POINT ( 'NONE', #7574 ) ;
#8228 = CARTESIAN_POINT ( 'NONE',  ( 0.1822455911001416018, -0.4993161093247819315, 0.08306801194993664039 ) ) ;
#8229 = ORIENTED_EDGE ( 'NONE', *, *, #34158, .T. ) ;
#8230 = CARTESIAN_POINT ( 'NONE',  ( 0.4259907721281001036, -1.086727892038337417, -0.5155029497116575543 ) ) ;
#8231 = CARTESIAN_POINT ( 'NONE',  ( 0.1499999999999996336, 0.3232818887608630010, 0.4449593469062194107 ) ) ;
#8233 = ORIENTED_EDGE ( 'NONE', *, *, #20732, .T. ) ;
#8232 = CARTESIAN_POINT ( 'NONE',  ( 0.008756164835982942901, -0.6361421079842972670, -0.004039510205650067784 ) ) ;
#8234 = VECTOR ( 'NONE', #20832, 39.37007874015748854 ) ;
#8235 = ORIENTED_EDGE ( 'NONE', *, *, #31080, .F. ) ;
#8236 = CARTESIAN_POINT ( 'NONE',  ( 0.3029314534210234000, -0.8887505455264903542, 0.8055725980740405801 ) ) ;
#8237 = EDGE_LOOP ( 'NONE', ( #4520, #7508, #21828, #4489 ) ) ;
#8238 = ADVANCED_FACE ( 'NONE', ( #17046 ), #1400, .T. ) ;
#8239 = CARTESIAN_POINT ( 'NONE',  ( 0.2059273467974228888, -1.283046334493782803, -0.6919850938583151923 ) ) ;
#8241 = CARTESIAN_POINT ( 'NONE',  ( 0.4822264149303859826, -1.608418054921360918, -0.3880980494168181361 ) ) ;
#8240 = DIRECTION ( 'NONE',  ( 0.000000000000000000, -0.5877852522924371659, 0.8090169943749736525 ) ) ;
#8242 = APPLIED_SECURITY_CLASSIFICATION_ASSIGNMENT ( #445, ( #40648 ) ) ;
#8243 = CYLINDRICAL_SURFACE ( 'NONE', #30533, 0.1000000000000000194 ) ;
#8244 = EDGE_CURVE ( 'NONE', #36413, #31881, #11242, .T. ) ;
#8245 = COORDINATED_UNIVERSAL_TIME_OFFSET ( 0, 0, .AHEAD. ) ;
#8246 = CARTESIAN_POINT ( 'NONE',  ( 0.5654596793231598806, -1.618818539163461301, 0.5682417262808788783 ) ) ;
#8248 = ORIENTED_EDGE ( 'NONE', *, *, #21376, .T. ) ;
#8247 = EDGE_LOOP ( 'NONE', ( #23635, #27944, #3244, #5910 ) ) ;
#8249 = EDGE_CURVE ( 'NONE', #30856, #19865, #29492, .T. ) ;
#8250 = CARTESIAN_POINT ( 'NONE',  ( 0.01172053995184539968, -0.7041130843534951778, -0.1131832977452343625 ) ) ;
#8251 = CIRCLE ( 'NONE', #17448, 0.05330708661417339622 ) ;
#8252 = CARTESIAN_POINT ( 'NONE',  ( 0.02390224293416483292, -0.9197127835399234730, 0.5774128202788778585 ) ) ;
#8253 = CARTESIAN_POINT ( 'NONE',  ( 0.1429797709452751697, -0.7177769904828193992, 0.5286191414039091985 ) ) ;
#8254 = CARTESIAN_POINT ( 'NONE',  ( 0.1854231476496841502, -0.8287896031818428044, 0.1136188594679051200 ) ) ;
#8255 = CARTESIAN_POINT ( 'NONE',  ( 0.02999864200428311450, -2.091147118151543083, -0.7263534371344014806 ) ) ;
#8256 = DIRECTION ( 'NONE',  ( 0.4999551463232382309, -0.8660512985181127998, 1.639108796198564242E-15 ) ) ;
#8257 = DIRECTION ( 'NONE',  ( 0.4999551463232372317, -0.8660512985181135770, 0.000000000000000000 ) ) ;
#8258 = CARTESIAN_POINT ( 'NONE',  ( 0.4331046530248302551, -1.588691189085156052, -0.6440782542836179791 ) ) ;
#8259 = CYLINDRICAL_SURFACE ( 'NONE', #7591, 0.1946589359789743512 ) ;
#8260 = CARTESIAN_POINT ( 'NONE',  ( -0.01548846960707524721, -0.4638115001430989648, 0.2459753896937853235 ) ) ;
#8261 = CARTESIAN_POINT ( 'NONE',  ( -0.2789010053595591954, 0.4834754829570393486, 0.3599999999999987654 ) ) ;
#8262 = CARTESIAN_POINT ( 'NONE',  ( 0.3951584779506375211, -1.106112822567272280, 0.6036734362241392704 ) ) ;
#8263 = CARTESIAN_POINT ( 'NONE',  ( 0.4374457586934000219, -1.230173854262892830, 0.5848115461677827476 ) ) ;
#8264 = LENGTH_MEASURE_WITH_UNIT ( LENGTH_MEASURE( 0.02539999999999999897 ), #24525 );
#8265 = AXIS2_PLACEMENT_3D ( 'NONE', #28323, #37575, #197 ) ;
#8266 = AXIS2_PLACEMENT_3D ( 'NONE', #34963, #18942, #13149 ) ;
#8267 = CARTESIAN_POINT ( 'NONE',  ( 0.6268473112825395654, -1.602176188498357190, -0.4542866955106492077 ) ) ;
#8268 = CARTESIAN_POINT ( 'NONE',  ( 0.003124719664520433666, -0.5686731593868930013, 0.1115160683991335139 ) ) ;
#8269 = CARTESIAN_POINT ( 'NONE',  ( 0.4929465528686915454, -1.082715557938388029, 0.5653634300333020279 ) ) ;
#8270 = CARTESIAN_POINT ( 'NONE',  ( 0.06486303625374841009, -1.341253824744560452, 0.5682723891644412273 ) ) ;
#8271 = PERSON_AND_ORGANIZATION_ROLE ( 'creator' ) ;
#8272 = CARTESIAN_POINT ( 'NONE',  ( 0.6100913662829361428, -1.289225211610094401, 0.8693105457786516332 ) ) ;
#8273 = APPLIED_SECURITY_CLASSIFICATION_ASSIGNMENT ( #9595, ( #40656 ) ) ;
#8274 = ADVANCED_FACE ( 'NONE', ( #17841 ), #14352, .F. ) ;
#8275 = B_SPLINE_CURVE_WITH_KNOTS ( 'NONE', 3,
 ( #28840, #13194, #4134, #6599, #22896, #19179, #22282, #26172, #25978, #34795 ),
 .UNSPECIFIED., .F., .F.,
 ( 4, 2, 2, 2, 4 ),
 ( 0.000000000000000000, 0.0005616480656060959548, 0.001123296131212191910, 0.001684944196818287864, 0.002246592262424383819 ),
 .UNSPECIFIED. ) ;
#8276 = CARTESIAN_POINT ( 'NONE',  ( 0.3731218858483254519, -1.618895737510273936, -0.6660657155332145862 ) ) ;
#8277 = EDGE_CURVE ( 'NONE', #20283, #40308, #8183, .T. ) ;
#8278 = AXIS2_PLACEMENT_3D ( 'NONE', #14336, #11467, #33456 ) ;
#8279 = CARTESIAN_POINT ( 'NONE',  ( 0.05269111014006781779, 0.009103832413167858503, -0.4686064687114369631 ) ) ;
#8280 =( BOUNDED_SURFACE ( )  B_SPLINE_SURFACE ( 3, 2, ( 
 ( #7193, #13599, #26161 ),
 ( #38681, #4715, #8011 ),
 ( #1871, #20378, #39483 ),
 ( #16891, #20797, #8421 ),
 ( #29433, #33319, #14591 ),
 ( #20584, #14385, #29628 ),
 ( #20988, #5125, #32906 ),
 ( #1277, #33118, #26764 ),
 ( #39096, #23671, #27161 ),
 ( #4927, #36198, #38875 ) ),
 .UNSPECIFIED., .F., .F., .T. ) 
 B_SPLINE_SURFACE_WITH_KNOTS ( ( 4, 2, 2, 2, 4 ),
 ( 3, 3 ),
 ( 3.523657060577889411E-19, 0.0004886858803072692331, 0.0009773717606145380325, 0.001466057640921806723, 0.001954743521229075631 ),
 ( 0.000000000000000000, 1.000000000000000000 ),
 .UNSPECIFIED. ) 
 GEOMETRIC_REPRESENTATION_ITEM ( )  RATIONAL_B_SPLINE_SURFACE ( (
 ( 1.000000000000000000, 0.7071067811883920973, 1.000000000000000000),
 ( 1.000000000000000000, 0.7381839715666297375, 1.000000000000000000),
 ( 1.000000000000000000, 0.7637209924130993199, 1.000000000000000000),
 ( 1.000000000000000000, 0.8085232108216923175, 1.000000000000000000),
 ( 1.000000000000000000, 0.8280261753706451566, 1.000000000000000000),
 ( 1.000000000000000000, 0.8596601947502618968, 1.000000000000000000),
 ( 1.000000000000000000, 0.8720237471664858964, 1.000000000000000000),
 ( 1.000000000000000000, 0.8878769223232639840, 1.000000000000000000),
 ( 1.000000000000000000, 0.8914915958465460255, 1.000000000000000000),
 ( 1.000000000000000000, 0.8903032814718140342, 1.000000000000000000) ) ) 
 REPRESENTATION_ITEM ( '' )  SURFACE ( )  );
#8281 = VERTEX_POINT ( 'NONE', #10882 ) ;
#8282 = CARTESIAN_POINT ( 'NONE',  ( 0.09999999999997892519, -2.097675824466505023, -0.7286991843995646034 ) ) ;
#8283 = CARTESIAN_POINT ( 'NONE',  ( 0.01410851223904770191, -0.6557637843359752639, 0.5002397451194796618 ) ) ;
#8284 = CARTESIAN_POINT ( 'NONE',  ( 0.1294052168131209490, -0.5750714970858038511, 0.2516657636888773864 ) ) ;
#8285 = CARTESIAN_POINT ( 'NONE',  ( 0.3361824506367084853, -1.634927130874744172, 0.4198097592826174340 ) ) ;
#8287 = VERTEX_POINT ( 'NONE', #20148 ) ;
#8286 = CARTESIAN_POINT ( 'NONE',  ( 0.3901308303885444029, -1.763536657467503321, -0.4831808549932304353 ) ) ;
#8288 = CARTESIAN_POINT ( 'NONE',  ( 0.3296415583488681023, -1.757109584657895907, 0.4726979017080325529 ) ) ;
#8289 = CARTESIAN_POINT ( 'NONE',  ( 0.2968044078846433509, -0.7977486025825716309, 0.6363905851602879027 ) ) ;
#8291 = EDGE_LOOP ( 'NONE', ( #4586, #21774, #2832, #1051 ) ) ;
#8290 = ORIENTED_EDGE ( 'NONE', *, *, #8223, .T. ) ;
#8292 = CARTESIAN_POINT ( 'NONE',  ( 0.1196427001920667699, -1.324177393134752911, -0.6828421133618256533 ) ) ;
#8293 = ORIENTED_EDGE ( 'NONE', *, *, #1666, .F. ) ;
#8294 = DIRECTION ( 'NONE',  ( 0.3468893892380655042, -0.2594111197898628651, 0.9013177145509854160 ) ) ;
#8295 = CARTESIAN_POINT ( 'NONE',  ( 0.2899202446100145880, -1.199999382632172207, 0.4182417262798592827 ) ) ;
#8296 = APPROVAL_ROLE ( '' ) ;
#8297 = CARTESIAN_POINT ( 'NONE',  ( -0.03478556507500055878, 0.4639967941986962163, -0.2267627654641953261 ) ) ;
#8298 = ORIENTED_EDGE ( 'NONE', *, *, #29094, .F. ) ;
#8299 = CARTESIAN_POINT ( 'NONE',  ( -0.2746410161513782033, -1.990692974992658737, -0.4647843861454829528 ) ) ;
#8300 = CIRCLE ( 'NONE', #32606, 0.01499999999999994393 ) ;
#8301 = CARTESIAN_POINT ( 'NONE',  ( 0.1024053258065399929, -0.7484833377281776556, 0.3519811350192522670 ) ) ;
#8302 = CARTESIAN_POINT ( 'NONE',  ( 0.1137005432816620976, -0.9903671524150755578, 0.9280563831205882463 ) ) ;
#8303 = CARTESIAN_POINT ( 'NONE',  ( 0.1413657729933081586, -0.7268754190988079289, 0.5433663266485807553 ) ) ;
#8305 = CARTESIAN_POINT ( 'NONE',  ( -0.01548846960688968731, -0.4638115001435005325, -0.2459753896940882756 ) ) ;
#8304 = CARTESIAN_POINT ( 'NONE',  ( 0.3291103594116518427, -1.757007705610827086, 0.4729914256106402259 ) ) ;
#8306 = CARTESIAN_POINT ( 'NONE',  ( 0.09713336615736777035, -1.305095304553262947, 0.5932891525630709095 ) ) ;
#8307 = APPLIED_SECURITY_CLASSIFICATION_ASSIGNMENT ( #31951, ( #40654 ) ) ;
#8308 = EDGE_LOOP ( 'NONE', ( #3710, #13049, #14054, #15085 ) ) ;
#8309 = ORIENTED_EDGE ( 'NONE', *, *, #23502, .F. ) ;
#8310 = CARTESIAN_POINT ( 'NONE',  ( 0.04582889109739239630, -0.4389390569944004450, -0.2108010426992268926 ) ) ;
#8311 = CARTESIAN_POINT ( 'NONE',  ( 0.3960999722200455042, -0.9602260210612366675, 0.7467566221574177820 ) ) ;
#8312 = AXIS2_PLACEMENT_3D ( 'NONE', #1962, #13864, #35899 ) ;
#8313 = DIRECTION ( 'NONE',  ( 0.4999551463232372317, -0.8660512985181135770, 0.000000000000000000 ) ) ;
#8314 = CARTESIAN_POINT ( 'NONE',  ( 0.4687176343584499305, -1.116552776705967531, 0.5688755853127047679 ) ) ;
#8315 = DIRECTION ( 'NONE',  ( 1.000000000000000000, 0.000000000000000000, 0.000000000000000000 ) ) ;
#8316 = DIRECTION ( 'NONE',  ( -1.387778780781449225E-15, 6.590151126658375938E-16, -1.000000000000000000 ) ) ;
#8317 = CARTESIAN_POINT ( 'NONE',  ( 0.2659700368960441486, -1.559712477108197826, -0.7136488599841258607 ) ) ;
#8318 = CARTESIAN_POINT ( 'NONE',  ( 0.3132663380321701885, -1.175085214117265187, 0.5020501538770495431 ) ) ;
#8319 = CARTESIAN_POINT ( 'NONE',  ( 0.6161168803315352216, -1.293011444959033973, 0.6214722141784767562 ) ) ;
#8320 = CALENDAR_DATE ( 2026, 13, 10 ) ;
#8321 = CARTESIAN_POINT ( 'NONE',  ( -0.1119307826792329957, -0.5115903042181111360, 0.1085569730127855792 ) ) ;
#8322 = CARTESIAN_POINT ( 'NONE',  ( -0.05464101615137796630, -1.682484669133182953, -0.03683853088544701559 ) ) ;
#8323 = VECTOR ( 'NONE', #2713, 39.37007874015748854 ) ;
#8324 = CARTESIAN_POINT ( 'NONE',  ( 0.3690560719070919427, -2.063130292613079231, -0.5133036944193291040 ) ) ;
#8325 = DIRECTION ( 'NONE',  ( 0.4999551463232372317, -0.8660512985181133550, 0.000000000000000000 ) ) ;
#8326 = LINE ( 'NONE', #17178, #19907 ) ;
#8327 = CARTESIAN_POINT ( 'NONE',  ( -0.02242905165739169857, -0.3548958552285863544, -0.3695186750059928360 ) ) ;
#8328 = AXIS2_PLACEMENT_3D ( 'NONE', #39722, #24121, #5343 ) ;
#8329 = APPLIED_APPROVAL_ASSIGNMENT ( #16070, ( #11608 ) ) ;
#8330 = EDGE_LOOP ( 'NONE', ( #5827, #25202, #9753, #12700, #31011, #22428 ) ) ;
#8331 = DIRECTION ( 'NONE',  ( 2.465190328815661892E-32, 1.000000000000000000, 6.656013887802287108E-31 ) ) ;
#8332 = CARTESIAN_POINT ( 'NONE',  ( 0.3247324306352935563, -1.759421949583405365, 0.4854534786567430427 ) ) ;
#8333 = AXIS2_PLACEMENT_3D ( 'NONE', #31078, #31295, #37651 ) ;
#8334 = CARTESIAN_POINT ( 'NONE',  ( 0.06214721934179495005, -0.9131463676375551897, 0.5762997311010702450 ) ) ;
#8335 = VERTEX_POINT ( 'NONE', #27120 ) ;
#8336 = CARTESIAN_POINT ( 'NONE',  ( 0.1614573949321077284, -0.7569534866611321577, 0.1932149833450299559 ) ) ;
#8337 = CARTESIAN_POINT ( 'NONE',  ( 0.02242828275838827656, -0.06992002095336109779, 0.5075510395145186315 ) ) ;
#8338 = CARTESIAN_POINT ( 'NONE',  ( 0.3741198898060815181, -1.763750014703691082, -0.4380172221794854659 ) ) ;
#8339 = CARTESIAN_POINT ( 'NONE',  ( 0.1994740068363786423, -2.042640899752901085, -0.2765909798240093198 ) ) ;
#8340 = CARTESIAN_POINT ( 'NONE',  ( 0.4143713219839447182, -1.164911342593115240, 0.6919132719734564230 ) ) ;
#8342 = DIRECTION ( 'NONE',  ( -0.9750333724971924632, 0.000000000000000000, -0.2220583763715098247 ) ) ;
#8341 = CARTESIAN_POINT ( 'NONE',  ( 0.05076541221973829288, 0.4633004642377209215, 0.09914728473420074406 ) ) ;
#8343 = EDGE_CURVE ( 'NONE', #17938, #27730, #31736, .T. ) ;
#8344 = DIRECTION ( 'NONE',  ( 0.000000000000000000, 0.000000000000000000, -1.000000000000000000 ) ) ;
#8345 = EDGE_LOOP ( 'NONE', ( #30295, #15069, #26923, #35707 ) ) ;
#8346 = ORIENTED_EDGE ( 'NONE', *, *, #1657, .F. ) ;
#8347 = CARTESIAN_POINT ( 'NONE',  ( 0.08099778489142739346, -1.320264099216433173, 0.5551538849635637707 ) ) ;
#8348 = ORIENTED_EDGE ( 'NONE', *, *, #5114, .T. ) ;
#8349 = LINE ( 'NONE', #8538, #4908 ) ;
#8350 = CARTESIAN_POINT ( 'NONE',  ( 0.4352560923565332307, -1.548119695606142265, 0.7308037930344200017 ) ) ;
#8352 = DIRECTION ( 'NONE',  ( -1.355854680848614260E-31, 3.330669073875470114E-16, 1.000000000000000000 ) ) ;
#8351 = CARTESIAN_POINT ( 'NONE',  ( 0.06739980034908768514, -0.6389769636022399890, 0.005946806555783851894 ) ) ;
#8353 = LINE ( 'NONE', #36938, #30315 ) ;
#8354 = VERTEX_POINT ( 'NONE', #32676 ) ;
#8355 = EDGE_LOOP ( 'NONE', ( #34852, #38658, #27353, #1851, #19887 ) ) ;
#8356 = CARTESIAN_POINT ( 'NONE',  ( 0.3930409166178727154, -1.973603618960653838, -0.2924226959962179517 ) ) ;
#8357 = CARTESIAN_POINT ( 'NONE',  ( 0.5739587120820951460, -1.480387852324690057, 0.6855574093161642679 ) ) ;
#8358 = CARTESIAN_POINT ( 'NONE',  ( 0.3352639066339355711, -1.762270631036203516, 0.5634487449406784254 ) ) ;
#8359 = CARTESIAN_POINT ( 'NONE',  ( 0.02999607453758943582, -2.087869005097288788, -0.7252195465745524539 ) ) ;
#8360 = CARTESIAN_POINT ( 'NONE',  ( 0.6435666421574203211, -1.544684378243342593, 0.4182417262808776903 ) ) ;
#8361 = CARTESIAN_POINT ( 'NONE',  ( 0.2053975955868210246, -1.248453031607742458, 0.4579970562924251531 ) ) ;
#8362 = CARTESIAN_POINT ( 'NONE',  ( 0.3991297247951158256, -1.748847237429244528, -0.4900819145088913809 ) ) ;
#8363 = PLANE ( 'NONE',  #33857 ) ;
#8364 = CARTESIAN_POINT ( 'NONE',  ( 0.2064087850599171381, -0.5517209573913892662, 0.4235422224703019323 ) ) ;
#8365 = CARTESIAN_POINT ( 'NONE',  ( 0.07473354200822579507, -1.325658353975272208, 0.4791244499874081075 ) ) ;
#8366 = CARTESIAN_POINT ( 'NONE',  ( -0.1873388932668325069, 0.5325605939836577374, 0.08499999999999950651 ) ) ;
#8367 = CARTESIAN_POINT ( 'NONE',  ( 0.5755826762959820320, -1.611988069552146463, -0.4931026870110623017 ) ) ;
#8368 = CARTESIAN_POINT ( 'NONE',  ( 0.03478489236951365360, 0.2420938338887054231, 0.4561872437641242839 ) ) ;
#8369 = CARTESIAN_POINT ( 'NONE',  ( 0.6275535865577528405, -1.582657856101383098, 0.6191178097732258356 ) ) ;
#8370 = CARTESIAN_POINT ( 'NONE',  ( 0.5943505786846313699, -1.599619272918265445, 0.4280844162099405881 ) ) ;
#8371 = DIRECTION ( 'NONE',  ( -0.8660512985181130219, -0.4999551463232378978, 1.983296656985678775E-15 ) ) ;
#8372 = EDGE_CURVE ( 'NONE', #31015, #23886, #29795, .T. ) ;
#8373 = PRODUCT_DEFINITION ( 'UNKNOWN', '', #39149, #23669 ) ;
#8374 = CARTESIAN_POINT ( 'NONE',  ( 0.1587139193017044758, -1.140357826010188314, 1.006504499293092714 ) ) ;
#8375 = CARTESIAN_POINT ( 'NONE',  ( 0.3808488912321134068, -1.751740863376598067, -0.5696910252506037775 ) ) ;
#8376 = CARTESIAN_POINT ( 'NONE',  ( 0.1457989028442929769, -1.282480442862664161, 0.5557458682560576513 ) ) ;
#8377 = CARTESIAN_POINT ( 'NONE',  ( 0.3048570497350418518, -1.756853555320991189, 0.5694442476137144826 ) ) ;
#8379 = ORIENTED_EDGE ( 'NONE', *, *, #34613, .F. ) ;
#8378 = B_SPLINE_SURFACE_WITH_KNOTS ( 'NONE', 3, 3, ( 
 ( #20394, #14215, #29450, #35613, #20815, #4945, #20200, #4136, #29249, #7823, #26575, #39308, #38897, #32725, #7414, #1292, #20605, #16702, #26783, #13613, #23296, #19992, #36018, #23503, #29645, #11329, #32922, #4345, #36213, #16907, #4732, #26363, #10725, #35822, #1487, #7635, #23899, #4532, #17097, #14005, #39114, #10942, #14402, #17302, #29856, #11129, #23688, #8028, #33136, #17511, #30060, #1890, #26965, #21204, #37243, #5760, #18116, #9244, #27180, #15029, #18318, #17695, #30860, #11738, #21429, #15224, #30241, #33741, #24295, #39710, #24110, #27579, #24498 ),
 ( #11547, #33333, #5552, #2290, #11933, #2071, #14608, #5954, #27991, #2682, #36634, #34145, #39920, #30670, #2489, #8438, #8631, #40105, #27782, #40320, #21004, #24712, #9059, #21621, #8850, #18514, #33524, #12147, #15440, #33960, #5333, #37030, #31069, #2889, #40530, #17895, #5142, #12350, #24908, #37432, #30462, #14829, #27396, #36817, #22646, #31285, #28986, #25935, #25515, #850, #13360, #3097, #9458, #470, #16259, #6979, #28598, #6560, #32082, #16054, #19550, #28187, #28387, #28796, #656, #34960, #52, #25710, #6768, #38241, #18939, #19137, #10072 ),
 ( #19346, #6165, #31884, #256, #9860, #3702, #18728, #9670, #12753, #15640, #12544, #3494, #12967, #3889, #25099, #21820, #37638, #31474, #37855, #31676, #22432, #34753, #3281, #35176, #22037, #38047, #22239, #13146, #16443, #38456, #25315, #34351, #34562, #6371, #15836, #33088, #36170, #26525, #1441, #4084, #16653, #13572, #29202, #7165, #1846, #1062, #17054, #17254, #10674, #13955, #30016, #38653, #35774, #23248, #39065, #35564, #10471, #29407, #26138, #16865, #22856, #26736, #14361, #26925, #35375, #39266, #20555, #14168, #10891, #20354, #7363, #23039, #10291 ),
 ( #19940, #1252, #19733, #11089, #32266, #32474, #4300, #23649, #4897, #7979, #23463, #32875, #13754, #26319, #38845, #17463, #7584, #20159, #32687, #35979, #4492, #4685, #29600, #7785, #29808, #1649, #15175, #2837, #36983, #36375, #17852, #20766, #30621, #18069, #24250, #5902, #2446, #33289, #30817, #39662, #14983, #30202, #8193, #15389, #36772, #5098, #18464, #2033, #33482, #8585, #21160, #11283, #9017, #27345, #31017, #39458, #23850, #27131, #17656, #14564, #11499, #24062, #36589, #39875, #2638, #11884, #33690, #8391, #20962, #5504, #24450, #5288, #8804 ),
 ( #27732, #27537, #18275, #30414, #2245, #40058, #14784, #21382, #33918, #11695, #5717, #40267, #12103, #24669, #37197, #21578, #34100, #22591, #419, #37386, #28747, #34510, #12695, #25258, #21767, #3237, #37800, #22382, #25468, #34301, #19291, #3650, #9619, #16212, #6108, #9405, #18675, #38002, #25049, #12310, #25662, #609, #31835, #15599, #22193, #31238, #9811, #27946, #34708, #10, #15997, #15783, #13102, #12913, #6513, #3835, #3054, #19085, #34909, #24866, #6717, #6320, #38196, #28145, #21982, #28333, #18893, #12492, #37582, #31624, #3439, #10021, #31431 ),
 ( #204, #28544, #35122, #9199, #6926, #19498, #32028, #40484, #25880, #17204, #22984, #1201, #13704, #10234, #32425, #26271, #10842, #13898, #22803, #7739, #32823, #38788, #4629, #35325, #38603, #7115, #26470, #13522, #800, #14119, #29749, #20303, #4034, #10620, #19681, #39006, #16392, #23195, #29144, #4443, #1592, #26691, #32216, #35719, #10422, #1010, #17005, #39224, #11044, #7925, #35931, #20502, #26084, #19888, #35503, #29548, #7532, #23417, #23604, #32638, #36118, #16599, #1386, #33034, #28933, #7311, #20107, #13307, #38398, #4247, #16815, #29359, #36935 ),
 ( #12051, #36731, #26879, #8747, #5053, #8539, #36319, #14320, #21532, #2190, #1804, #24609, #8138, #39609, #30364, #14729, #17410, #15123, #33440, #37147, #8959, #4838, #33246, #39411, #20715, #17614, #29970, #11229, #23801, #30161, #21109, #1988, #14511, #27077, #11445, #24207, #40013, #30766, #11648, #27296, #27681, #39824, #2585, #24011, #36538, #11836, #24396, #18010, #8350, #21325, #30571, #33862, #20920, #33637, #5665, #5248, #5450, #17801, #2396, #14933, #40216, #27489, #18220, #34857, #9767, #25205, #12866, #40627, #34052, #31386, #3001, #3387, #147 ),
 ( #9352, #3191, #22148, #6272, #15549, #6666, #2790, #18846, #21931, #15731, #34458, #28281, #37527, #12640, #15338, #37748, #9570, #16167, #19242, #34664, #6467, #27894, #40431, #37338, #12259, #30964, #25615, #24816, #19037, #362, #31568, #15944, #13064, #21713, #28488, #25427, #37956, #18626, #34247, #12443, #9150, #24996, #5850, #22336, #38146, #9970, #18411, #31784, #3598, #28704, #568, #6059, #31183, #28099, #26645, #23361, #38558, #14069, #6873, #26223, #4195, #16959, #16550, #10381, #16354, #19642, #38960, #39176, #20053, #19448, #959, #3798, #13658 ),
 ( #38745, #28889, #13850, #22749, #10571, #10789, #750, #3987, #13255, #32586, #32176, #31986, #20259, #35882, #26423, #10180, #7262, #25826, #4401, #22540, #16762, #35276, #23145, #7694, #32781, #38345, #19836, #29093, #7071, #35674, #4582, #17154, #35067, #1343, #13469, #26036, #22944, #35461, #7476, #32371, #29503, #29703, #1549, #29310, #1158, #36690, #33806, #11604, #26837, #30308, #27243, #14886, #33395, #39366, #23559, #2346, #11791, #30722, #27445, #11186, #39555, #39774, #24349, #20449, #18168, #15081, #14674, #2543, #27635, #32983, #23746, #2135, #5397 ),
 ( #21270, #11389, #11001, #36077, #7877, #36268, #4790, #1761, #14273, #17364, #29919, #23960, #39970, #24166, #36489, #8090, #20666, #5202, #8496, #33200, #21060, #30114, #17960, #5005, #17572, #8303, #1945, #14461, #27028, #17756, #33587, #8691, #20874, #30519, #36883, #5612, #15500, #37483, #28238, #12400, #9104, #313, #8907, #24954, #28054, #9304, #40580, #21882, #2949, #34411, #21484, #31344, #18793, #22290, #25377, #15687, #3149, #6226, #9722, #102, #37910, #5809, #6010, #6419, #34619, #12599, #18368, #3332, #25158, #15895, #37290, #37698, #28439 ),
 ( #9521, #24561, #22097, #18575, #18987, #30915, #34199, #31519, #31133, #34005, #2739, #12818, #34805, #6609, #15284, #40165, #37092, #21670, #19190, #31729, #3549, #16118, #11995, #27843, #40382, #12207, #24767, #25990, #3940, #38514, #32137, #10345, #38097, #19786, #7218, #10736, #13809, #4143, #32326, #22487, #35012, #31941, #6825, #25569, #20212, #19407, #35424, #35624, #29045, #16713, #7648, #16314, #13415, #913, #29259, #13206, #28849, #7035, #3761, #35234, #525, #4354, #32737, #4544, #13020, #16915, #38908, #32536, #1111, #38707, #25777, #709, #28656 ),
 ( #13619, #29460, #38296, #26184, #23311, #10527, #10128, #23098, #7428, #1304, #22906, #22703, #9916, #20004, #26379, #19604, #35835, #16502, #4958, #33926, #18472, #26591, #24873, #21779, #21389, #37395, #9207, #39129, #4743, #36990, #12110, #2846, #24457, #14991, #24676, #15183, #23515, #9024, #34107, #27544, #5912, #36030, #39320, #7834, #27740, #14228, #1502, #15395, #31024, #21585, #17314, #2454, #10953, #40276, #17109, #11894, #29871, #5726, #27953, #40492, #20405, #40065, #11140, #1710, #18281, #12318, #34308, #29658, #37204, #14016, #26793, #20616, #23699 ),
 ( #32938, #36227, #30825, #8810, #8041, #33152, #18076, #30629, #2645, #22599, #10243, #3659, #3063, #25267, #28153, #38010, #25475, #31634, #13314, #9820, #17, #38206, #6328, #22391, #37593, #15607, #22811, #3449, #12503, #25886, #9414, #211, #16007, #28553, #18684, #16400, #34715, #38405, #6118, #31245, #34518, #25059, #21992, #18902, #31439, #3246, #6521, #10028, #19300, #426, #15793, #28343, #12923, #31842, #12705, #16219, #37809, #616, #9627, #22199, #19094, #34919, #6725, #28756, #13110, #25671, #3844, #35131, #6933, #19506, #32036, #28941, #806 ),
 ( #7934, #29976, #7746, #4042, #36125, #1209, #20116, #32646, #29153, #10630, #1018, #32223, #26888, #13528, #1396, #1600, #35727, #26478, #14326, #22991, #4450, #7540, #39013, #19895, #35513, #13711, #26094, #26279, #7122, #11052, #39418, #11237, #19689, #23611, #4845, #39231, #10849, #4637, #32431, #38609, #35333, #20509, #23203, #16605, #10431, #23423, #17014, #29757, #29367, #29555, #7318, #4256, #33043, #16822, #32832, #38797, #13905, #35940, #20309, #17213, #14127, #1811, #26698, #17418, #15131, #24021, #14943, #14518, #33251, #40443, #21119, #20722, #30972 ),
 ( #8967, #30581, #8547, #34060, #18019, #21542, #30169, #30372, #30776, #18229, #36943, #1997, #27692, #8757, #40225, #20926, #33648, #12060, #27903, #40021, #5061, #21334, #2798, #5860, #11844, #27084, #24622, #37156, #27495, #2593, #2198, #23811, #5458, #33447, #33870, #2404, #17621, #36328, #36738, #5254, #24409, #39619, #11452, #18417, #15346, #5675, #36546, #8146, #14739, #8357, #17811, #27304, #39833, #11654, #24214, #3397, #6068, #25434, #9774, #155, #22347, #18635, #37537, #9157, #15740, #18853, #12650, #31396, #28290, #6282, #25212, #21722, #9579 ),
 ( #34670, #22156, #34254, #31192, #3010, #15558, #28106, #13072, #40634, #37758, #12876, #3198, #6477, #576, #12453, #19045, #31577, #15952, #25004, #9360, #21940, #34467, #28498, #12266, #34864, #25623, #24823, #372, #6673, #16175, #19252, #37965, #31792, #3609, #28713, #37347, #9090, #24333, #40565, #33377, #11979, #30707, #2722, #2330, #36860, #2117, #5380, #24751, #12384, #5795, #5180, #27431, #30284, #40148, #27619, #33788, #15484, #24544, #14651, #40361, #8479, #37074, #39755, #17734, #24939, #5595, #27220, #28037, #11587, #14870, #18153, #2529, #20854 ),
 ( #5993, #24149, #39955, #15268, #27824, #21466, #36671, #12191, #33990, #37273, #17942, #15067, #21656, #8284, #8893, #21040, #18353, #33565, #34183, #30900, #30499, #18559, #31114, #2929, #11775, #8676, #21252, #34789, #6405, #6807, #3533, #31327, #13398, #9706, #18972, #16098, #6206, #18775, #10112, #6593, #31925, #34998, #3133, #28835, #13187, #19174, #25757, #15673, #31505, #28220, #19388, #34602, #21866, #35218, #38282, #693, #25143, #22275, #87, #3743, #37467, #31715, #9501, #25553, #22685, #7019, #12581, #28640, #3314, #22079, #38082, #19584, #32120 ),
 ( #16297, #15878, #37682, #896, #3924, #12797, #29027, #34393, #511, #13005, #16482, #28425, #25360, #298, #37895, #9287, #9900, #22471, #22889, #4337, #7202, #17089, #4524, #10718, #33129, #29638, #19768, #17294, #26167, #1479, #16692, #35408, #1881, #23289, #32306, #4937, #29239, #19983, #35812, #7626, #38497, #36207, #13790, #17504, #30053, #25972, #13605, #4126, #1096, #38690, #10327, #10507, #26357, #29849, #39106, #20193, #23078, #35604, #32718, #10932, #7405, #23495, #16898, #20388, #32515, #29440, #38887, #1284, #13997, #26569, #36011, #7817, #23681 ),
 ( #32915, #4725, #1689, #14207, #26773, #39302, #11122, #20596, #8020, #25387, #9927, #28665, #22496, #16126, #35022, #22107, #38108, #22915, #6833, #10353, #18997, #19199, #19612, #7043, #25785, #31530, #16513, #38307, #29053, #9729, #19414, #923, #16723, #28858, #34626, #10139, #32335, #38521, #717, #3344, #13428, #25999, #3768, #32145, #31740, #12606, #31949, #22299, #22711, #16321, #6427, #29270, #25578, #34815, #13218, #15902, #28448, #4156, #35243, #7229, #37706, #35431, #3558, #3952, #19798, #321, #533, #25166, #9528, #12826, #37919, #6620, #13030 ) ),
 .UNSPECIFIED., .F., .F., .F.,
 ( 4, 3, 3, 3, 3, 3, 4 ),
 ( 4, 3, 3, 3, 3, 3, 3, 3, 3, 3, 3, 3, 3, 3, 3, 3, 3, 3, 3, 3, 3, 3, 3, 3, 4 ),
 ( 0.01801207478348941515, 0.2164687590774609371, 0.4149254433714324453, 0.6133821276654038979, 0.7126104698123896242, 0.7622246408858825983, 0.8118388119593754615 ),
 ( 2.187425721392353805E-15, 0.01572090919976749240, 0.03144181839953279906, 0.04716272759929809877, 0.05502318219918075209, 0.06288363679906340542, 0.09432545519859400485, 0.1257672735981246182, 0.1886509103971858448, 0.2515345471962470714, 0.3773018207943694691, 0.5030690943924919223, 0.6288363679906143755, 0.6917200047896755466, 0.7546036415887367177, 0.8174872783877979998, 0.8803709151868591709, 0.9432545519859203420, 0.9746963703854509831, 0.9904172795852163036, 0.9982777341850990194, 0.9992602910100844005, 1.000242847835069782, 1.002207961485040322, 1.006138188784981624 ),
 .UNSPECIFIED. ) ;
#8380 = SPHERICAL_SURFACE ( 'NONE', #22421, 0.01499999999999999944 ) ;
#8381 = CARTESIAN_POINT ( 'NONE',  ( 0.3965913301904479549, -1.111811593118468222, 0.6217369508112342569 ) ) ;
#8382 = LINE ( 'NONE', #11274, #6179 ) ;
#8383 = CARTESIAN_POINT ( 'NONE',  ( 0.5289571426068226945, -1.341546719958805367, 0.6404369235087098433 ) ) ;
#8385 = ORIENTED_EDGE ( 'NONE', *, *, #1717, .F. ) ;
#8384 = FACE_OUTER_BOUND ( 'NONE', #16426, .T. ) ;
#8386 = CARTESIAN_POINT ( 'NONE',  ( 0.5123549971852071616, -1.116020584419624928, 0.5891410297636010540 ) ) ;
#8387 = ORIENTED_EDGE ( 'NONE', *, *, #34382, .T. ) ;
#8388 = CARTESIAN_POINT ( 'NONE',  ( 0.1499999999999996059, -0.2306506793134098787, -0.4716198300880303784 ) ) ;
#8389 = EDGE_LOOP ( 'NONE', ( #22807, #5800, #33276, #12917 ) ) ;
#8390 = CARTESIAN_POINT ( 'NONE',  ( 0.5462802289783860177, -1.167382474216637878, -0.3984834965322623379 ) ) ;
#8391 = CARTESIAN_POINT ( 'NONE',  ( 0.3559890658834663490, -1.622350306201388648, 0.5721008954271108449 ) ) ;
#8393 = CARTESIAN_POINT ( 'NONE',  ( 0.1883394337541199892, -0.5195054202416713451, 0.1487585982833818932 ) ) ;
#8392 = CARTESIAN_POINT ( 'NONE',  ( 0.7062469264261600488, -1.498219618710284307, 0.5157970235707075579 ) ) ;
#8394 = CYLINDRICAL_SURFACE ( 'NONE', #35241, 0.03749999999977545601 ) ;
#8395 = ORIENTED_EDGE ( 'NONE', *, *, #38297, .T. ) ;
#8396 = ORIENTED_EDGE ( 'NONE', *, *, #20114, .T. ) ;
#8397 = ADVANCED_FACE ( 'NONE', ( #33076 ), #6608, .T. ) ;
#8398 = ORIENTED_EDGE ( 'NONE', *, *, #3854, .F. ) ;
#8399 = CARTESIAN_POINT ( 'NONE',  ( 0.4679778500672936992, -1.237826332153874942, 0.6057417262809768888 ) ) ;
#8400 = ADVANCED_FACE ( 'NONE', ( #17245 ), #1638, .F. ) ;
#8401 = DIRECTION ( 'NONE',  ( 0.4999551463232372317, -0.8660512985181134660, 0.000000000000000000 ) ) ;
#8402 = CARTESIAN_POINT ( 'NONE',  ( 0.1620457668995331502, -0.9696402434604897147, 0.6787910925089855052 ) ) ;
#8403 = LINE ( 'NONE', #20973, #35603 ) ;
#8404 = ADVANCED_FACE ( 'NONE', ( #23235 ), #23452, .T. ) ;
#8405 = CARTESIAN_POINT ( 'NONE',  ( 0.5467981811930779923, -1.652054351292815637, -0.5405695263049933308 ) ) ;
#8406 = EDGE_CURVE ( 'NONE', #32833, #17796, #26345, .T. ) ;
#8407 = ADVANCED_FACE ( 'NONE', ( #11079 ), #3331, .T. ) ;
#8408 = CARTESIAN_POINT ( 'NONE',  ( 0.3700970165061411854, -1.093180069723885151, 0.6366904215209722162 ) ) ;
#8409 = CARTESIAN_POINT ( 'NONE',  ( -0.3000000000000000999, -3.217981293616048344, -0.2530108926800492264 ) ) ;
#8410 = CARTESIAN_POINT ( 'NONE',  ( 0.05562144613422612127, 0.4316454521248598297, 0.1615915407302006557 ) ) ;
#8411 = CARTESIAN_POINT ( 'NONE',  ( -0.02000000000000000042, -2.551729310907437043, -0.5086726180052709712 ) ) ;
#8412 = CARTESIAN_POINT ( 'NONE',  ( 0.008926059106093127415, -1.005466151381485762, 0.5191422350400326513 ) ) ;
#8413 = COORDINATED_UNIVERSAL_TIME_OFFSET ( 0, 0, .AHEAD. ) ;
#8414 = CARTESIAN_POINT ( 'NONE',  ( 0.4598481105376261979, -1.136922751769048112, 0.4503496864651998499 ) ) ;
#8415 = DIRECTION ( 'NONE',  ( -1.000000000000000000, -7.857794173099924470E-32, -8.628166150854818811E-32 ) ) ;
#8416 = DIRECTION ( 'NONE',  ( 0.000000000000000000, 0.000000000000000000, -1.000000000000000000 ) ) ;
#8417 = ADVANCED_FACE ( 'NONE', ( #23639 ), #36195, .T. ) ;
#8418 = ORIENTED_EDGE ( 'NONE', *, *, #30543, .T. ) ;
#8419 = APPLIED_PERSON_AND_ORGANIZATION_ASSIGNMENT ( #40291, #17487, ( #21216 ) ) ;
#8420 = CARTESIAN_POINT ( 'NONE',  ( 0.0004848065072079743576, -0.4386563779232509064, 0.1504137895485508913 ) ) ;
#8421 = CARTESIAN_POINT ( 'NONE',  ( 0.3901692948650766768, -1.742007056135487453, -0.5885189368440594260 ) ) ;
#8422 = CARTESIAN_POINT ( 'NONE',  ( 0.09031319398383846897, -0.9021502138935498794, 0.8729315218264226406 ) ) ;
#8423 = B_SPLINE_CURVE_WITH_KNOTS ( 'NONE', 3,
 ( #1528, #35861, #11367, #4562 ),
 .UNSPECIFIED., .F., .F.,
 ( 4, 4 ),
 ( 0.01056310462781991956, 0.01080186441643053545 ),
 .UNSPECIFIED. ) ;
#8424 = DIRECTION ( 'NONE',  ( -0.9780874495037190641, 0.000000000000000000, 0.2081944790894071917 ) ) ;
#8425 = EDGE_LOOP ( 'NONE', ( #11538, #12046, #32068, #18233 ) ) ;
#8426 = ORIENTED_EDGE ( 'NONE', *, *, #10148, .F. ) ;
#8427 = CARTESIAN_POINT ( 'NONE',  ( 0.1876095839365586326, -1.270310460104812966, 0.4182417262808778013 ) ) ;
#8428 = EDGE_LOOP ( 'NONE', ( #39487, #23795, #20863, #5799 ) ) ;
#8429 = DIRECTION ( 'NONE',  ( -1.110842377313538251E-32, -0.4506112020353472136, -0.8927203059190820245 ) ) ;
#8430 = B_SPLINE_CURVE_WITH_KNOTS ( 'NONE', 3,
 ( #27404, #24507, #11137, #2299 ),
 .UNSPECIFIED., .F., .F.,
 ( 4, 4 ),
 ( 1.301042606982604936E-18, 0.005310656474785389360 ),
 .UNSPECIFIED. ) ;
#8432 = EDGE_LOOP ( 'NONE', ( #37897, #35405, #24155, #27174 ) ) ;
#8431 = CARTESIAN_POINT ( 'NONE',  ( -0.1196081096344516342, -0.4993394475604094884, 0.1302951649420520941 ) ) ;
#8434 = ORIENTED_EDGE ( 'NONE', *, *, #4618, .T. ) ;
#8433 = CARTESIAN_POINT ( 'NONE',  ( 0.007143729570262430731, -0.7929765756790790876, 0.02764597234640707793 ) ) ;
#8435 = ORIENTED_EDGE ( 'NONE', *, *, #28525, .T. ) ;
#8436 = FACE_OUTER_BOUND ( 'NONE', #36805, .T. ) ;
#8437 = EDGE_LOOP ( 'NONE', ( #27492, #34837, #34760, #16247 ) ) ;
#8438 = CARTESIAN_POINT ( 'NONE',  ( 2.342671343675246831E-07, -0.5622830454464696759, 0.2845663875592439052 ) ) ;
#8440 = CARTESIAN_POINT ( 'NONE',  ( 0.1187585920567054698, -1.268575696611346837, 0.6205308943225873453 ) ) ;
#8439 = CARTESIAN_POINT ( 'NONE',  ( -0.03662792686184387220, -0.4431041838557909784, -0.1872093443778377886 ) ) ;
#8441 = FACE_BOUND ( 'NONE', #27390, .T. ) ;
#8442 = DATE_AND_TIME ( #11333, #10966 ) ;
#8443 = CARTESIAN_POINT ( 'NONE',  ( -0.1710642718812830643, 0.4986889572247752977, 0.3079501053856176784 ) ) ;
#8445 = VERTEX_POINT ( 'NONE', #38835 ) ;
#8444 = ORIENTED_EDGE ( 'NONE', *, *, #10314, .T. ) ;
#8446 = CARTESIAN_POINT ( 'NONE',  ( 0.01136143083286298566, -0.9375195846693863411, 0.07874446343318208807 ) ) ;
#8447 = CARTESIAN_POINT ( 'NONE',  ( 0.04816613662790503875, -1.016162693040883580, 0.7049299541483310394 ) ) ;
#8448 = EDGE_CURVE ( 'NONE', #11376, #38403, #390, .T. ) ;
#8449 = CARTESIAN_POINT ( 'NONE',  ( 0.2433285908094565408, -0.9051221626985026525, 0.7049880737946966347 ) ) ;
#8450 = CARTESIAN_POINT ( 'NONE',  ( 0.1873786129353195162, -0.6949979828772413493, 0.03410752346106595695 ) ) ;
#8451 = LINE ( 'NONE', #4960, #2148 ) ;
#8452 = ADVANCED_FACE ( 'NONE', ( #8572 ), #15824, .T. ) ;
#8453 = CARTESIAN_POINT ( 'NONE',  ( 0.3870312468228055414, -1.728124992867544840, -0.4409901392731783165 ) ) ;
#8454 = CARTESIAN_POINT ( 'NONE',  ( 0.3985710665783231410, -1.718231302922667902, 0.4257489112140997456 ) ) ;
#8455 = ADVANCED_FACE ( 'NONE', ( #24438 ), #24655, .T. ) ;
#8456 = CARTESIAN_POINT ( 'NONE',  ( 0.3794276050540705825, -1.663060803246817709, -0.6235637553391095711 ) ) ;
#8457 = FACE_OUTER_BOUND ( 'NONE', #12824, .T. ) ;
#8458 = DIRECTION ( 'NONE',  ( -6.162975822039154046E-33, 0.000000000000000000, -1.000000000000000000 ) ) ;
#8459 = CARTESIAN_POINT ( 'NONE',  ( 0.4602167293986741958, -1.115147919679363220, 0.5809538542335968003 ) ) ;
#8460 = CARTESIAN_POINT ( 'NONE',  ( 0.4358858445580117702, -1.231077702336109247, 0.5834295217759662977 ) ) ;
#8461 = CARTESIAN_POINT ( 'NONE',  ( -0.1749999999999998779, 0.000000000000000000, 0.000000000000000000 ) ) ;
#8462 = B_SPLINE_CURVE_WITH_KNOTS ( 'NONE', 3,
 ( #3019, #2600, #18642, #12274, #37354, #21127, #12459, #9166, #31202, #15139, #25013, #27701, #12068, #5867, #37546, #30378, #9367, #33654 ),
 .UNSPECIFIED., .F., .F.,
 ( 4, 2, 2, 2, 2, 2, 2, 2, 4 ),
 ( 0.006166307077309264237, 0.006694450257964496345, 0.007222593438619729321, 0.007750736619274962297, 0.008278879799930194405, 0.008807022980585426514, 0.009335166161240658622, 0.009863309341895892465, 0.01039145252255112457 ),
 .UNSPECIFIED. ) ;
#8463 = DIRECTION ( 'NONE',  ( -1.000000000000000000, -2.280301054154495132E-31, 1.664003471950577689E-31 ) ) ;
#8464 = CARTESIAN_POINT ( 'NONE',  ( -8.537024980200822558E-17, -0.6872203660140405734, 0.09557912180100291977 ) ) ;
#8465 = CARTESIAN_POINT ( 'NONE',  ( 0.3924682913416943086, -1.027586590250060272, 0.6289202682814357681 ) ) ;
#8466 = CARTESIAN_POINT ( 'NONE',  ( 0.03203312987340298235, -0.9921091887597466297, 0.6716006140561699977 ) ) ;
#8467 = CALENDAR_DATE ( 2026, 13, 10 ) ;
#8468 = CARTESIAN_POINT ( 'NONE',  ( 0.4910703360858987843, -1.094828989692585575, 0.8654809858424608038 ) ) ;
#8469 = ADVANCED_FACE ( 'NONE', ( #15161 ), #36971, .T. ) ;
#8470 = EDGE_CURVE ( 'NONE', #23080, #22141, #21367, .T. ) ;
#8471 = EDGE_CURVE ( 'NONE', #35865, #25611, #27017, .T. ) ;
#8472 = EDGE_CURVE ( 'NONE', #1162, #24445, #18450, .T. ) ;
#8473 = FACE_OUTER_BOUND ( 'NONE', #13616, .T. ) ;
#8474 = CARTESIAN_POINT ( 'NONE',  ( 0.03171861681795883070, 0.07587220456997828544, -0.5191007718638542823 ) ) ;
#8475 = DIRECTION ( 'NONE',  ( 1.000000000000000000, 0.000000000000000000, 8.132394101956133308E-16 ) ) ;
#8476 = EDGE_LOOP ( 'NONE', ( #359, #35280, #19193, #31918 ) ) ;
#8477 = CARTESIAN_POINT ( 'NONE',  ( -0.02000000000000000042, -1.699711333021935777, -0.9366211149475224262 ) ) ;
#8478 = CARTESIAN_POINT ( 'NONE',  ( 0.1655410750827681077, -1.289410180641110459, 0.9375906627650165692 ) ) ;
#8479 = CARTESIAN_POINT ( 'NONE',  ( 0.5879879495906505937, -1.491234220313641057, 0.5743657966556454664 ) ) ;
#8480 = CARTESIAN_POINT ( 'NONE',  ( 0.3738311686567912240, -1.761219272650979883, -0.4365117680794876609 ) ) ;
#8482 = ORIENTED_EDGE ( 'NONE', *, *, #3906, .F. ) ;
#8481 = CARTESIAN_POINT ( 'NONE',  ( 0.3923243630925582481, -1.966611948492517969, -0.4968729097669116745 ) ) ;
#8483 = CARTESIAN_POINT ( 'NONE',  ( 0.6161168803315352216, -1.293011444959033973, 0.6214722141784767562 ) ) ;
#8485 = ORIENTED_EDGE ( 'NONE', *, *, #24647, .T. ) ;
#8484 = EDGE_LOOP ( 'NONE', ( #6986, #23792, #21158, #22694, #38130, #31573 ) ) ;
#8486 = CARTESIAN_POINT ( 'NONE',  ( 0.04054455197037542397, -1.519181945081407248, -0.6711553787198715204 ) ) ;
#8487 = ORIENTED_EDGE ( 'NONE', *, *, #14172, .T. ) ;
#8488 = CARTESIAN_POINT ( 'NONE',  ( 0.3602315267031791501, -1.757724114542561278, -0.5288427849778383205 ) ) ;
#8489 = DIRECTION ( 'NONE',  ( -0.2147743920926303840, -0.9766636885342064867, -4.765223073521777996E-15 ) ) ;
#8490 = DATE_AND_TIME ( #11380, #37208 ) ;
#8491 = CARTESIAN_POINT ( 'NONE',  ( -0.03171893264487601199, 0.4702476704888088332, -0.2325692314474739619 ) ) ;
#8492 = VERTEX_POINT ( 'NONE', #12088 ) ;
#8493 = DIRECTION ( 'NONE',  ( 0.9998941247116547304, -0.01455087607601020412, 0.0001066420868422379633 ) ) ;
#8494 = CARTESIAN_POINT ( 'NONE',  ( 0.09018131941781912242, -0.7099448699386352590, 0.2428910566028353035 ) ) ;
#8495 = CARTESIAN_POINT ( 'NONE',  ( 0.3049302094162430476, -1.696219588324320959, 0.8439175857698040240 ) ) ;
#8496 = CARTESIAN_POINT ( 'NONE',  ( 0.1049909493019218765, -0.6021604844197550044, 0.3340894142283440393 ) ) ;
#8497 = CARTESIAN_POINT ( 'NONE',  ( -0.0001978441549465614934, -0.7095828240749427751, -0.02101536200760643555 ) ) ;
#8498 = CARTESIAN_POINT ( 'NONE',  ( 0.1712463865401376573, -1.267487284506117140, 0.5682417262808779901 ) ) ;
#8499 = ORIENTED_EDGE ( 'NONE', *, *, #8517, .T. ) ;
#8500 = ORIENTED_EDGE ( 'NONE', *, *, #1739, .T. ) ;
#8501 = EDGE_CURVE ( 'NONE', #21610, #2060, #2700, .T. ) ;
#8502 = DIRECTION ( 'NONE',  ( -0.7798479508145914618, 0.000000000000000000, -0.6259689877384361223 ) ) ;
#8503 = B_SPLINE_CURVE_WITH_KNOTS ( 'NONE', 3,
 ( #8092, #14072, #17367, #32588, #1345, #35676, #11003, #39368, #36079, #14463, #38962, #23363 ),
 .UNSPECIFIED., .F., .F.,
 ( 4, 2, 2, 2, 2, 4 ),
 ( 0.000000000000000000, 0.0001072734482993500222, 0.0002145468965987000444, 0.0004290937931974111476, 0.0008581875863948205604, 0.001716375172789631580 ),
 .UNSPECIFIED. ) ;
#8504 = CARTESIAN_POINT ( 'NONE',  ( 0.5757129296766062554, -1.349865815820367354, 0.8829375841553319670 ) ) ;
#8505 = EDGE_CURVE ( 'NONE', #40153, #39497, #16511, .T. ) ;
#8506 = FACE_OUTER_BOUND ( 'NONE', #14597, .T. ) ;
#8507 = CARTESIAN_POINT ( 'NONE',  ( -0.05464101615137796630, -2.070343076906777213, -0.2454056712452573896 ) ) ;
#8508 = CARTESIAN_POINT ( 'NONE',  ( 0.1499999999999993561, 0.000000000000000000, 0.000000000000000000 ) ) ;
#8509 = FACE_OUTER_BOUND ( 'NONE', #22704, .T. ) ;
#8510 = CARTESIAN_POINT ( 'NONE',  ( 0.1554368662221911890, -1.283069701700759513, -0.6964379544131902300 ) ) ;
#8511 = CARTESIAN_POINT ( 'NONE',  ( 0.3208732210860777423, -1.182420994350418697, 0.5690449570999311923 ) ) ;
#8512 = CARTESIAN_POINT ( 'NONE',  ( 0.2495280903959155583, -0.7823963870098056272, 0.5160991521645093005 ) ) ;
#8513 = PERSON_AND_ORGANIZATION ( #28500, #32463 ) ;
#8514 =( BOUNDED_SURFACE ( )  B_SPLINE_SURFACE ( 3, 2, ( 
 ( #20580, #35797, #1273 ),
 ( #33314, #13978, #17672 ),
 ( #29832, #7804, #33109 ),
 ( #26551, #38869, #20180 ),
 ( #17075, #4921, #29622 ),
 ( #39091, #17277, #4710 ),
 ( #5120, #14193, #23482 ),
 ( #32899, #26758, #39286 ),
 ( #11109, #17488, #11522 ),
 ( #5307, #8606, #40081 ),
 ( #27155, #24888, #2470 ),
 ( #18703, #2267, #36611 ),
 ( #17874, #31262, #20983 ),
 ( #18490, #27759, #11909 ),
 ( #8414, #37006, #40292 ),
 ( #12124, #33717, #9039 ),
 ( #21182, #15004, #5530 ),
 ( #30440, #8827, #5741 ),
 ( #14808, #14587, #24085 ),
 ( #30649, #24473, #2659 ),
 ( #24274, #21406, #15199 ),
 ( #15412, #18094, #33941 ),
 ( #33500, #27559, #18298 ),
 ( #24690, #27371, #5926 ),
 ( #30837, #31045, #39896 ),
 ( #11716, #21794, #39686 ),
 ( #34327, #6139, #36797 ),
 ( #37221, #21601, #40508 ),
 ( #34124, #37412, #2864 ),
 ( #27969, #12331, #9222 ) ),
 .UNSPECIFIED., .F., .F., .T. ) 
 B_SPLINE_SURFACE_WITH_KNOTS ( ( 4, 2, 2, 2, 2, 2, 2, 2, 2, 2, 2, 2, 2, 2, 4 ),
 ( 3, 3 ),
 ( -3.469446951953614189E-18, 0.0008451783626492559258, 0.001267767543973885623, 0.001690356725298515321, 0.002112945906623145235, 0.002535535087947774716, 0.002958124269272404197, 0.003380713450597034112, 0.003803302631921664026, 0.004225891813246293940, 0.004648480994570923855, 0.005071070175895552902, 0.005493659357220181949, 0.005916248538544811864, 0.006761426901194071692 ),
 ( 0.000000000000000000, 1.000000000000000000 ),
 .UNSPECIFIED. ) 
 GEOMETRIC_REPRESENTATION_ITEM ( )  RATIONAL_B_SPLINE_SURFACE ( (
 ( 1.000000000000000000, 0.7062849495007544887, 1.000000000000000000),
 ( 1.000000000000000000, 0.7227129208496203550, 1.000000000000000000),
 ( 1.000000000000000000, 0.7446039768329009156, 1.000000000000000000),
 ( 1.000000000000000000, 0.7785882448431576952, 1.000000000000000000),
 ( 1.000000000000000000, 0.7899748008720065551, 1.000000000000000000),
 ( 1.000000000000000000, 0.8124594432436503810, 1.000000000000000000),
 ( 1.000000000000000000, 0.8236310436141200952, 1.000000000000000000),
 ( 1.000000000000000000, 0.8448283019538158634, 1.000000000000000000),
 ( 1.000000000000000000, 0.8549254312217464680, 1.000000000000000000),
 ( 1.000000000000000000, 0.8740472546363526885, 1.000000000000000000),
 ( 1.000000000000000000, 0.8831075751990844491, 1.000000000000000000),
 ( 1.000000000000000000, 0.8995851049065786142, 1.000000000000000000),
 ( 1.000000000000000000, 0.9070756499137949680, 1.000000000000000000),
 ( 1.000000000000000000, 0.9205552158185307254, 1.000000000000000000),
 ( 1.000000000000000000, 0.9265890096043063462, 1.000000000000000000),
 ( 1.000000000000000000, 0.9367297899379105619, 1.000000000000000000),
 ( 1.000000000000000000, 0.9408642172682338822, 1.000000000000000000),
 ( 1.000000000000000000, 0.9471737341364497853, 1.000000000000000000),
 ( 1.000000000000000000, 0.9493269720088893804, 1.000000000000000000),
 ( 1.000000000000000000, 0.9513457469809029066, 1.000000000000000000),
 ( 1.000000000000000000, 0.9512623927072865193, 1.000000000000000000),
 ( 1.000000000000000000, 0.9488501058180722758, 1.000000000000000000),
 ( 1.000000000000000000, 0.9465153709087239520, 1.000000000000000000),
 ( 1.000000000000000000, 0.9398721796748563673, 1.000000000000000000),
 ( 1.000000000000000000, 0.9355047118274805173, 1.000000000000000000),
 ( 1.000000000000000000, 0.9250133594824604399, 1.000000000000000000),
 ( 1.000000000000000000, 0.9189219428161754522, 1.000000000000000000),
 ( 1.000000000000000000, 0.8981866250659263917, 1.000000000000000000),
 ( 1.000000000000000000, 0.8810974021035897774, 1.000000000000000000),
 ( 1.000000000000000000, 0.8619304930065656567, 1.000000000000000000) ) ) 
 REPRESENTATION_ITEM ( '' )  SURFACE ( )  );
#8515 = CARTESIAN_POINT ( 'NONE',  ( 0.3617574415146475042, -1.960072772299676691, -0.4981249426996302576 ) ) ;
#8516 = CARTESIAN_POINT ( 'NONE',  ( 0.3632367524865356967, -1.979769653201874480, -0.4982808577658072724 ) ) ;
#8517 = EDGE_CURVE ( 'NONE', #40111, #2424, #36838, .T. ) ;
#8518 = CARTESIAN_POINT ( 'NONE',  ( 0.02953079040095690777, -0.4684706630666085614, 0.2484463060367459175 ) ) ;
#8519 = CARTESIAN_POINT ( 'NONE',  ( 0.4484726360943441792, -1.685722521223443904, -0.5155029497116575543 ) ) ;
#8520 = LINE ( 'NONE', #34220, #1570 ) ;
#8521 = ORIENTED_EDGE ( 'NONE', *, *, #23599, .T. ) ;
#8522 = CARTESIAN_POINT ( 'NONE',  ( 0.3405654008276560174, -0.9375483805025445205, 0.6383954687273779571 ) ) ;
#8523 = CARTESIAN_POINT ( 'NONE',  ( -2.112273405726188513E-14, -2.097675824466503691, -0.4937760292030871079 ) ) ;
#8524 = CARTESIAN_POINT ( 'NONE',  ( -0.02872242845530507266, 0.07817994906157174628, -0.5268390348591137640 ) ) ;
#8525 = CARTESIAN_POINT ( 'NONE',  ( 0.009566731965422575409, -0.8481436005400048161, 0.2526215923527056484 ) ) ;
#8526 = VERTEX_POINT ( 'NONE', #24854 ) ;
#8527 = DIRECTION ( 'NONE',  ( 0.4999551463232372317, -0.8660512985181135770, 0.000000000000000000 ) ) ;
#8528 = CARTESIAN_POINT ( 'NONE',  ( 0.3264244126186546802, -1.294301107126978767, -0.5166151207188711680 ) ) ;
#8529 = CARTESIAN_POINT ( 'NONE',  ( 0.02953079040094720373, -0.4684706630666299887, -0.2484463060367549936 ) ) ;
#8530 = CARTESIAN_POINT ( 'NONE',  ( 0.4410195951477819398, -1.197182411727151008, 0.6593086987560837775 ) ) ;
#8532 = CARTESIAN_POINT ( 'NONE',  ( 0.001662780879258194885, -0.4326592981238366886, 0.1457185332388686305 ) ) ;
#8531 = CARTESIAN_POINT ( 'NONE',  ( 0.04945776359514829357, 0.4635931069071551058, 0.1136454792236781391 ) ) ;
#8533 = B_SPLINE_CURVE_WITH_KNOTS ( 'NONE', 3,
 ( #3767, #37705, #109, #3154, #3342, #9926 ),
 .UNSPECIFIED., .F., .F.,
 ( 4, 2, 4 ),
 ( 0.000000000000000000, 0.5000000000000000000, 1.000000000000000000 ),
 .UNSPECIFIED. ) ;
#8534 = CARTESIAN_POINT ( 'NONE',  ( 0.01899496522503133639, -0.3622296354306509536, -0.3730445619378164324 ) ) ;
#8535 = ORIENTED_EDGE ( 'NONE', *, *, #28330, .F. ) ;
#8536 = CARTESIAN_POINT ( 'NONE',  ( -0.02953079040095707777, -0.5250338024619264354, 0.07436286310882474215 ) ) ;
#8537 = VERTEX_POINT ( 'NONE', #31421 ) ;
#8538 = CARTESIAN_POINT ( 'NONE',  ( -0.2746410161513776482, -3.838583118162426810, -0.3058907208964237734 ) ) ;
#8539 = CARTESIAN_POINT ( 'NONE',  ( 0.06051550865496472392, -0.5443424548793918127, 0.1927890781605659798 ) ) ;
#8541 = CARTESIAN_POINT ( 'NONE',  ( 0.1994847130146940317, -0.7607898051193093814, 0.3264396457034328125 ) ) ;
#8540 = CARTESIAN_POINT ( 'NONE',  ( -0.04293701532779559127, -0.4875995331660226695, 0.08291810260646308162 ) ) ;
#8542 = DIRECTION ( 'NONE',  ( 0.4999999999999982792, 0.6404870708789264233, -0.5829033470798866690 ) ) ;
#8543 = ORIENTED_EDGE ( 'NONE', *, *, #3885, .F. ) ;
#8544 = EDGE_CURVE ( 'NONE', #8729, #4884, #33906, .T. ) ;
#8545 = ORIENTED_EDGE ( 'NONE', *, *, #25766, .T. ) ;
#8546 = CARTESIAN_POINT ( 'NONE',  ( 0.1847441199961494251, -1.719353529619476184, -0.3282637342952985371 ) ) ;
#8547 = CARTESIAN_POINT ( 'NONE',  ( 0.1223843250744573868, -0.5500287403895844918, 0.1616903350415000440 ) ) ;
#8548 = CARTESIAN_POINT ( 'NONE',  ( 0.6256947331227940001, -1.595527352996821469, 0.6076831429631934789 ) ) ;
#8549 = LINE ( 'NONE', #40446, #31191 ) ;
#8550 = LINE ( 'NONE', #12064, #9341 ) ;
#8551 = CARTESIAN_POINT ( 'NONE',  ( 0.2211220101159939722, -1.227820234045938097, 0.5209104070613070903 ) ) ;
#8552 = AXIS2_PLACEMENT_3D ( 'NONE', #645, #19335, #32070 ) ;
#8553 = FACE_OUTER_BOUND ( 'NONE', #20243, .T. ) ;
#8554 = LINE ( 'NONE', #24221, #15474 ) ;
#8555 = CARTESIAN_POINT ( 'NONE',  ( 0.4624512237511245738, -1.047046041135732741, 0.8530670246638676346 ) ) ;
#8556 = AXIS2_PLACEMENT_3D ( 'NONE', #3273, #21811, #5943 ) ;
#8557 = DIRECTION ( 'NONE',  ( 1.000000000000000000, -0.000000000000000000, -0.000000000000000000 ) ) ;
#8558 = CARTESIAN_POINT ( 'NONE',  ( 0.006240228873519562680, -0.9884989829865254984, 0.4718170318920712480 ) ) ;
#8559 = CARTESIAN_POINT ( 'NONE',  ( 0.6142222766639747755, -1.573946724494656113, -0.5812230652184764423 ) ) ;
#8560 = LINE ( 'NONE', #24638, #27176 ) ;
#8561 = CARTESIAN_POINT ( 'NONE',  ( 0.5824768036646325031, -1.621001158744945991, 0.5712635245953084917 ) ) ;
#8562 = FACE_OUTER_BOUND ( 'NONE', #16304, .T. ) ;
#8563 = CARTESIAN_POINT ( 'NONE',  ( 0.5953197980378833742, -1.599064723402610300, 0.4311035055375501135 ) ) ;
#8564 = ORIENTED_EDGE ( 'NONE', *, *, #34894, .F. ) ;
#8565 = CARTESIAN_POINT ( 'NONE',  ( 0.1802725749815597966, -0.5022333234960129067, 0.1376211838849571434 ) ) ;
#8566 = CARTESIAN_POINT ( 'NONE',  ( 0.4081716264380494952, -1.688076292791299782, -0.6123051696410536371 ) ) ;
#8567 = CARTESIAN_POINT ( 'NONE',  ( -0.3000000000000000999, -3.941790907013290823, -0.4709369376873030477 ) ) ;
#8568 = CARTESIAN_POINT ( 'NONE',  ( 0.3432581181243943846, -1.758429828403793138, 0.5770599949894790193 ) ) ;
#8569 = ORIENTED_EDGE ( 'NONE', *, *, #20978, .F. ) ;
#8570 = DIRECTION ( 'NONE',  ( -0.4999999999999993894, 0.3085698060533125786, 0.8091876635195458523 ) ) ;
#8571 = CARTESIAN_POINT ( 'NONE',  ( 0.3318240906244541710, -1.171642975870005543, 0.5913302545968384116 ) ) ;
#8572 = FACE_OUTER_BOUND ( 'NONE', #24905, .T. ) ;
#8573 = B_SPLINE_CURVE_WITH_KNOTS ( 'NONE', 3,
 ( #16009, #35515, #16824, #23205, #19897, #3661, #32038, #19691, #29369, #12925, #10632, #20118 ),
 .UNSPECIFIED., .F., .F.,
 ( 4, 2, 2, 2, 2, 4 ),
 ( 1.291175088092316414E-16, 0.0008557172854888003312, 0.001283575928233135661, 0.001711434570977471425, 0.002567151856466139050, 0.003422869141954806241 ),
 .UNSPECIFIED. ) ;
#8574 = CARTESIAN_POINT ( 'NONE',  ( 0.4120243698460513970, -1.164832338238820819, 0.7510118434071767490 ) ) ;
#8575 = CONICAL_SURFACE ( 'NONE', #26979, 0.5399999999999999245, 1.211529128687673262 ) ;
#8577 = ORIENTED_EDGE ( 'NONE', *, *, #17315, .T. ) ;
#8576 = DIRECTION ( 'NONE',  ( 0.000000000000000000, 0.000000000000000000, -1.000000000000000000 ) ) ;
#8578 = CARTESIAN_POINT ( 'NONE',  ( 0.5089221226418110255, -1.111225213825750568, 0.6024461477417591970 ) ) ;
#8579 = EDGE_LOOP ( 'NONE', ( #31410, #35164, #38763, #29943 ) ) ;
#8580 = FACE_OUTER_BOUND ( 'NONE', #39100, .T. ) ;
#8581 = ORIENTED_EDGE ( 'NONE', *, *, #22276, .T. ) ;
#8582 = LINE ( 'NONE', #31561, #29101 ) ;
#8583 = VERTEX_POINT ( 'NONE', #37570 ) ;
#8584 = VECTOR ( 'NONE', #2433, 39.37007874015748143 ) ;
#8585 = CARTESIAN_POINT ( 'NONE',  ( 0.3566523005335134333, -1.604465007536034049, 0.7245065946462900808 ) ) ;
#8587 = CARTESIAN_POINT ( 'NONE',  ( 0.1139193472829358872, -0.5653918311555475862, -0.06223708083321360246 ) ) ;
#8586 = DIRECTION ( 'NONE',  ( -1.000000000000000000, -2.276539994720197063E-15, 0.000000000000000000 ) ) ;
#8588 = CARTESIAN_POINT ( 'NONE',  ( -0.2746410161513779258, -4.250025578259899461, -0.8852376261118947154 ) ) ;
#8589 = VECTOR ( 'NONE', #37271, 39.37007874015748143 ) ;
#8590 = AXIS2_PLACEMENT_3D ( 'NONE', #38003, #13308, #16600 ) ;
#8591 = VERTEX_POINT ( 'NONE', #11869 ) ;
#8592 = ORIENTED_EDGE ( 'NONE', *, *, #13765, .T. ) ;
#8593 = CARTESIAN_POINT ( 'NONE',  ( 0.3040981744558501898, -0.9753306080842758519, 0.5622688203834439458 ) ) ;
#8594 = EDGE_LOOP ( 'NONE', ( #582, #17002, #39162, #16060 ) ) ;
#8595 = DIRECTION ( 'NONE',  ( 0.4999551463232372317, -0.8660512985181134660, 0.000000000000000000 ) ) ;
#8596 = LINE ( 'NONE', #37398, #25728 ) ;
#8597 = CARTESIAN_POINT ( 'NONE',  ( 0.2879064663585326755, -1.217751227854929841, 0.7176035333459224175 ) ) ;
#8598 = CARTESIAN_POINT ( 'NONE',  ( 4.823816367165299356E-16, 0.2949999999999992073, 0.06434668806854010326 ) ) ;
#8599 = CARTESIAN_POINT ( 'NONE',  ( -0.1608542991165615721, 0.4995867522469602529, 0.3503927954982317128 ) ) ;
#8600 = PLANE ( 'NONE',  #4113 ) ;
#8601 = CARTESIAN_POINT ( 'NONE',  ( 0.07043814880410684265, -1.334972480813831242, 0.5056242588139928662 ) ) ;
#8602 = CARTESIAN_POINT ( 'NONE',  ( 0.6465835049539362389, -1.539613817736340318, 0.4182417262808776903 ) ) ;
#8603 = DIRECTION ( 'NONE',  ( -1.000000000000000000, -2.280301054154495132E-31, 1.664003471950577689E-31 ) ) ;
#8604 = DATE_AND_TIME ( #39895, #7536 ) ;
#8605 = AXIS2_PLACEMENT_3D ( 'NONE', #12911, #22191, #35322 ) ;
#8606 = CARTESIAN_POINT ( 'NONE',  ( 0.4264195861673160115, -1.139367626797110900, 0.4357676993674804988 ) ) ;
#8607 = AXIS2_PLACEMENT_3D ( 'NONE', #31638, #9824, #19098 ) ;
#8608 = CARTESIAN_POINT ( 'NONE',  ( 0.5565975663448354815, -1.184644286187108708, 0.6057417262809814407 ) ) ;
#8609 = LINE ( 'NONE', #30651, #35644 ) ;
#8610 = TOROIDAL_SURFACE ( 'NONE', #29657, 0.1333070866141734256, 0.02999999999999999889 ) ;
#8611 = CARTESIAN_POINT ( 'NONE',  ( 0.0003124531501750084676, -0.4743565691596361433, 0.01672823577956931637 ) ) ;
#8612 = DIRECTION ( 'NONE',  ( -1.000000000000000000, -2.280301054154495132E-31, 1.664003471950577689E-31 ) ) ;
#8613 = AXIS2_PLACEMENT_3D ( 'NONE', #13189, #25554, #1285 ) ;
#8614 = DIRECTION ( 'NONE',  ( 1.000000000000000000, 0.000000000000000000, 0.000000000000000000 ) ) ;
#8615 = B_SPLINE_CURVE_WITH_KNOTS ( 'NONE', 3,
 ( #31597, #34883, #3029, #12077, #176, #18246, #12467, #2813 ),
 .UNSPECIFIED., .F., .F.,
 ( 4, 2, 2, 4 ),
 ( 2.350980519172206433E-07, 0.001838925622864722624, 0.002758270885271125235, 0.003677616147677528063 ),
 .UNSPECIFIED. ) ;
#8616 = DIRECTION ( 'NONE',  ( 0.4999551463232377313, -0.8660512985181132439, -0.000000000000000000 ) ) ;
#8617 = ORIENTED_EDGE ( 'NONE', *, *, #2259, .F. ) ;
#8618 = EDGE_CURVE ( 'NONE', #37794, #849, #37632, .T. ) ;
#8619 = ORIENTED_EDGE ( 'NONE', *, *, #30344, .F. ) ;
#8620 = CARTESIAN_POINT ( 'NONE',  ( 0.05999999999999990757, -0.1354409211049039941, -0.1857769145426272639 ) ) ;
#8621 = VERTEX_POINT ( 'NONE', #9186 ) ;
#8622 = DIRECTION ( 'NONE',  ( -0.7038049723615886766, -0.4062933899497684909, 0.5827385710266903551 ) ) ;
#8623 = ADVANCED_FACE ( 'NONE', ( #27333 ), #5891, .T. ) ;
#8624 = DIRECTION ( 'NONE',  ( -1.000000000000000000, 0.000000000000000000, 0.000000000000000000 ) ) ;
#8626 = ORIENTED_EDGE ( 'NONE', *, *, #18193, .T. ) ;
#8625 = CARTESIAN_POINT ( 'NONE',  ( 0.009902733472184338873, -0.5495308982465882952, 0.06817473810473409501 ) ) ;
#8627 = ADVANCED_FACE ( 'NONE', ( #19877 ), #23733, .F. ) ;
#8628 = ORIENTED_EDGE ( 'NONE', *, *, #15204, .T. ) ;
#8629 = CYLINDRICAL_SURFACE ( 'NONE', #17269, 0.08000000000000000167 ) ;
#8630 = ORIENTED_EDGE ( 'NONE', *, *, #20483, .T. ) ;
#8631 = CARTESIAN_POINT ( 'NONE',  ( 0.0008771832397133621367, -0.5718434724294755300, 0.3100202370988239808 ) ) ;
#8633 = CARTESIAN_POINT ( 'NONE',  ( 0.1171568423075159127, -1.261316438396035355, 0.6037076130698849630 ) ) ;
#8632 = CARTESIAN_POINT ( 'NONE',  ( -0.04154009738085474857, -0.4416556227939096302, -0.1617111092119922766 ) ) ;
#8634 = DIRECTION ( 'NONE',  ( 0.4999551463232372317, -0.8660512985181135770, 0.000000000000000000 ) ) ;
#8635 = CONTEXT_DEPENDENT_SHAPE_REPRESENTATION ( #6103, #7807 ) ;
#8636 = AXIS2_PLACEMENT_3D ( 'NONE', #27587, #5342, #5153 ) ;
#8637 = CARTESIAN_POINT ( 'NONE',  ( 0.7093866102592447653, -1.464446360347554155, 0.5673451516581958787 ) ) ;
#8639 = VERTEX_POINT ( 'NONE', #28922 ) ;
#8638 = ORIENTED_EDGE ( 'NONE', *, *, #27753, .F. ) ;
#8640 = CARTESIAN_POINT ( 'NONE',  ( 0.3965913301904470112, -1.111811593118468666, 0.6217369508112339238 ) ) ;
#8641 = CARTESIAN_POINT ( 'NONE',  ( 0.1109049718729727962, -0.9286333055842151962, 0.1410250186500828229 ) ) ;
#8642 = CARTESIAN_POINT ( 'NONE',  ( -0.04229883635637818329, -0.4470233673486266324, 0.1406638142521413615 ) ) ;
#8643 = CARTESIAN_POINT ( 'NONE',  ( 0.2297829359340678446, -0.8828613649094588789, 0.6895610511698265777 ) ) ;
#8644 = VECTOR ( 'NONE', #37662, 39.37007874015748143 ) ;
#8645 = CARTESIAN_POINT ( 'NONE',  ( 0.1853695079015652281, -0.8324104521289150682, 0.1224972303491578957 ) ) ;
#8646 = EDGE_CURVE ( 'NONE', #36862, #33486, #30937, .T. ) ;
#8647 = DIRECTION ( 'NONE',  ( -8.881784197001245421E-16, 2.361472542561082612E-16, -1.000000000000000000 ) ) ;
#8648 = DIRECTION ( 'NONE',  ( -0.9378410757839560352, 0.2807814858886596987, 0.2039996905746388478 ) ) ;
#8649 = APPROVAL ( #3674, 'UNSPECIFIED' ) ;
#8650 = AXIS2_PLACEMENT_3D ( 'NONE', #13687, #26452, #10406 ) ;
#8651 = CARTESIAN_POINT ( 'NONE',  ( 0.3724564093243000751, -1.728032324874020143, -0.4192446018103713756 ) ) ;
#8652 = CARTESIAN_POINT ( 'NONE',  ( 0.3891948688262691358, -1.730102521992781694, 0.4274210666962675598 ) ) ;
#8653 = CARTESIAN_POINT ( 'NONE',  ( 0.3402959632056909989, -1.632552626064600609, -0.5940485371126208447 ) ) ;
#8654 = DIRECTION ( 'NONE',  ( 1.000000000000000000, 0.000000000000000000, 0.000000000000000000 ) ) ;
#8655 = DIRECTION ( 'NONE',  ( -1.000000000000000000, 0.000000000000000000, 0.000000000000000000 ) ) ;
#8656 = CARTESIAN_POINT ( 'NONE',  ( 0.4007660105564045949, -1.129975317395211620, 0.6051902615802887686 ) ) ;
#8657 = CYLINDRICAL_SURFACE ( 'NONE', #10199, 0.4614999999999880864 ) ;
#8658 = CARTESIAN_POINT ( 'NONE',  ( -0.009999999999999962044, 0.000000000000000000, 0.000000000000000000 ) ) ;
#8659 = VECTOR ( 'NONE', #15126, 39.37007874015748143 ) ;
#8660 = CARTESIAN_POINT ( 'NONE',  ( 0.03643058821096618188, -0.2291047292463120055, 0.4577947064495202500 ) ) ;
#8661 = CARTESIAN_POINT ( 'NONE',  ( 3.304294434668030104E-05, -0.6893515101347650331, 0.1975634471597359221 ) ) ;
#8662 = CARTESIAN_POINT ( 'NONE',  ( 0.05855645742600570219, -1.102688816132245009, 0.7515070308652079811 ) ) ;
#8663 = APPLICATION_PROTOCOL_DEFINITION ( 'international standard', 'automotive_design', 2000, #37659 ) ;
#8664 = CARTESIAN_POINT ( 'NONE',  ( 0.2690787404081327883, -0.7149439305734058836, 0.6099944544563858928 ) ) ;
#8665 = VECTOR ( 'NONE', #1023, 39.37007874015748854 ) ;
#8666 = CARTESIAN_POINT ( 'NONE',  ( 0.02881195911414601712, 0.06013796869038309789, -0.4945549975361969719 ) ) ;
#8667 = EDGE_CURVE ( 'NONE', #11702, #25265, #6233, .T. ) ;
#8668 = CIRCLE ( 'NONE', #8025, 0.1400000000000009570 ) ;
#8669 = AXIS2_PLACEMENT_3D ( 'NONE', #27963, #37404, #40502 ) ;
#8670 = DIRECTION ( 'NONE',  ( -1.000000000000000000, -7.857794173099924470E-32, -8.628166150854818811E-32 ) ) ;
#8671 = ORIENTED_EDGE ( 'NONE', *, *, #39139, .T. ) ;
#8672 = LINE ( 'NONE', #40562, #4644 ) ;
#8673 = CARTESIAN_POINT ( 'NONE',  ( 0.1160506195841335408, -1.088369628471243633, 0.8769193895170159792 ) ) ;
#8674 = VECTOR ( 'NONE', #8125, 39.37007874015748143 ) ;
#8675 = EDGE_CURVE ( 'NONE', #8899, #641, #11882, .T. ) ;
#8676 = CARTESIAN_POINT ( 'NONE',  ( 0.1751938157831150200, -0.7243946344483128685, 0.5279096736120190148 ) ) ;
#8678 = ORIENTED_EDGE ( 'NONE', *, *, #325, .T. ) ;
#8677 = CARTESIAN_POINT ( 'NONE',  ( 0.2225889308918536924, -1.238345268919997855, 0.5682417262808776570 ) ) ;
#8679 = EDGE_CURVE ( 'NONE', #29543, #19627, #37502, .T. ) ;
#8680 = CARTESIAN_POINT ( 'NONE',  ( 0.2097017171917790468, -0.6397877375661684685, 0.3875311123790295409 ) ) ;
#8682 = ORIENTED_EDGE ( 'NONE', *, *, #17428, .T. ) ;
#8681 = VERTEX_POINT ( 'NONE', #6912 ) ;
#8683 = CARTESIAN_POINT ( 'NONE',  ( 0.5514545221111827322, -1.194714523076736423, 0.8193424885052650319 ) ) ;
#8684 = DIRECTION ( 'NONE',  ( 1.000000000000000000, -0.000000000000000000, -0.000000000000000000 ) ) ;
#8685 = DIRECTION ( 'NONE',  ( -1.000000000000000000, -7.857794173099924470E-32, -8.628166150854818811E-32 ) ) ;
#8686 = CONTEXT_DEPENDENT_SHAPE_REPRESENTATION ( #4540, #10781 ) ;
#8687 = CARTESIAN_POINT ( 'NONE',  ( -0.02881329448201502830, 0.4517642754607751887, -0.2100174381953940073 ) ) ;
#8688 = ORIENTED_EDGE ( 'NONE', *, *, #11422, .F. ) ;
#8689 = CARTESIAN_POINT ( 'NONE',  ( 0.1482573209055756402, -0.8073945103406793278, 0.5257187345872705864 ) ) ;
#8690 = CARTESIAN_POINT ( 'NONE',  ( 0.3111309942001374562, -1.709659708352874619, 0.8393873792776631593 ) ) ;
#8691 = CARTESIAN_POINT ( 'NONE',  ( 0.2632880871822030899, -1.020987797972919164, 0.7882303987144065882 ) ) ;
#8693 = CARTESIAN_POINT ( 'NONE',  ( 0.002149636668525627126, -0.5209811123354256557, 0.1235383891433055742 ) ) ;
#8692 = CARTESIAN_POINT ( 'NONE',  ( -0.01548846960707504251, -0.09061086148575973886, 0.5171215251571027460 ) ) ;
#8694 = ADVANCED_FACE ( 'NONE', ( #19487 ), #32249, .T. ) ;
#8695 = CARTESIAN_POINT ( 'NONE',  ( 0.05041038597642048119, -1.271665433281254032, 0.6452718344857854005 ) ) ;
#8696 = EDGE_LOOP ( 'NONE', ( #10598, #697, #23032 ) ) ;
#8697 = EDGE_CURVE ( 'NONE', #35302, #14209, #23097, .T. ) ;
#8698 = ORIENTED_EDGE ( 'NONE', *, *, #2110, .T. ) ;
#8699 = AXIS2_PLACEMENT_3D ( 'NONE', #1311, #13817, #14025 ) ;
#8700 = CARTESIAN_POINT ( 'NONE',  ( -0.1684323895664706916, 0.5231977504175452376, 0.1471384328909199346 ) ) ;
#8701 = CARTESIAN_POINT ( 'NONE',  ( 0.4281045213691702656, -0.9891014172330019338, 0.8333036199592755988 ) ) ;
#8702 = CARTESIAN_POINT ( 'NONE',  ( 0.2914323826288399699, -1.233685883474753497, -0.5166151207188711680 ) ) ;
#8703 = TOROIDAL_SURFACE ( 'NONE', #31066, 0.05000000000000000971, 0.1700000000000000400 ) ;
#8704 = AXIS2_PLACEMENT_3D ( 'NONE', #5691, #26714, #5476 ) ;
#8705 = DIRECTION ( 'NONE',  ( 0.9480245940703959651, 0.3181970600707381691, 0.000000000000000000 ) ) ;
#8706 = AXIS2_PLACEMENT_3D ( 'NONE', #19730, #37634, #16051 ) ;
#8707 = CARTESIAN_POINT ( 'NONE',  ( 0.3663975874019596568, -1.157438136726378186, 0.4269148889825730708 ) ) ;
#8708 = CARTESIAN_POINT ( 'NONE',  ( 0.2714277091601389746, -1.671900126436688838, 0.5222435141121624103 ) ) ;
#8709 = CARTESIAN_POINT ( 'NONE',  ( 0.3256425937109617141, -1.179684785606091468, 0.5587805044134809274 ) ) ;
#8710 = CARTESIAN_POINT ( 'NONE',  ( 0.5136166297679740644, -1.127695158652323615, 0.6751074532211280843 ) ) ;
#8711 = B_SPLINE_SURFACE_WITH_KNOTS ( 'NONE', 5, 5, ( 
 ( #8181, #4883, #7349, #39048, #1835, #23233 ),
 ( #17243, #35761, #1240, #35968, #20756, #7572 ),
 ( #29396, #26915, #7774, #14155, #19925, #39445 ),
 ( #26725, #39254, #11077, #23637, #11272, #36157 ),
 ( #35549, #23839, #33278, #5085, #30191, #2021 ),
 ( #26126, #4287, #32674, #17044, #10459, #23025 ) ),
 .UNSPECIFIED., .F., .F., .F.,
 ( 6, 6 ),
 ( 6, 6 ),
 ( -6.477000000001651436, 6.477000000001639002 ),
 ( -2.080605796196421498, 4.396394203803585476 ),
 .UNSPECIFIED. ) ;
#8712 = PERSON_AND_ORGANIZATION_ROLE ( 'design_supplier' ) ;
#8713 = CARTESIAN_POINT ( 'NONE',  ( 0.4777184729955372133, -1.099464642909131928, -0.4149595035330911896 ) ) ;
#8714 = AXIS2_PLACEMENT_3D ( 'NONE', #434, #9634, #7128 ) ;
#8715 = DIRECTION ( 'NONE',  ( -1.387778780781449423E-15, 6.590151126658376924E-16, -1.000000000000000000 ) ) ;
#8716 = CARTESIAN_POINT ( 'NONE',  ( -0.1455608194604313677, -0.5249067277714107860, 0.3032895567580803919 ) ) ;
#8717 = CARTESIAN_POINT ( 'NONE',  ( -0.02953079040095591551, -0.3810518745593868273, -0.3687679460475801196 ) ) ;
#8718 = EDGE_CURVE ( 'NONE', #4225, #35619, #34257, .T. ) ;
#8719 = VERTEX_POINT ( 'NONE', #29134 ) ;
#8720 = CARTESIAN_POINT ( 'NONE',  ( 0.3605448558321485697, -1.159604706203796631, 0.5182417262812284431 ) ) ;
#8721 = CARTESIAN_POINT ( 'NONE',  ( -0.05078493045283998669, -0.2374933143169552507, 0.4099093267371753391 ) ) ;
#8722 = AXIS2_PLACEMENT_3D ( 'NONE', #14998, #9215, #27747 ) ;
#8723 = EDGE_CURVE ( 'NONE', #13846, #10925, #19156, .T. ) ;
#8724 = CARTESIAN_POINT ( 'NONE',  ( -2.112273405726188513E-14, -2.104523713476923685, -0.2882857794135356144 ) ) ;
#8725 = EDGE_LOOP ( 'NONE', ( #2727, #39443, #35601, #34546 ) ) ;
#8726 = CARTESIAN_POINT ( 'NONE',  ( -0.05634115714581353074, 0.005221855766568654980, -0.4588864551388210922 ) ) ;
#8727 = CARTESIAN_POINT ( 'NONE',  ( 0.02924548582525025170, -0.9126776490762169569, 0.5652727012340077462 ) ) ;
#8729 = VERTEX_POINT ( 'NONE', #9607 ) ;
#8728 = ORIENTED_EDGE ( 'NONE', *, *, #27890, .T. ) ;
#8730 = CARTESIAN_POINT ( 'NONE',  ( 0.4830258349640542126, -1.691802070263692004, 0.5182417262812423209 ) ) ;
#8731 = AXIS2_PLACEMENT_3D ( 'NONE', #27373, #15414, #27972 ) ;
#8732 = CIRCLE ( 'NONE', #31741, 0.01750000000000001554 ) ;
#8733 = CARTESIAN_POINT ( 'NONE',  ( 0.05634402396114680800, -0.01030784378588360008, 0.4588801752140554968 ) ) ;
#8734 = CARTESIAN_POINT ( 'NONE',  ( 0.7435985525077578595, -1.513373960891965186, 0.6163350003740883931 ) ) ;
#8735 = EDGE_CURVE ( 'NONE', #25046, #40387, #22372, .T. ) ;
#8736 = CARTESIAN_POINT ( 'NONE',  ( 0.3633112630502835505, -1.980641880850154468, -0.4944986277467309788 ) ) ;
#8737 = CARTESIAN_POINT ( 'NONE',  ( 0.4514811354680951516, -1.211986655109367650, 0.6466260521952869045 ) ) ;
#8739 = CARTESIAN_POINT ( 'NONE',  ( 0.2200519516156196342, -1.355113298751763562, 0.5481991913389544502 ) ) ;
#8738 = FACE_OUTER_BOUND ( 'NONE', #12386, .T. ) ;
#8740 = CARTESIAN_POINT ( 'NONE',  ( -0.2399999999999999079, -3.941790907013290823, -0.5334369376873030477 ) ) ;
#8741 = ORIENTED_EDGE ( 'NONE', *, *, #13496, .T. ) ;
#8742 = ORIENTED_EDGE ( 'NONE', *, *, #16286, .F. ) ;
#8743 = DIRECTION ( 'NONE',  ( -5.551115123125856658E-17, 5.007578356027541926E-16, 1.000000000000000000 ) ) ;
#8744 = VERTEX_POINT ( 'NONE', #12903 ) ;
#8745 = AXIS2_PLACEMENT_3D ( 'NONE', #25688, #3077, #38027 ) ;
#8746 = DIRECTION ( 'NONE',  ( 5.551115123125788865E-17, -3.676620095425087714E-16, -1.000000000000000000 ) ) ;
#8747 = CARTESIAN_POINT ( 'NONE',  ( 0.06045611542974323876, -0.5406557321920382186, 0.1728691795844525259 ) ) ;
#8749 = DIRECTION ( 'NONE',  ( 1.000000000000000000, 1.707404996040165152E-15, 0.000000000000000000 ) ) ;
#8748 = CARTESIAN_POINT ( 'NONE',  ( 0.3324871086615504012, -1.659137217475707304, -0.6399689536651966826 ) ) ;
#8750 = DIRECTION ( 'NONE',  ( -1.000000000000000000, 0.000000000000000000, 0.000000000000000000 ) ) ;
#8751 = EDGE_CURVE ( 'NONE', #1392, #27226, #15203, .T. ) ;
#8752 = ORIENTED_EDGE ( 'NONE', *, *, #28244, .T. ) ;
#8753 = APPLIED_PERSON_AND_ORGANIZATION_ASSIGNMENT ( #6220, #96, ( #14861 ) ) ;
#8754 = DIRECTION ( 'NONE',  ( 0.5000000000000019984, 0.6123724356957942483, -0.6123724356957930270 ) ) ;
#8755 = EDGE_CURVE ( 'NONE', #35264, #20946, #18994, .T. ) ;
#8756 = FACE_OUTER_BOUND ( 'NONE', #7573, .T. ) ;
#8757 = CARTESIAN_POINT ( 'NONE',  ( 0.1234749398008549298, -0.5742850910011407795, 0.2528056413081115616 ) ) ;
#8758 = CARTESIAN_POINT ( 'NONE',  ( 0.4452028689750809343, -1.684051297054903307, 0.4425228722054742603 ) ) ;
#8759 = CARTESIAN_POINT ( 'NONE',  ( 0.4069049488313739027, -1.594104043689183570, 0.6057417262804756231 ) ) ;
#8760 =( BOUNDED_SURFACE ( )  B_SPLINE_SURFACE ( 3, 2, ( 
 ( #39270, #1850, #5669 ),
 ( #27685, #15127, #40220 ),
 ( #2589, #5855, #11093 ),
 ( #35982, #31187, #21536 ) ),
 .UNSPECIFIED., .F., .F., .T. ) 
 B_SPLINE_SURFACE_WITH_KNOTS ( ( 4, 4 ),
 ( 3, 3 ),
 ( 0.000000000000000000, 0.001804009323275673022 ),
 ( 0.000000000000000000, 1.000000000000000000 ),
 .UNSPECIFIED. ) 
 GEOMETRIC_REPRESENTATION_ITEM ( )  RATIONAL_B_SPLINE_SURFACE ( (
 ( 1.000000000000000000, 0.7071067811865464625, 1.000000000000000000),
 ( 1.000000000000000000, 0.7071042723947907893, 1.000000000000000000),
 ( 1.000000000000000000, 0.7064338697126849587, 1.000000000000000000),
 ( 1.000000000000000000, 0.7053326528219889813, 1.000000000000000000) ) ) 
 REPRESENTATION_ITEM ( '' )  SURFACE ( )  );
#8761 = VERTEX_POINT ( 'NONE', #25651 ) ;
#8762 = DIRECTION ( 'NONE',  ( 0.000000000000000000, 0.5877852522924840173, 0.8090169943749395687 ) ) ;
#8763 = CARTESIAN_POINT ( 'NONE',  ( 0.2277099777986371920, -1.235451102848944993, 0.5588482542077454207 ) ) ;
#8764 = VECTOR ( 'NONE', #31858, 39.37007874015748143 ) ;
#8765 = DIRECTION ( 'NONE',  ( 0.5000000000000000000, -4.252453317207019391E-31, -0.8660254037844384856 ) ) ;
#8766 = DIRECTION ( 'NONE',  ( 7.771561172376107616E-16, -7.170354002788761615E-17, 1.000000000000000000 ) ) ;
#8767 = CARTESIAN_POINT ( 'NONE',  ( 0.6207796129641102167, -1.305782781463471265, 0.8357864796646383709 ) ) ;
#8768 = AXIS2_PLACEMENT_3D ( 'NONE', #3212, #38372, #25023 ) ;
#8769 = AXIS2_PLACEMENT_3D ( 'NONE', #17039, #7768, #29578 ) ;
#8770 = CARTESIAN_POINT ( 'NONE',  ( -0.04947837552028187119, 0.3081459059633598341, 0.3644550506195312067 ) ) ;
#8771 = CARTESIAN_POINT ( 'NONE',  ( 0.007114566881182543719, -0.9829610562604936819, 0.4921441418150904190 ) ) ;
#8772 = CARTESIAN_POINT ( 'NONE',  ( 0.6140140453192455272, -1.573459653471211528, -0.4496618410196442928 ) ) ;
#8773 = CARTESIAN_POINT ( 'NONE',  ( 0.02999607453758943582, -2.087869005097288788, -0.7252195465745524539 ) ) ;
#8774 = CARTESIAN_POINT ( 'NONE',  ( 0.5704542012684959973, -1.616399117461207569, 0.5772614208947250969 ) ) ;
#8775 = CARTESIAN_POINT ( 'NONE',  ( 0.03158843595483482730, 0.3316344853930308645, -0.3635668653053517052 ) ) ;
#8776 = CONICAL_SURFACE ( 'NONE', #37024, 0.1400000000000009570, 1.047197551196600962 ) ;
#8777 = CARTESIAN_POINT ( 'NONE',  ( 0.3699999999999786793, -2.097675824466503691, -0.4688691127277797022 ) ) ;
#8778 = CIRCLE ( 'NONE', #7451, 0.1000000000000000194 ) ;
#8779 = VERTEX_POINT ( 'NONE', #38182 ) ;
#8780 = DIRECTION ( 'NONE',  ( 1.000000000000000000, 0.000000000000000000, 0.000000000000000000 ) ) ;
#8781 = DIRECTION ( 'NONE',  ( 0.8660512985181134660, 0.4999551463232372317, 0.000000000000000000 ) ) ;
#8782 = CARTESIAN_POINT ( 'NONE',  ( 0.4242202903503162759, -1.646166226851143666, -0.6219045950159559633 ) ) ;
#8783 = EDGE_CURVE ( 'NONE', #4981, #23884, #994, .T. ) ;
#8784 = CARTESIAN_POINT ( 'NONE',  ( 0.4511441812504100035, -1.668355241267087674, -0.6190017437410819667 ) ) ;
#8785 = EDGE_CURVE ( 'NONE', #17955, #24067, #31623, .T. ) ;
#8786 = ORIENTED_EDGE ( 'NONE', *, *, #36423, .F. ) ;
#8787 = CARTESIAN_POINT ( 'NONE',  ( 0.4503105844069756891, -1.094366478625318440, -0.6237232363132070301 ) ) ;
#8788 = CARTESIAN_POINT ( 'NONE',  ( 0.3311563363071323152, -1.162429047844745877, 0.5776872415141406369 ) ) ;
#8789 = CARTESIAN_POINT ( 'NONE',  ( -0.2746410161513782033, -2.183180860297908144, -0.4937760292030871079 ) ) ;
#8790 = B_SPLINE_CURVE_WITH_KNOTS ( 'NONE', 5,
 ( #21843, #34582, #3111, #8872, #6184, #15655 ),
 .UNSPECIFIED., .F., .F.,
 ( 6, 6 ),
 ( 0.2521360130142110134, 0.5291905289985323613 ),
 .UNSPECIFIED. ) ;
#8791 = CARTESIAN_POINT ( 'NONE',  ( 0.05268932808079795915, 0.2680477706051491715, -0.3844863582443084349 ) ) ;
#8792 = AXIS2_PLACEMENT_3D ( 'NONE', #22846, #20149, #3880 ) ;
#8793 = CARTESIAN_POINT ( 'NONE',  ( 0.4594999264872952072, -1.231639012166720004, 0.7236424862120242052 ) ) ;
#8795 = VERTEX_POINT ( 'NONE', #23404 ) ;
#8794 = LINE ( 'NONE', #24442, #21981 ) ;
#8796 = CARTESIAN_POINT ( 'NONE',  ( 0.3793958449840821867, -1.004087596663555848, 0.6383754926613092184 ) ) ;
#8797 = ORIENTED_EDGE ( 'NONE', *, *, #8718, .F. ) ;
#8798 = PERSON_AND_ORGANIZATION ( #28500, #32463 ) ;
#8799 = DIRECTION ( 'NONE',  ( 1.000000000000000000, -3.406373435249580326E-19, 7.771561172376097755E-16 ) ) ;
#8800 = ORIENTED_EDGE ( 'NONE', *, *, #20792, .F. ) ;
#8801 = CARTESIAN_POINT ( 'NONE',  ( -0.02869942827333593627, 0.3396431753871648751, -0.3648167270360638814 ) ) ;
#8802 = AXIS2_PLACEMENT_3D ( 'NONE', #20902, #2371, #36713 ) ;
#8803 = CIRCLE ( 'NONE', #6152, 0.02999999999999998848 ) ;
#8804 = CARTESIAN_POINT ( 'NONE',  ( 0.3552119812245919106, -1.622044444526105522, 0.5608365975959591632 ) ) ;
#8806 = CARTESIAN_POINT ( 'NONE',  ( 0.1120118048860820614, -0.8483571591711281945, -0.03450342869453253136 ) ) ;
#8805 = CARTESIAN_POINT ( 'NONE',  ( -0.1044460467970230316, -0.4741855622371820567, 0.3602693341844401265 ) ) ;
#8807 = DIRECTION ( 'NONE',  ( -0.9378410757839568124, -0.2807814858886553133, 0.2039996905746412070 ) ) ;
#8808 = VERTEX_POINT ( 'NONE', #11430 ) ;
#8809 = CARTESIAN_POINT ( 'NONE',  ( 0.4020964902746486658, -1.115374752730860841, 0.6163322898183211107 ) ) ;
#8810 = CARTESIAN_POINT ( 'NONE',  ( 0.1161887176043710779, -0.5502801146938044452, 0.1708140022945554004 ) ) ;
#8811 = VERTEX_POINT ( 'NONE', #4826 ) ;
#8812 = AXIS2_PLACEMENT_3D ( 'NONE', #3606, #15555, #369 ) ;
#8813 = CARTESIAN_POINT ( 'NONE',  ( 0.1371954450951175242, -1.846940070490806773, -0.3495212765556848233 ) ) ;
#8814 = CARTESIAN_POINT ( 'NONE',  ( -0.02000000000000000042, -2.183180860297908144, -0.4937760292030871079 ) ) ;
#8815 = AXIS2_PLACEMENT_3D ( 'NONE', #37494, #9316, #25172 ) ;
#8816 = DIRECTION ( 'NONE',  ( -0.8660254037844401509, -0.2682606777263719100, 0.4219433715391024964 ) ) ;
#8817 = EDGE_CURVE ( 'NONE', #11734, #858, #13081, .T. ) ;
#8818 = DIRECTION ( 'NONE',  ( 0.4999999999999943379, -0.3297230132044419726, -0.8008013077932559787 ) ) ;
#8819 = CARTESIAN_POINT ( 'NONE',  ( 0.6540709664215760277, -1.593060928864740156, 0.5182417262812423209 ) ) ;
#8820 = CARTESIAN_POINT ( 'NONE',  ( 0.3927915226382389657, -1.715293516864650147, 0.5707417262808793801 ) ) ;
#8821 = FACE_OUTER_BOUND ( 'NONE', #26825, .T. ) ;
#8822 = CARTESIAN_POINT ( 'NONE',  ( 0.4265404446467185307, -1.123912635142109817, 0.5182417262812248904 ) ) ;
#8823 = CARTESIAN_POINT ( 'NONE',  ( 0.04695358122948785351, -1.249483587492180581, 0.6552810377283075915 ) ) ;
#8824 = APPLICATION_PROTOCOL_DEFINITION ( 'international standard', 'automotive_design', 2000, #36329 ) ;
#8825 = VECTOR ( 'NONE', #9098, 39.37007874015748854 ) ;
#8826 = TOROIDAL_SURFACE ( 'NONE', #6843, 0.08830708661417323302, 0.01499999999999999944 ) ;
#8827 = CARTESIAN_POINT ( 'NONE',  ( 0.4741765585715493336, -1.132356602107696952, 0.4721259381520144793 ) ) ;
#8828 = FACE_OUTER_BOUND ( 'NONE', #3711, .T. ) ;
#8829 = DIRECTION ( 'NONE',  ( 1.000000000000000000, 2.280301054154495132E-31, -1.664003471950577689E-31 ) ) ;
#8830 = TOROIDAL_SURFACE ( 'NONE', #14084, 0.08249999999977555842, 0.01000000000000000021 ) ;
#8831 = CIRCLE ( 'NONE', #15388, 0.01500000000000003761 ) ;
#8832 =( GEOMETRIC_REPRESENTATION_CONTEXT ( 3 ) GLOBAL_UNCERTAINTY_ASSIGNED_CONTEXT ( ( #40439 ) ) GLOBAL_UNIT_ASSIGNED_CONTEXT ( ( #16884, #26549, #10491 ) ) REPRESENTATION_CONTEXT ( 'NONE', 'WORKASPACE' ) );
#8833 = CARTESIAN_POINT ( 'NONE',  ( 0.0001146438086225802652, -0.5834251000296799550, -0.08070232224184867298 ) ) ;
#8834 = CARTESIAN_POINT ( 'NONE',  ( 0.3298351036060790387, -1.757032636962086114, 0.4723056884894215046 ) ) ;
#8835 = CARTESIAN_POINT ( 'NONE',  ( -0.2136509456379323546, -0.4946207598421927254, 0.3599999999999999867 ) ) ;
#8836 = FACE_OUTER_BOUND ( 'NONE', #25672, .T. ) ;
#8837 = AXIS2_PLACEMENT_3D ( 'NONE', #4587, #29509, #35467 ) ;
#8838 = EDGE_LOOP ( 'NONE', ( #7911, #33436, #17846, #37577 ) ) ;
#8839 = VERTEX_POINT ( 'NONE', #23785 ) ;
#8840 = AXIS2_PLACEMENT_3D ( 'NONE', #13594, #37665, #19162 ) ;
#8841 = CARTESIAN_POINT ( 'NONE',  ( -0.1196081096344499550, -0.4993394475604064908, 0.1302951649420537872 ) ) ;
#8842 = ORIENTED_EDGE ( 'NONE', *, *, #36776, .T. ) ;
#8843 = DIRECTION ( 'NONE',  ( 1.000000000000000000, -0.000000000000000000, -0.000000000000000000 ) ) ;
#8844 = CARTESIAN_POINT ( 'NONE',  ( -0.1190772264498491800, -0.4967457283353927111, 0.1275078045371871027 ) ) ;
#8846 = ORIENTED_EDGE ( 'NONE', *, *, #14959, .F. ) ;
#8845 = CARTESIAN_POINT ( 'NONE',  ( 0.001993913723218970323, -0.5355225131288038343, 0.09668841071476408366 ) ) ;
#8847 = ORIENTED_EDGE ( 'NONE', *, *, #24325, .T. ) ;
#8848 = CARTESIAN_POINT ( 'NONE',  ( 0.04229956186878620211, 0.4483852441756290275, -0.1364680347311786890 ) ) ;
#8849 = VERTEX_POINT ( 'NONE', #35710 ) ;
#8850 = CARTESIAN_POINT ( 'NONE',  ( 0.02433822063067445085, -0.7066234909068694892, 0.5546226239478463382 ) ) ;
#8852 = CARTESIAN_POINT ( 'NONE',  ( 0.1260969926168152566, -1.253913687407651967, 0.6054891446326211568 ) ) ;
#8851 = CARTESIAN_POINT ( 'NONE',  ( 0.3168552283135301351, -1.073657105286919267, 0.7402218143473522360 ) ) ;
#8853 = CARTESIAN_POINT ( 'NONE',  ( 0.3727806007709784097, -1.152479425862310558, 0.4884953832116078476 ) ) ;
#8854 = CONTEXT_DEPENDENT_SHAPE_REPRESENTATION ( #20071, #36407 ) ;
#8855 = CONICAL_SURFACE ( 'NONE', #35787, 0.1400000000000009570, 1.047197551196600962 ) ;
#8856 = CARTESIAN_POINT ( 'NONE',  ( 0.7055834023472599137, -1.451092590515833392, 0.5677234696916273471 ) ) ;
#8858 = ORIENTED_EDGE ( 'NONE', *, *, #23412, .F. ) ;
#8857 = ORIENTED_EDGE ( 'NONE', *, *, #35356, .T. ) ;
#8859 = AXIS2_PLACEMENT_3D ( 'NONE', #14469, #21495, #2354 ) ;
#8860 = CARTESIAN_POINT ( 'NONE',  ( 0.000000000000000000, 0.000000000000000000, 0.000000000000000000 ) ) ;
#8861 = DIRECTION ( 'NONE',  ( -6.162975822039154046E-33, 0.000000000000000000, -1.000000000000000000 ) ) ;
#8862 = DIRECTION ( 'NONE',  ( 0.000000000000000000, 0.000000000000000000, -1.000000000000000000 ) ) ;
#8863 = AXIS2_PLACEMENT_3D ( 'NONE', #25858, #22964, #37981 ) ;
#8864 = CARTESIAN_POINT ( 'NONE',  ( 0.3717445303674562496, -1.104844584519105943, 0.7786008353294959772 ) ) ;
#8865 = DIRECTION ( 'NONE',  ( -1.000000000000000000, 0.000000000000000000, 0.000000000000000000 ) ) ;
#8866 = LOCAL_TIME ( 0, 53, 7.000000000000000000, #21180 ) ;
#8867 = DIRECTION ( 'NONE',  ( 0.000000000000000000, 0.000000000000000000, -1.000000000000000000 ) ) ;
#8868 = CARTESIAN_POINT ( 'NONE',  ( 0.3191045316042666613, -1.760553544078689026, 0.5737075626876623202 ) ) ;
#8869 = CARTESIAN_POINT ( 'NONE',  ( 0.3891894383937726243, -1.723671533896645958, 0.4268439981611141243 ) ) ;
#8870 = AXIS2_PLACEMENT_3D ( 'NONE', #27910, #12067, #8765 ) ;
#8871 = CARTESIAN_POINT ( 'NONE',  ( 0.3619193181407161508, -1.620069869474523472, -0.6100577121333333741 ) ) ;
#8872 = CARTESIAN_POINT ( 'NONE',  ( 0.07405242469529096927, -1.324323623009547202, 0.5682417262808779901 ) ) ;
#8873 = CARTESIAN_POINT ( 'NONE',  ( 0.3119220788584739501, -1.019769644837810185, 0.7484519766187490708 ) ) ;
#8874 = CARTESIAN_POINT ( 'NONE',  ( 0.4247042268939170140, -1.110871729138690256, 0.6103025838679678738 ) ) ;
#8875 = CARTESIAN_POINT ( 'NONE',  ( 0.3539331831703069198, -1.624680115194805152, -0.4258185731538512431 ) ) ;
#8876 = B_SPLINE_CURVE_WITH_KNOTS ( 'NONE', 3,
 ( #12342, #3090, #15632, #3483, #22228, #28788, #25505, #28590, #22845, #19337, #13347, #16640, #6550, #35552, #10061, #13561, #35365, #7155 ),
 .UNSPECIFIED., .F., .F.,
 ( 4, 2, 2, 2, 2, 2, 2, 2, 4 ),
 ( -0.002633528389679722082, -0.001975271857855721153, -0.001317015326031719790, -0.0006587587942077184275, -5.022623837174985950E-07, 0.0006577542694402834303, 0.001316010801264285227, 0.001974267333088286155, 0.002632523864912287084 ),
 .UNSPECIFIED. ) ;
#8877 = CARTESIAN_POINT ( 'NONE',  ( -0.2399999999999999079, -4.442986640879458271, -0.6151136631325511139 ) ) ;
#8878 = EDGE_CURVE ( 'NONE', #40516, #19999, #39399, .T. ) ;
#8879 = CARTESIAN_POINT ( 'NONE',  ( 0.003338613830247910610, -0.5117837562375455729, 0.3073580953312808339 ) ) ;
#8880 = CARTESIAN_POINT ( 'NONE',  ( 0.04797482002446179505, -1.049455964310542777, 0.7276413311358312930 ) ) ;
#8881 = CALENDAR_DATE ( 2026, 13, 10 ) ;
#8882 = CARTESIAN_POINT ( 'NONE',  ( 0.4378619693737221819, -1.010538247186560268, 0.8194577876302902020 ) ) ;
#8883 = AXIS2_PLACEMENT_3D ( 'NONE', #3666, #32441, #32045 ) ;
#8884 = CARTESIAN_POINT ( 'NONE',  ( 0.7038410752055113129, -1.517571454057699443, 0.5632464140165025501 ) ) ;
#8885 = CARTESIAN_POINT ( 'NONE',  ( -0.2746410161513779258, -1.874946189051298617, -0.07947534077849525980 ) ) ;
#8886 = EDGE_CURVE ( 'NONE', #29074, #10339, #15054, .T. ) ;
#8887 = CARTESIAN_POINT ( 'NONE',  ( 0.3394335999418694461, -1.659526807576534146, -0.3889335715588135289 ) ) ;
#8888 = ORIENTED_EDGE ( 'NONE', *, *, #4230, .F. ) ;
#8889 = CARTESIAN_POINT ( 'NONE',  ( -0.05464101615137761936, -1.984114763688379579, -0.7731012124309359912 ) ) ;
#8890 = APPLIED_APPROVAL_ASSIGNMENT ( #33271, ( #26657 ) ) ;
#8891 = APPROVAL ( #25347, 'UNSPECIFIED' ) ;
#8892 = CARTESIAN_POINT ( 'NONE',  ( 0.2628895756871428291, -1.634670359451999788, 0.7935051471341527662 ) ) ;
#8893 = CARTESIAN_POINT ( 'NONE',  ( 0.1296612367934588672, -0.5770376283328382261, 0.2571717286738921526 ) ) ;
#8895 = ORIENTED_EDGE ( 'NONE', *, *, #1929, .T. ) ;
#8894 = LINE ( 'NONE', #21657, #15179 ) ;
#8896 = CIRCLE ( 'NONE', #19427, 0.1346589359789737705 ) ;
#8897 = CARTESIAN_POINT ( 'NONE',  ( 0.5890075386511577360, -1.247786712317649815, 0.6995832148063678702 ) ) ;
#8899 = VERTEX_POINT ( 'NONE', #1582 ) ;
#8898 = ORIENTED_EDGE ( 'NONE', *, *, #38358, .F. ) ;
#8900 = CARTESIAN_POINT ( 'NONE',  ( 0.2381337884976891806, -0.6974119706843676658, 0.5054819936770663658 ) ) ;
#8901 = CARTESIAN_POINT ( 'NONE',  ( 0.3568951684747839748, -1.733180931717886120, -0.5240687084291923981 ) ) ;
#8902 = APPROVAL_DATE_TIME ( #17952, #19955 ) ;
#8903 = CARTESIAN_POINT ( 'NONE',  ( -0.2343922129835739054, -0.5166151207188712791, 0.1000000000000000749 ) ) ;
#8904 = ORIENTED_EDGE ( 'NONE', *, *, #35806, .T. ) ;
#8905 = CARTESIAN_POINT ( 'NONE',  ( 0.09981923470275097521, -0.7260083312159106850, 0.3343492273789105407 ) ) ;
#8906 = CARTESIAN_POINT ( 'NONE',  ( 0.1757500541653520265, -1.230771478115229245, -0.7462941026102624109 ) ) ;
#8907 = CARTESIAN_POINT ( 'NONE',  ( 0.4725026279546233332, -1.434192584178236807, 0.8017224222965745328 ) ) ;
#8909 = CARTESIAN_POINT ( 'NONE',  ( -0.001900788452498577497, -0.8469055337045260368, 0.09163843197140913999 ) ) ;
#8908 = FACE_OUTER_BOUND ( 'NONE', #23544, .T. ) ;
#8910 = CARTESIAN_POINT ( 'NONE',  ( 0.01623329718145851558, -0.9477957671793985073, 0.2415891105782959902 ) ) ;
#8911 = ORIENTED_EDGE ( 'NONE', *, *, #39899, .T. ) ;
#8912 = VERTEX_POINT ( 'NONE', #16803 ) ;
#8913 = CYLINDRICAL_SURFACE ( 'NONE', #34440, 0.06250000000000001388 ) ;
#8914 = CARTESIAN_POINT ( 'NONE',  ( 0.5545352172160372684, -1.200673110126019294, 0.8790629059729889727 ) ) ;
#8915 = AXIS2_PLACEMENT_3D ( 'NONE', #28860, #18809, #6430 ) ;
#8916 = CARTESIAN_POINT ( 'NONE',  ( -0.05464101615137796630, -1.622350287959229087, -0.08960079202753243321 ) ) ;
#8917 = EDGE_CURVE ( 'NONE', #14679, #33134, #18494, .T. ) ;
#8918 = LINE ( 'NONE', #27254, #15325 ) ;
#8919 = APPROVAL_PERSON_ORGANIZATION ( #18459, #28494, #31619 ) ;
#8920 = CARTESIAN_POINT ( 'NONE',  ( 0.000000000000000000, 0.000000000000000000, 0.000000000000000000 ) ) ;
#8921 = EDGE_CURVE ( 'NONE', #26169, #28258, #14531, .T. ) ;
#8922 = EDGE_CURVE ( 'NONE', #15637, #10835, #28332, .T. ) ;
#8923 = CARTESIAN_POINT ( 'NONE',  ( -0.2399999999999999079, -2.458279774191353351, -0.8760505995903041798 ) ) ;
#8924 = ADVANCED_FACE ( 'NONE', ( #8128 ), #14524, .T. ) ;
#8925 = AXIS2_PLACEMENT_3D ( 'NONE', #19702, #22404, #16232 ) ;
#8926 = CARTESIAN_POINT ( 'NONE',  ( 0.3511079287476749355, -1.164805985122749465, 0.4335040596137047508 ) ) ;
#8927 = CARTESIAN_POINT ( 'NONE',  ( 0.5083828713348212958, -1.120917766412646177, 0.6786323191735850191 ) ) ;
#8928 = APPROVAL_ROLE ( '' ) ;
#8929 = FACE_OUTER_BOUND ( 'NONE', #29732, .T. ) ;
#8930 = CARTESIAN_POINT ( 'NONE',  ( 0.3699999999999785127, -2.054734391222357459, -0.6850094247584045393 ) ) ;
#8931 = LINE ( 'NONE', #3355, #4386 ) ;
#8932 = CARTESIAN_POINT ( 'NONE',  ( 0.3923243630925510872, -1.966611948492501316, -0.4968729097670202544 ) ) ;
#8933 = ADVANCED_FACE ( 'NONE', ( #40419 ), #14291, .T. ) ;
#8934 = EDGE_LOOP ( 'NONE', ( #562, #26270, #4397, #6867 ) ) ;
#8935 = CARTESIAN_POINT ( 'NONE',  ( 0.3942702837509829417, -1.601394264692599156, -0.3531866499983610241 ) ) ;
#8936 = FACE_OUTER_BOUND ( 'NONE', #12440, .T. ) ;
#8937 = CARTESIAN_POINT ( 'NONE',  ( 0.6841302653033145553, -1.411212316466117223, 0.6057417262805112612 ) ) ;
#8938 = ORIENTED_EDGE ( 'NONE', *, *, #15151, .T. ) ;
#8939 = AXIS2_PLACEMENT_3D ( 'NONE', #13575, #10075, #259 ) ;
#8940 = CARTESIAN_POINT ( 'NONE',  ( -0.05544444631433741166, -0.02030017825816498797, -0.4608552147122320641 ) ) ;
#8941 = CARTESIAN_POINT ( 'NONE',  ( 0.1447739588591331894, -1.157841457446613598, 0.7566199150856840472 ) ) ;
#8943 = ORIENTED_EDGE ( 'NONE', *, *, #25631, .F. ) ;
#8942 = ORIENTED_EDGE ( 'NONE', *, *, #24100, .T. ) ;
#8944 = CARTESIAN_POINT ( 'NONE',  ( -0.1211791774340324757, -0.5069275750892242582, 0.1468366819525770417 ) ) ;
#8945 = CARTESIAN_POINT ( 'NONE',  ( 0.03875673594170349345, -0.03328920108826790430, 0.4752375706209726602 ) ) ;
#8946 = APPLIED_SECURITY_CLASSIFICATION_ASSIGNMENT ( #25389, ( #40653 ) ) ;
#8947 = CARTESIAN_POINT ( 'NONE',  ( 0.01548846960706570797, -0.4730347584886935852, -0.2341461249029953284 ) ) ;
#8948 = B_SPLINE_CURVE_WITH_KNOTS ( 'NONE', 3,
 ( #8640, #33967, #17703, #30250, #11556, #39930, #5562, #11746, #18325, #2080, #37039, #36828, #40113, #14618, #21213, #30680 ),
 .UNSPECIFIED., .F., .F.,
 ( 4, 2, 2, 2, 2, 2, 2, 4 ),
 ( 0.000000000000000000, 0.0004030402500546790201, 0.0008060805001093580401, 0.001209120750164036952, 0.001612161000218716080, 0.002418241500328066531, 0.002821281750382742624, 0.003224322000437419150 ),
 .UNSPECIFIED. ) ;
#8949 = CARTESIAN_POINT ( 'NONE',  ( 0.3777061319049067056, -1.720453251631598679, -0.5284398357475414976 ) ) ;
#8950 = DIRECTION ( 'NONE',  ( 1.000000000000000000, -0.000000000000000000, -0.000000000000000000 ) ) ;
#8952 = CARTESIAN_POINT ( 'NONE',  ( 0.2325871439873127555, -1.347985720369676121, 0.5231355526079688456 ) ) ;
#8951 = CARTESIAN_POINT ( 'NONE',  ( 0.04230258372739759826, 0.4443637212174459394, 0.1488268768076428383 ) ) ;
#8953 = CARTESIAN_POINT ( 'NONE',  ( 0.02881408050861044082, -0.3393437137871890275, -0.3647498010034141425 ) ) ;
#8954 = VERTEX_POINT ( 'NONE', #13515 ) ;
#8955 = CIRCLE ( 'NONE', #1129, 0.01500000000000004281 ) ;
#8956 = CARTESIAN_POINT ( 'NONE',  ( 0.1774005755516563920, -0.7643112578446873417, 0.6237371788150407603 ) ) ;
#8957 = ORIENTED_EDGE ( 'NONE', *, *, #18808, .F. ) ;
#8958 = CARTESIAN_POINT ( 'NONE',  ( 0.6777607415330073604, -1.552933800012288978, 0.6113354315870481726 ) ) ;
#8959 = CARTESIAN_POINT ( 'NONE',  ( 0.07091372799986922493, -0.6193112222544570056, 0.3868635014313515641 ) ) ;
#8961 = CARTESIAN_POINT ( 'NONE',  ( 0.5532300872722170082, -1.623494116491306594, 0.5181769067174267773 ) ) ;
#8960 = CARTESIAN_POINT ( 'NONE',  ( 0.000000000000000000, 0.8492681979939306069, -0.2138253033704803907 ) ) ;
#8962 = CARTESIAN_POINT ( 'NONE',  ( 4.780733988912460139E-16, 0.2949999999999991518, -7.512581982576723358E-16 ) ) ;
#8963 = FACE_OUTER_BOUND ( 'NONE', #21569, .T. ) ;
#8964 = ORIENTED_EDGE ( 'NONE', *, *, #23876, .F. ) ;
#8965 = CARTESIAN_POINT ( 'NONE',  ( 0.05999999999999990757, -0.03575622569115821658, -0.2978615321325044363 ) ) ;
#8966 = CARTESIAN_POINT ( 'NONE',  ( 0.1808977814881074231, -1.754363797449167262, -0.3261742699824988767 ) ) ;
#8967 = CARTESIAN_POINT ( 'NONE',  ( 0.1224514167073170595, -0.5493860373880040671, 0.1457185332388692411 ) ) ;
#8968 = CARTESIAN_POINT ( 'NONE',  ( 0.4547198050419078430, -1.678377057945577677, 0.4517409696548269071 ) ) ;
#8969 = DIRECTION ( 'NONE',  ( 1.060606950627616897E-16, 6.122684696619992497E-17, 1.000000000000000000 ) ) ;
#8970 = ADVANCED_FACE ( 'NONE', ( #36313 ), #2730, .T. ) ;
#8971 = CARTESIAN_POINT ( 'NONE',  ( -0.04229956186878639640, 0.4483852441756294160, 0.1364680347311792996 ) ) ;
#8972 = FACE_OUTER_BOUND ( 'NONE', #17415, .T. ) ;
#8973 = ADVANCED_FACE ( 'NONE', ( #22979 ), #29355, .F. ) ;
#8974 = FACE_OUTER_BOUND ( 'NONE', #28663, .T. ) ;
#8975 = FACE_OUTER_BOUND ( 'NONE', #23501, .T. ) ;
#8976 = VECTOR ( 'NONE', #21034, 39.37007874015748143 ) ;
#8977 = EDGE_CURVE ( 'NONE', #5149, #4721, #886, .T. ) ;
#8978 = CARTESIAN_POINT ( 'NONE',  ( 0.4897931935426230177, -1.095389100717072850, 0.8439147301884563079 ) ) ;
#8979 = CARTESIAN_POINT ( 'NONE',  ( -0.04047161733259624361, 0.3430572239576530902, 0.3654812350069518434 ) ) ;
#8980 = CARTESIAN_POINT ( 'NONE',  ( 0.02467386667972750608, -1.028554209509673578, 0.5662612265361036679 ) ) ;
#8981 = APPROVAL_PERSON_ORGANIZATION ( #19597, #40187, #7640 ) ;
#8982 = EDGE_CURVE ( 'NONE', #40212, #35830, #28305, .T. ) ;
#8983 = B_SPLINE_CURVE_WITH_KNOTS ( 'NONE', 3,
 ( #5216, #15301, #27647, #40177, #40394, #40592 ),
 .UNSPECIFIED., .F., .F.,
 ( 4, 2, 4 ),
 ( -5.502486261264484631E-06, 0.0003446809754944347277, 0.0006948644372501340018 ),
 .UNSPECIFIED. ) ;
#8984 = CARTESIAN_POINT ( 'NONE',  ( 0.6612567317249036236, -1.491170171073062045, -0.4119998595604874025 ) ) ;
#8985 = CARTESIAN_POINT ( 'NONE',  ( 0.02953079040094807803, 0.2329676531120586647, 0.4763574306556516702 ) ) ;
#8986 = CARTESIAN_POINT ( 'NONE',  ( 0.1401418647927308025, -0.8661219404098066121, 0.4927111136368755306 ) ) ;
#8987 = CARTESIAN_POINT ( 'NONE',  ( 0.2669858372074024322, -1.675026322382315191, 0.5720923781018742993 ) ) ;
#8988 = AXIS2_PLACEMENT_3D ( 'NONE', #38009, #16399, #31633 ) ;
#8989 = DIRECTION ( 'NONE',  ( 1.000000000000000000, 0.000000000000000000, 0.000000000000000000 ) ) ;
#8990 = ADVANCED_FACE ( 'NONE', ( #11438 ), #38194, .T. ) ;
#8991 = VERTEX_POINT ( 'NONE', #40424 ) ;
#8992 = PLANE ( 'NONE',  #9510 ) ;
#8993 = DIRECTION ( 'NONE',  ( -1.000000000000000000, -2.341930812374887555E-31, 1.664003471950578127E-31 ) ) ;
#8994 = ADVANCED_FACE ( 'NONE', ( #21526 ), #17609, .T. ) ;
#8995 = CARTESIAN_POINT ( 'NONE',  ( 0.6554648208145406052, -1.536877632280804873, 0.4182417262808777458 ) ) ;
#8996 = CARTESIAN_POINT ( 'NONE',  ( 0.4233792892081513215, -1.670469256985428474, -0.6343475356697100276 ) ) ;
#8997 = ADVANCED_FACE ( 'NONE', ( #2388, #30564 ), #36532, .F. ) ;
#8998 = EDGE_LOOP ( 'NONE', ( #34812, #13603, #34661, #3978 ) ) ;
#8999 = CARTESIAN_POINT ( 'NONE',  ( 0.4939251185753719686, -1.677760966407569665, -0.6096475700680613619 ) ) ;
#9000 = EDGE_CURVE ( 'NONE', #33695, #20593, #15856, .T. ) ;
#9001 = VERTEX_POINT ( 'NONE', #14504 ) ;
#9002 = CARTESIAN_POINT ( 'NONE',  ( 0.3917146490717380303, -1.113158088163010095, 0.6227922109902478409 ) ) ;
#9003 = CARTESIAN_POINT ( 'NONE',  ( 0.1892549258828873926, -0.8411929458066104148, 0.2428197129412378030 ) ) ;
#9004 = CARTESIAN_POINT ( 'NONE',  ( 0.03170953572518810798, 0.3312786565686240969, -0.3635309226454341291 ) ) ;
#9005 = CARTESIAN_POINT ( 'NONE',  ( 0.4381095118996915505, -1.199720832187643582, 0.7206127906299513164 ) ) ;
#9007 = ORIENTED_EDGE ( 'NONE', *, *, #40637, .F. ) ;
#9006 = PLANE ( 'NONE',  #33765 ) ;
#9008 = CARTESIAN_POINT ( 'NONE',  ( 0.3877041582795131003, -1.010062466692070560, 0.6423187497268529889 ) ) ;
#9009 = CIRCLE ( 'NONE', #19533, 0.06250000000000000000 ) ;
#9010 = ORIENTED_EDGE ( 'NONE', *, *, #12935, .T. ) ;
#9011 = PERSON_AND_ORGANIZATION ( #28500, #32463 ) ;
#9012 =( REPRESENTATION_RELATIONSHIP ('NONE','NONE', #33020, #24383 ) REPRESENTATION_RELATIONSHIP_WITH_TRANSFORMATION ( #5764 )SHAPE_REPRESENTATION_RELATIONSHIP( ) );
#9013 = CARTESIAN_POINT ( 'NONE',  ( 0.5612334960093817715, -1.620627794947044897, -0.4868944820179721966 ) ) ;
#9014 = ORIENTED_EDGE ( 'NONE', *, *, #13270, .F. ) ;
#9015 = ORIENTED_EDGE ( 'NONE', *, *, #14710, .T. ) ;
#9016 =( BOUNDED_SURFACE ( )  B_SPLINE_SURFACE ( 3, 2, ( 
 ( #14722, #39602, #24811 ),
 ( #8534, #21318, #5658 ),
 ( #18214, #30760, #15116 ),
 ( #8953, #2783, #15332 ),
 ( #27888, #9144, #21708 ),
 ( #12856, #12437, #19443 ),
 ( #28884, #19231, #3590 ),
 ( #25199, #15543, #40621 ),
 ( #6458, #10173, #31773 ),
 ( #12633, #3376, #28094 ),
 ( #25417, #9759, #6052 ),
 ( #15932, #22529, #24990 ),
 ( #37741, #141, #19029 ),
 ( #21924, #18839, #28694 ),
 ( #745, #22742, #25819 ),
 ( #38340, #3793, #18620 ),
 ( #22329, #37521, #28479 ),
 ( #31178, #31381, #34848 ) ),
 .UNSPECIFIED., .F., .F., .T. ) 
 B_SPLINE_SURFACE_WITH_KNOTS ( ( 4, 2, 2, 2, 2, 2, 2, 2, 4 ),
 ( 3, 3 ),
 ( -0.001532620576208848376, -0.0007637936630077624307, 5.033250193323623133E-06, 0.0007738601633944096770, 0.001542687076595495622, 0.002311513989796581785, 0.003080340902997667513, 0.003849167816198753242, 0.004617994729399839404 ),
 ( 0.000000000000000000, 1.000000000000000000 ),
 .UNSPECIFIED. ) 
 GEOMETRIC_REPRESENTATION_ITEM ( )  RATIONAL_B_SPLINE_SURFACE ( (
 ( 1.000000000000000000, 0.7283825911960419841, 1.000000000000000000),
 ( 1.000000000000000000, 0.7404385082114082195, 1.000000000000000000),
 ( 1.000000000000000000, 0.7521504257738304000, 1.000000000000000000),
 ( 1.000000000000000000, 0.7744497410761531642, 1.000000000000000000),
 ( 1.000000000000000000, 0.7845654757373292654, 1.000000000000000000),
 ( 1.000000000000000000, 0.8022083990892909799, 1.000000000000000000),
 ( 1.000000000000000000, 0.8094167424697321644, 1.000000000000000000),
 ( 1.000000000000000000, 0.8194491993618630010, 1.000000000000000000),
 ( 1.000000000000000000, 0.8220634900780660059, 1.000000000000000000),
 ( 1.000000000000000000, 0.8220705070823303151, 1.000000000000000000),
 ( 1.000000000000000000, 0.8194468812480828479, 1.000000000000000000),
 ( 1.000000000000000000, 0.8094220769839568508, 1.000000000000000000),
 ( 1.000000000000000000, 0.8022659121986730479, 1.000000000000000000),
 ( 1.000000000000000000, 0.7845681159034245677, 1.000000000000000000),
 ( 1.000000000000000000, 0.7744426415185311496, 1.000000000000000000),
 ( 1.000000000000000000, 0.7522890290928635482, 1.000000000000000000),
 ( 1.000000000000000000, 0.7403540167215398871, 1.000000000000000000),
 ( 1.000000000000000000, 0.7283825911960186694, 1.000000000000000000) ) ) 
 REPRESENTATION_ITEM ( '' )  SURFACE ( )  );
#9017 = CARTESIAN_POINT ( 'NONE',  ( 0.3594954150521289526, -1.619161029595283186, 0.6519928337199429880 ) ) ;
#9019 = CARTESIAN_POINT ( 'NONE',  ( 0.1753879760477817240, -0.8109860937599424613, -0.04834239174515909954 ) ) ;
#9018 = CARTESIAN_POINT ( 'NONE',  ( 0.06505414422235179794, -0.8155846679102959351, 0.07151615054459180276 ) ) ;
#9020 = CARTESIAN_POINT ( 'NONE',  ( 0.2112514853725389330, -1.519796704070200732, -0.3223733989273451228 ) ) ;
#9021 = ORIENTED_EDGE ( 'NONE', *, *, #24785, .F. ) ;
#9022 = EDGE_LOOP ( 'NONE', ( #37130, #20720, #3235 ) ) ;
#9023 = CARTESIAN_POINT ( 'NONE',  ( 0.3090203544014926140, -0.9165002773570758432, 0.5981876956776405185 ) ) ;
#9024 = CARTESIAN_POINT ( 'NONE',  ( 0.4408853310126066849, -1.325034971439371212, 0.8326428173140825173 ) ) ;
#9025 = ORIENTED_EDGE ( 'NONE', *, *, #7894, .F. ) ;
#9026 = CARTESIAN_POINT ( 'NONE',  ( 0.1926120471057841121, -1.518195021730778471, -0.3560059264261548062 ) ) ;
#9027 = DIRECTION ( 'NONE',  ( -0.4999551463232372317, 0.8660512985181134660, -0.000000000000000000 ) ) ;
#9028 = CARTESIAN_POINT ( 'NONE',  ( 0.07950324646436757181, -1.397811199834917417, -0.3670508432710352653 ) ) ;
#9029 = EDGE_CURVE ( 'NONE', #22735, #20761, #16527, .T. ) ;
#9030 = CARTESIAN_POINT ( 'NONE',  ( 0.5901238867768096030, -1.488331658671158797, -0.4293751906308629906 ) ) ;
#9031 = B_SPLINE_CURVE_WITH_KNOTS ( 'NONE', 3,
 ( #21486, #5399, #2951, #18577, #8909, #24168, #17962, #30522, #27447, #2347, #24351, #15502, #33589, #34007, #18170, #8497, #27637, #5811, #6012, #15286, #18370, #36692, #28056, #21062, #34201, #39972, #11793, #30724, #30917, #21672, #36885, #8693, #24769, #21272 ),
 .UNSPECIFIED., .F., .F.,
 ( 4, 2, 2, 2, 2, 2, 2, 2, 2, 2, 2, 2, 2, 2, 2, 2, 4 ),
 ( 0.000000000000000000, 0.0008327512041488100087, 0.001665502408297620017, 0.002498253612446430568, 0.003331004816595241336, 0.004163756020744051670, 0.004996507224892862871, 0.005829258429041673205, 0.006662009633190484406, 0.007494760837339294740, 0.008327512041488103339, 0.009160263245636913673, 0.009993014449785724007, 0.01082576565393453434, 0.01165851685808334294, 0.01249126806223215327, 0.01332401926638096534 ),
 .UNSPECIFIED. ) ;
#9032 = EDGE_CURVE ( 'NONE', #19986, #37556, #32285, .T. ) ;
#9033 = DIRECTION ( 'NONE',  ( 1.000000000000000000, -0.000000000000000000, -0.000000000000000000 ) ) ;
#9034 = CARTESIAN_POINT ( 'NONE',  ( 0.5696125550597064269, -1.613556559779221189, 0.4687417262808790674 ) ) ;
#9035 = CARTESIAN_POINT ( 'NONE',  ( 0.03309057659885121516, 0.3730661755626903942, -0.3633900220890659005 ) ) ;
#9036 = DIRECTION ( 'NONE',  ( -1.000000000000000000, -0.000000000000000000, -0.000000000000000000 ) ) ;
#9037 = CARTESIAN_POINT ( 'NONE',  ( 0.2073812095156316870, -1.204313567361931847, 0.5182417262812423209 ) ) ;
#9038 = APPLICATION_PROTOCOL_DEFINITION ( 'international standard', 'automotive_design', 2000, #24276 ) ;
#9039 = CARTESIAN_POINT ( 'NONE',  ( 0.4635148750433638609, -1.130672306621219647, 0.4607556654368962779 ) ) ;
#9040 = CARTESIAN_POINT ( 'NONE',  ( 0.4374219344798826459, -1.230185402379724069, 0.5856983068965044836 ) ) ;
#9041 = DIRECTION ( 'NONE',  ( 1.000000000000000000, 1.138269997360101095E-15, -8.537024980200757723E-16 ) ) ;
#9042 = CARTESIAN_POINT ( 'NONE',  ( 0.01266180416972241714, -0.9102398499036795654, 0.5581420674395337622 ) ) ;
#9043 = CARTESIAN_POINT ( 'NONE',  ( 0.2616322387702281205, -1.678013124025769187, 0.5382687897764735219 ) ) ;
#9044 = DIRECTION ( 'NONE',  ( -0.3961231183188297922, 0.000000000000000000, 0.9181974053183586948 ) ) ;
#9045 = CARTESIAN_POINT ( 'NONE',  ( 0.5971614065082352374, -1.461417804984935342, 0.6057417262805111502 ) ) ;
#9046 = CIRCLE ( 'NONE', #7060, 0.1620173459747806799 ) ;
#9047 = ORIENTED_EDGE ( 'NONE', *, *, #11263, .F. ) ;
#9048 = ORIENTED_EDGE ( 'NONE', *, *, #6142, .F. ) ;
#9049 = CARTESIAN_POINT ( 'NONE',  ( -0.1148699535791894571, -0.5253002637279450271, 0.1262353127152268661 ) ) ;
#9050 = ORIENTED_EDGE ( 'NONE', *, *, #933, .T. ) ;
#9051 = CARTESIAN_POINT ( 'NONE',  ( -2.696301922142129510E-33, 0.7171888913565960255, -0.2325238883388469069 ) ) ;
#9052 = CARTESIAN_POINT ( 'NONE',  ( -0.2399999999999999079, -2.375187403135927688, -0.6336237179921873075 ) ) ;
#9053 = CARTESIAN_POINT ( 'NONE',  ( -0.2399999999999999079, -2.810395079000055585, -0.3781292493067240912 ) ) ;
#9055 = ORIENTED_EDGE ( 'NONE', *, *, #2205, .F. ) ;
#9054 = DIRECTION ( 'NONE',  ( 1.188678714063518227E-15, -1.000000000000000000, -3.263080277421930985E-16 ) ) ;
#9056 = ORIENTED_EDGE ( 'NONE', *, *, #36776, .F. ) ;
#9057 = CARTESIAN_POINT ( 'NONE',  ( 0.01895494625228211910, 0.5124113341948440814, -0.08888305413160359214 ) ) ;
#9058 = VERTEX_POINT ( 'NONE', #27069 ) ;
#9059 = CARTESIAN_POINT ( 'NONE',  ( 0.01298442562731116044, -0.6517174416560403971, 0.4734301074441944479 ) ) ;
#9061 = CARTESIAN_POINT ( 'NONE',  ( 0.6047538891612445067, -1.605163873594933843, 0.4396382108053981108 ) ) ;
#9060 = CARTESIAN_POINT ( 'NONE',  ( 0.2984382882072237897, -1.047452999410511065, 0.7351907297634064919 ) ) ;
#9062 = CARTESIAN_POINT ( 'NONE',  ( 0.6065946466975035145, -1.478929314905678361, 0.5636733106534758120 ) ) ;
#9063 = DATE_AND_TIME ( #56, #29371 ) ;
#9064 = CARTESIAN_POINT ( 'NONE',  ( -0.002218965743620939825, -1.368565310413371705, -0.3828039145932563558 ) ) ;
#9066 = VERTEX_POINT ( 'NONE', #8740 ) ;
#9065 = VERTEX_POINT ( 'NONE', #30155 ) ;
#9067 = CARTESIAN_POINT ( 'NONE',  ( 0.3842289435304718226, -1.843891179545533943, -0.4840290186776841086 ) ) ;
#9068 = DIRECTION ( 'NONE',  ( 0.4999999999999968359, -0.4440468346413921075, -0.7435202812600091304 ) ) ;
#9069 = CARTESIAN_POINT ( 'NONE',  ( -0.2399999999999999079, -2.342996121808762044, -0.6842569225768811991 ) ) ;
#9070 = CARTESIAN_POINT ( 'NONE',  ( 0.4914180550386734736, -1.285646375261855878, 0.7919587470386610928 ) ) ;
#9071 = CARTESIAN_POINT ( 'NONE',  ( 0.01548846960707528191, -0.4638115001430989648, 0.2459753896937853235 ) ) ;
#9072 = CARTESIAN_POINT ( 'NONE',  ( 0.5308991137012172290, -1.672779244431372492, -0.4688114127372004503 ) ) ;
#9073 = CARTESIAN_POINT ( 'NONE',  ( 0.03757742148941851240, -0.6212996915455626379, 0.6062798531290721771 ) ) ;
#9074 = B_SPLINE_CURVE_WITH_KNOTS ( 'NONE', 5,
 ( #8246, #8034, #14615, #27185, #18121, #40110 ),
 .UNSPECIFIED., .F., .F.,
 ( 6, 6 ),
 ( 5.240850777407929151, 7.803531517424560526 ),
 .UNSPECIFIED. ) ;
#9075 = FACE_BOUND ( 'NONE', #22530, .T. ) ;
#9076 = CARTESIAN_POINT ( 'NONE',  ( 0.6586645934826005355, -1.563799363216411331, 0.4177417262808784670 ) ) ;
#9077 = CARTESIAN_POINT ( 'NONE',  ( -0.2746410161513776482, -4.121841830394775030, -0.5449218438908057793 ) ) ;
#9078 = CARTESIAN_POINT ( 'NONE',  ( -0.2399999999999999079, -3.941790907013290823, -0.4709369376873030477 ) ) ;
#9079 = DIRECTION ( 'NONE',  ( -0.4999551463232372317, 0.8660512985181134660, -0.000000000000000000 ) ) ;
#9080 = CARTESIAN_POINT ( 'NONE',  ( 0.2039603895705197623, -1.429414345016513765, 0.9236325154956378514 ) ) ;
#9081 = CARTESIAN_POINT ( 'NONE',  ( 0.05019192336334400012, -1.073493884431249601, 0.7323994023816953192 ) ) ;
#9082 = PERSON_AND_ORGANIZATION_ROLE ( 'creator' ) ;
#9083 = CARTESIAN_POINT ( 'NONE',  ( 0.2173028089842584942, -0.6047810126270140030, 0.4525757583899530645 ) ) ;
#9084 = CARTESIAN_POINT ( 'NONE',  ( 0.6699292074404745723, -1.569526485364062474, 0.6071573546319919412 ) ) ;
#9085 = CARTESIAN_POINT ( 'NONE',  ( 0.03309057659885152047, -0.3730661755626882292, 0.3633900220890675103 ) ) ;
#9086 = CARTESIAN_POINT ( 'NONE',  ( 0.3646274796662056228, -1.706748141935739094, -0.4511273082355062303 ) ) ;
#9087 = ORIENTED_EDGE ( 'NONE', *, *, #32560, .T. ) ;
#9088 = CARTESIAN_POINT ( 'NONE',  ( 0.3591498995103406533, -1.737620376665804933, -0.5147966178037263196 ) ) ;
#9089 = CARTESIAN_POINT ( 'NONE',  ( 0.2675992341663611107, -1.614841384873237917, 0.8159387862359652743 ) ) ;
#9090 = CARTESIAN_POINT ( 'NONE',  ( 0.4552858789809595685, -1.287359980045181151, 0.8227995234754879039 ) ) ;
#9092 = ORIENTED_EDGE ( 'NONE', *, *, #17973, .T. ) ;
#9091 = DIRECTION ( 'NONE',  ( 0.8660512985181133550, 0.4999551463232371207, 0.000000000000000000 ) ) ;
#9093 = CARTESIAN_POINT ( 'NONE',  ( 0.5367554652047751285, -1.159747519872984300, 0.6504567231333411303 ) ) ;
#9095 = VERTEX_POINT ( 'NONE', #33434 ) ;
#9094 = ORIENTED_EDGE ( 'NONE', *, *, #38831, .F. ) ;
#9096 = CARTESIAN_POINT ( 'NONE',  ( 0.1959265899308190728, -1.288818386415671036, -0.7414046965098798347 ) ) ;
#9097 = DIRECTION ( 'NONE',  ( -1.000000000000000000, -0.000000000000000000, -0.000000000000000000 ) ) ;
#9098 = DIRECTION ( 'NONE',  ( 0.4999551463232372317, -0.8660512985181133550, 0.000000000000000000 ) ) ;
#9099 = DATE_AND_TIME ( #37087, #23435 ) ;
#9100 = CARTESIAN_POINT ( 'NONE',  ( 0.4159916692016358830, -1.069406866067976081, -0.5155029497116575543 ) ) ;
#9101 = ORIENTED_EDGE ( 'NONE', *, *, #17925, .F. ) ;
#9102 = CARTESIAN_POINT ( 'NONE',  ( 0.08673251224761270584, -0.7254629984980496271, 0.1796334135243346508 ) ) ;
#9103 = CARTESIAN_POINT ( 'NONE',  ( 0.3048570497350419073, -1.756853555320991189, 0.5694442476137213660 ) ) ;
#9104 = CARTESIAN_POINT ( 'NONE',  ( 0.4529273117239071000, -1.400119990640080081, 0.8223471911486823771 ) ) ;
#9106 = DIRECTION ( 'NONE',  ( 0.000000000000000000, 0.000000000000000000, -1.000000000000000000 ) ) ;
#9105 = CARTESIAN_POINT ( 'NONE',  ( 0.3520636416031024951, -1.608800853759478677, -0.6368828113034350480 ) ) ;
#9107 = CARTESIAN_POINT ( 'NONE',  ( 0.01573875648097932539, -0.9458718438695528086, 0.1964948750599073701 ) ) ;
#9108 = VERTEX_POINT ( 'NONE', #40209 ) ;
#9109 = CARTESIAN_POINT ( 'NONE',  ( 0.4624513059194432230, -1.677210534090505245, 0.5769224047549080803 ) ) ;
#9110 = CARTESIAN_POINT ( 'NONE',  ( 0.5352968706694352097, -1.169515972850764696, 0.8775555985942493642 ) ) ;
#9111 = CARTESIAN_POINT ( 'NONE',  ( 0.5079445638232780169, -1.582110533707940192, -0.5155029497116575543 ) ) ;
#9112 = DIRECTION ( 'NONE',  ( 0.000000000000000000, 1.000000000000000000, -3.330669073875470607E-16 ) ) ;
#9113 = APPLIED_DATE_AND_TIME_ASSIGNMENT ( #11178, #4030, ( #29284 ) ) ;
#9114 = CARTESIAN_POINT ( 'NONE',  ( -0.1743922129835733248, -0.5166151207188712791, 0.09999999999999961697 ) ) ;
#9115 = CARTESIAN_POINT ( 'NONE',  ( 0.3948505749649401375, -1.157343825677206617, 0.4182417262808778013 ) ) ;
#9116 = CARTESIAN_POINT ( 'NONE',  ( 0.003465668518863261691, -1.839186521745578284, -0.6434132171392461519 ) ) ;
#9117 = FACE_OUTER_BOUND ( 'NONE', #16352, .T. ) ;
#9118 = CARTESIAN_POINT ( 'NONE',  ( 0.4452807512755668218, -1.047893410216382382, 0.6910429845488149647 ) ) ;
#9119 = APPLICATION_PROTOCOL_DEFINITION ( 'international standard', 'automotive_design', 2000, #16635 ) ;
#9120 = CARTESIAN_POINT ( 'NONE',  ( 0.3624061103390691096, -1.968824918581854932, -0.4968426515055719972 ) ) ;
#9121 = CARTESIAN_POINT ( 'NONE',  ( 0.3898146559560766722, -1.698689370364980133, -0.4973142990484694104 ) ) ;
#9122 = CARTESIAN_POINT ( 'NONE',  ( 0.5611322101011324559, -1.505499452099228641, 0.5480364229397299836 ) ) ;
#9123 = CARTESIAN_POINT ( 'NONE',  ( -0.03474824846560347485, -0.07233741238826779663, 0.5114535313566185293 ) ) ;
#9124 = ADVANCED_FACE ( 'NONE', ( #39818 ), #18406, .T. ) ;
#9125 = ORIENTED_EDGE ( 'NONE', *, *, #10763, .T. ) ;
#9126 = CARTESIAN_POINT ( 'NONE',  ( -0.1212185687160894504, -0.5071153897904228103, 0.3078438592385183692 ) ) ;
#9127 = CARTESIAN_POINT ( 'NONE',  ( 0.2142458193968007074, -0.9048875576697104073, 0.6439300487045382937 ) ) ;
#9128 = ORIENTED_EDGE ( 'NONE', *, *, #3207, .T. ) ;
#9129 = CARTESIAN_POINT ( 'NONE',  ( -0.03171102739523230796, -0.05432883045314854803, -0.4888204606144185282 ) ) ;
#9130 = CARTESIAN_POINT ( 'NONE',  ( 0.1722800781603322229, -1.380285231960554526, 0.5936621141595983531 ) ) ;
#9132 = ORIENTED_EDGE ( 'NONE', *, *, #32275, .F. ) ;
#9131 = ORIENTED_EDGE ( 'NONE', *, *, #2894, .F. ) ;
#9133 = ADVANCED_FACE ( 'NONE', ( #2184 ), #9016, .T. ) ;
#9134 = DIRECTION ( 'NONE',  ( 2.465190328815661892E-32, 1.000000000000000000, 6.656013887802287108E-31 ) ) ;
#9135 = VERTEX_POINT ( 'NONE', #34453 ) ;
#9136 = CARTESIAN_POINT ( 'NONE',  ( 0.4840267074530639757, -1.682517813888804392, -0.4333519947141560857 ) ) ;
#9137 = CARTESIAN_POINT ( 'NONE',  ( 0.7308477326836637644, -1.487300591783543124, 0.7156276807793737760 ) ) ;
#9138 = CARTESIAN_POINT ( 'NONE',  ( 0.1836296472909090260, -1.744742035088381327, -0.3568621931777658518 ) ) ;
#9139 = EDGE_CURVE ( 'NONE', #17741, #38533, #36870, .T. ) ;
#9140 = FACE_OUTER_BOUND ( 'NONE', #22892, .T. ) ;
#9142 = CARTESIAN_POINT ( 'NONE',  ( 0.1826134026666640375, -1.261648033191452578, 0.4282186462236585722 ) ) ;
#9141 = DIRECTION ( 'NONE',  ( 0.4999999999999970024, 0.2529028965469328760, 0.8282753919549792343 ) ) ;
#9143 = ADVANCED_FACE ( 'NONE', ( #16157 ), #5312, .T. ) ;
#9144 = CARTESIAN_POINT ( 'NONE',  ( 0.04308558661661592015, -0.3346374335304956316, -0.3638133228716434187 ) ) ;
#9145 = ORIENTED_EDGE ( 'NONE', *, *, #34325, .T. ) ;
#9146 = ADVANCED_FACE ( 'NONE', ( #9962 ), #35291, .T. ) ;
#9147 = CARTESIAN_POINT ( 'NONE',  ( 0.1136507236048572705, -0.6373588427272240953, 0.4267424632662121242 ) ) ;
#9148 = ORIENTED_EDGE ( 'NONE', *, *, #143, .F. ) ;
#9149 = CARTESIAN_POINT ( 'NONE',  ( -0.2399999999999999079, -2.457388234162025675, -0.5792354969483111127 ) ) ;
#9150 = CARTESIAN_POINT ( 'NONE',  ( 0.4048501170226769807, -1.424128732296970234, 0.8405605425542692632 ) ) ;
#9152 = CARTESIAN_POINT ( 'NONE',  ( 0.5596723329040782513, -1.621442011146171369, 0.5567257723923959567 ) ) ;
#9151 = DIRECTION ( 'NONE',  ( 0.4996194577002578407, -0.8662449985352299597, 0.000000000000000000 ) ) ;
#9153 = CARTESIAN_POINT ( 'NONE',  ( 0.06875593408321428734, -1.327476523378791962, 0.5532905004612894695 ) ) ;
#9154 = DIRECTION ( 'NONE',  ( -0.2204180896037088722, -0.8274293670542908208, 0.5165041222600136317 ) ) ;
#9155 = CARTESIAN_POINT ( 'NONE',  ( -0.2746410161513770931, -2.861028283584748699, -0.4103205306338891245 ) ) ;
#9156 = CARTESIAN_POINT ( 'NONE',  ( 0.3916117103943055899, -1.785355738137090809, -0.5264918531311321148 ) ) ;
#9157 = CARTESIAN_POINT ( 'NONE',  ( 0.5809008504126312866, -1.495258029342362072, 0.5730765960790278335 ) ) ;
#9158 = CARTESIAN_POINT ( 'NONE',  ( 0.4838384605851756559, -1.673620472881901300, 0.5087549739108570002 ) ) ;
#9159 = CARTESIAN_POINT ( 'NONE',  ( -0.1684323895664525950, 0.5231977504174881721, 0.3032895567580808360 ) ) ;
#9160 = ADVANCED_FACE ( 'NONE', ( #13056 ), #9943, .F. ) ;
#9161 = VERTEX_POINT ( 'NONE', #6866 ) ;
#9162 = CARTESIAN_POINT ( 'NONE',  ( -0.04230188431063472421, 0.4429734639576320965, 0.1531098457317267014 ) ) ;
#9163 = APPLIED_DATE_AND_TIME_ASSIGNMENT ( #5632, #18187, ( #25768 ) ) ;
#9164 = CARTESIAN_POINT ( 'NONE',  ( -0.08000000000000000167, -2.183180860297908144, -0.4937760292030871079 ) ) ;
#9165 = CARTESIAN_POINT ( 'NONE',  ( 0.2181682312481163233, -1.239626545742103181, 0.5655726110498544568 ) ) ;
#9166 = CARTESIAN_POINT ( 'NONE',  ( 0.2259476328985426941, -1.236619376729935382, 0.4746024408792181570 ) ) ;
#9167 = B_SPLINE_CURVE_WITH_KNOTS ( 'NONE', 3,
 ( #35092, #6689, #16185, #19469, #28726, #32002, #3209, #15754, #587, #22561, #16369, #28304, #28908, #13279, #21737, #174, #34271, #31208 ),
 .UNSPECIFIED., .F., .F.,
 ( 4, 2, 2, 2, 2, 2, 2, 2, 4 ),
 ( 0.000000000000000000, 0.0007544293770661929764, 0.001508858754132385953, 0.002263288131198578929, 0.003017717508264771906, 0.003772146885330964882, 0.004526576262397157858, 0.005281005639463353003, 0.006035435016529549015 ),
 .UNSPECIFIED. ) ;
#9168 = CARTESIAN_POINT ( 'NONE',  ( 0.4805300281521128203, -1.080349003257709439, 0.8405881438443104647 ) ) ;
#9169 = CARTESIAN_POINT ( 'NONE',  ( -0.03874953289575077536, 0.2523958943867715687, 0.4040664878102117052 ) ) ;
#9170 = CARTESIAN_POINT ( 'NONE',  ( 0.4887921365776448090, -1.679766821171225999, -0.4193976862638449377 ) ) ;
#9171 = CARTESIAN_POINT ( 'NONE',  ( 0.6058310743872277193, -1.588085125911432804, -0.4741143205363104740 ) ) ;
#9172 = CARTESIAN_POINT ( 'NONE',  ( 0.3957193873654859528, -2.010249311248437198, -0.4875152547671333658 ) ) ;
#9173 = CARTESIAN_POINT ( 'NONE',  ( 0.1268788240767347308, -0.8367918140873071842, 0.4559310628402723498 ) ) ;
#9174 = CARTESIAN_POINT ( 'NONE',  ( 0.2623454991891604471, -1.677609158577047621, 0.5446184138564792443 ) ) ;
#9175 = CARTESIAN_POINT ( 'NONE',  ( 0.02953079040095700838, 0.2329676531120518090, 0.4763574306556300764 ) ) ;
#9176 = ORIENTED_EDGE ( 'NONE', *, *, #382, .F. ) ;
#9177 = FACE_OUTER_BOUND ( 'NONE', #18198, .T. ) ;
#9178 = CARTESIAN_POINT ( 'NONE',  ( 0.4045767908288230297, -1.721983033185328527, -0.6022994628584866783 ) ) ;
#9179 = CARTESIAN_POINT ( 'NONE',  ( 0.6583193209383879640, -1.530332598402602828, 0.4182417262808776903 ) ) ;
#9180 = DIRECTION ( 'NONE',  ( -1.000000000000000000, 0.000000000000000000, 0.000000000000000000 ) ) ;
#9181 = DIRECTION ( 'NONE',  ( 0.000000000000000000, 0.000000000000000000, -1.000000000000000000 ) ) ;
#9182 = ORIENTED_EDGE ( 'NONE', *, *, #20222, .F. ) ;
#9183 = ADVANCED_FACE ( 'NONE', ( #16348 ), #13251, .F. ) ;
#9184 = CARTESIAN_POINT ( 'NONE',  ( 0.5005869906397938385, -1.690277863677645875, -0.6089672282429000605 ) ) ;
#9185 = CARTESIAN_POINT ( 'NONE',  ( 0.3780793312557618191, -1.119558780295859535, 0.6237031023607847446 ) ) ;
#9186 = CARTESIAN_POINT ( 'NONE',  ( -0.2746410161513776482, -4.289222312108804225, -0.6708809693675255037 ) ) ;
#9187 = CARTESIAN_POINT ( 'NONE',  ( 0.04229974373173431973, 0.2684538943183510384, -0.3841910309321978079 ) ) ;
#9188 = ADVANCED_FACE ( 'NONE', ( #35270 ), #8610, .F. ) ;
#9189 = CARTESIAN_POINT ( 'NONE',  ( 0.4177594668114605336, -1.172467419432972724, 0.7388445284618762043 ) ) ;
#9191 = CARTESIAN_POINT ( 'NONE',  ( 0.5395555926592416895, -1.597940071789080374, -0.5747445381412426002 ) ) ;
#9190 = DIRECTION ( 'NONE',  ( 0.000000000000000000, 0.000000000000000000, -1.000000000000000000 ) ) ;
#9192 = CARTESIAN_POINT ( 'NONE',  ( 0.1960870051948097048, -0.8771803234346856604, 0.3014997781122282783 ) ) ;
#9193 = EDGE_LOOP ( 'NONE', ( #19286, #18984, #3595, #15158 ) ) ;
#9194 = PERSON_AND_ORGANIZATION_ROLE ( 'classification_officer' ) ;
#9195 = EDGE_CURVE ( 'NONE', #1840, #641, #2083, .T. ) ;
#9196 = DIRECTION ( 'NONE',  ( -8.788982220891970033E-16, 0.7692307692307691624, -0.6389710663783134681 ) ) ;
#9197 = EDGE_LOOP ( 'NONE', ( #21428, #18053, #23644, #6762 ) ) ;
#9198 = ORIENTED_EDGE ( 'NONE', *, *, #31080, .T. ) ;
#9199 = CARTESIAN_POINT ( 'NONE',  ( 0.04802694997680392180, -0.5385102852490685210, 0.1733495709028375353 ) ) ;
#9201 = CARTESIAN_POINT ( 'NONE',  ( 0.1864532405559393979, -0.6659192699994888054, -0.02049162290020863433 ) ) ;
#9200 = CYLINDRICAL_SURFACE ( 'NONE', #4608, 0.03000000000000029379 ) ;
#9202 = DIRECTION ( 'NONE',  ( -0.4999551463232373427, 0.8660512985181134660, -0.000000000000000000 ) ) ;
#9203 = ORIENTED_EDGE ( 'NONE', *, *, #19251, .T. ) ;
#9204 = VECTOR ( 'NONE', #18929, 39.37007874015748854 ) ;
#9205 = ORIENTED_EDGE ( 'NONE', *, *, #25007, .F. ) ;
#9206 = CARTESIAN_POINT ( 'NONE',  ( 0.3804416727307123880, -1.009541828604827218, 0.6200734748803748975 ) ) ;
#9207 = CARTESIAN_POINT ( 'NONE',  ( 0.1648809095896444921, -0.7520497700267493313, 0.5690099980341608576 ) ) ;
#9208 = ORIENTED_EDGE ( 'NONE', *, *, #8249, .T. ) ;
#9209 = CARTESIAN_POINT ( 'NONE',  ( 0.2060189241777137525, -2.057789047793026516, -0.3052958066308563145 ) ) ;
#9210 = CARTESIAN_POINT ( 'NONE',  ( 0.05999999999999990757, 0.000000000000000000, 0.000000000000000000 ) ) ;
#9211 = AXIS2_PLACEMENT_3D ( 'NONE', #40409, #16143, #12235 ) ;
#9212 = EDGE_CURVE ( 'NONE', #18566, #1887, #19785, .T. ) ;
#9213 = CARTESIAN_POINT ( 'NONE',  ( 0.001230546430223489760, -1.915437084753079722, -0.3396229129526682211 ) ) ;
#9214 = CARTESIAN_POINT ( 'NONE',  ( 0.02953079040095728247, 0.000000000000000000, 0.000000000000000000 ) ) ;
#9215 = DIRECTION ( 'NONE',  ( 1.188678714063518227E-15, -1.000000000000000000, -3.263080277421930985E-16 ) ) ;
#9216 = CARTESIAN_POINT ( 'NONE',  ( 0.3999999999999783729, -2.086934379033410725, -0.5179790689110178592 ) ) ;
#9217 = CARTESIAN_POINT ( 'NONE',  ( -0.08000000000000000167, -2.179113517810423062, -0.3318097452986852880 ) ) ;
#9218 = CARTESIAN_POINT ( 'NONE',  ( 0.4136294883733862005, -1.694877849074643672, 0.4182417262808776903 ) ) ;
#9219 = CARTESIAN_POINT ( 'NONE',  ( 0.06824055730039223222, -1.289945330482348496, 0.6789996349980699231 ) ) ;
#9220 = PERSON_AND_ORGANIZATION_ROLE ( 'classification_officer' ) ;
#9221 = CARTESIAN_POINT ( 'NONE',  ( 0.4613690144166702201, -1.065390048215762997, 0.6270275320092995042 ) ) ;
#9222 = CARTESIAN_POINT ( 'NONE',  ( 0.4611807422268464074, -1.110735627432217765, 0.5647948193072632739 ) ) ;
#9223 = DIRECTION ( 'NONE',  ( -8.881784197001246407E-16, 2.361472542561082612E-16, -1.000000000000000000 ) ) ;
#9224 = CARTESIAN_POINT ( 'NONE',  ( 0.5873347430034532302, -1.537871679492680110, -0.6182658308370784228 ) ) ;
#9225 = CARTESIAN_POINT ( 'NONE',  ( 0.01933088760290150449, -0.9443470376599968352, 0.6102586483404766060 ) ) ;
#9226 = FACE_OUTER_BOUND ( 'NONE', #7863, .T. ) ;
#9227 = DIRECTION ( 'NONE',  ( -0.4999999999999985567, -0.6123724356957951365, 0.6123724356957951365 ) ) ;
#9228 = AXIS2_PLACEMENT_3D ( 'NONE', #26638, #7686, #39167 ) ;
#9229 = CARTESIAN_POINT ( 'NONE',  ( 0.5960504044690355663, -1.458754575269462395, 0.6057417262805163682 ) ) ;
#9230 = ORIENTED_EDGE ( 'NONE', *, *, #11197, .F. ) ;
#9231 = ORIENTED_EDGE ( 'NONE', *, *, #9029, .F. ) ;
#9232 =( BOUNDED_SURFACE ( )  B_SPLINE_SURFACE ( 3, 2, ( 
 ( #18134, #14628, #8653 ),
 ( #5353, #27414, #30690 ),
 ( #31446, #23705, #14419 ),
 ( #17714, #8456, #20624 ),
 ( #30479, #21448, #37048 ),
 ( #28351, #4964, #17531 ),
 ( #30079, #23917, #8871 ),
 ( #2309, #40126, #14849 ) ),
 .UNSPECIFIED., .F., .F., .F. ) 
 B_SPLINE_SURFACE_WITH_KNOTS ( ( 4, 2, 2, 4 ),
 ( 3, 3 ),
 ( 0.001132904267245888079, 0.001446982864295271072, 0.001761061461344653849, 0.002389218655443419402 ),
 ( 0.000000000000000000, 1.000000000000000000 ),
 .UNSPECIFIED. ) 
 GEOMETRIC_REPRESENTATION_ITEM ( )  RATIONAL_B_SPLINE_SURFACE ( (
 ( 1.000000000000000000, 0.4483291926235775660, 1.000000000000000000),
 ( 1.000000000000000000, 0.4613307591293988597, 1.000000000000000000),
 ( 1.000000000000000000, 0.4741491466902303942, 1.000000000000000000),
 ( 1.000000000000000000, 0.4983216539137984014, 1.000000000000000000),
 ( 1.000000000000000000, 0.5096972859111215115, 1.000000000000000000),
 ( 1.000000000000000000, 0.5380540011986519877, 1.000000000000000000),
 ( 1.000000000000000000, 0.5496804717520560324, 1.000000000000000000),
 ( 1.000000000000000000, 0.5504785946861833201, 1.000000000000000000) ) ) 
 REPRESENTATION_ITEM ( '' )  SURFACE ( )  );
#9233 = CARTESIAN_POINT ( 'NONE',  ( -0.02000000000000000042, -2.274798198814180772, -0.3601501197397404264 ) ) ;
#9234 = ORIENTED_EDGE ( 'NONE', *, *, #30894, .F. ) ;
#9235 = DIRECTION ( 'NONE',  ( -8.881784197001246407E-16, 2.361472542561082612E-16, -1.000000000000000000 ) ) ;
#9236 = TOROIDAL_SURFACE ( 'NONE', #30266, 0.5250000000000000222, 0.01499999999999999944 ) ;
#9237 = ADVANCED_FACE ( 'NONE', ( #38551 ), #3236, .T. ) ;
#9238 = CARTESIAN_POINT ( 'NONE',  ( 0.5185735850971436856, -1.328908583238292973, 0.7912473624542825101 ) ) ;
#9240 = ORIENTED_EDGE ( 'NONE', *, *, #1446, .T. ) ;
#9239 = CARTESIAN_POINT ( 'NONE',  ( 0.01548846960706677829, 0.3772621329472856666, -0.3651003739303602669 ) ) ;
#9241 = EDGE_LOOP ( 'NONE', ( #28041, #24827, #417, #6119, #16340, #24458 ) ) ;
#9242 = CARTESIAN_POINT ( 'NONE',  ( 0.05999999999999990757, 0.000000000000000000, 0.000000000000000000 ) ) ;
#9243 = VERTEX_POINT ( 'NONE', #36484 ) ;
#9244 = CARTESIAN_POINT ( 'NONE',  ( 0.2678708459125263008, -1.675617809333246777, 0.5935539999434353842 ) ) ;
#9246 = CARTESIAN_POINT ( 'NONE',  ( 0.1039318284443993545, -1.302570566043166123, 0.5899279477117637116 ) ) ;
#9245 = CARTESIAN_POINT ( 'NONE',  ( 0.4959102259190470430, -1.676612535457929098, -0.4224503755058100496 ) ) ;
#9247 = ADVANCED_FACE ( 'NONE', ( #27836 ), #11787, .T. ) ;
#9248 = DIRECTION ( 'NONE',  ( -1.000000000000000000, -0.000000000000000000, -0.000000000000000000 ) ) ;
#9249 = COORDINATED_UNIVERSAL_TIME_OFFSET ( 0, 0, .AHEAD. ) ;
#9250 = CARTESIAN_POINT ( 'NONE',  ( -0.2746410161513770931, -2.909786385774835171, -0.3705357231075772084 ) ) ;
#9252 = ORIENTED_EDGE ( 'NONE', *, *, #7142, .F. ) ;
#9251 = ORIENTED_EDGE ( 'NONE', *, *, #18862, .T. ) ;
#9253 = CARTESIAN_POINT ( 'NONE',  ( 0.4705465871830276092, -1.070011441572239930, -0.4234330131081484594 ) ) ;
#9254 = DIRECTION ( 'NONE',  ( 0.01455087615875040596, 0.9998941303973200023, 0.000000000000000000 ) ) ;
#9255 = CARTESIAN_POINT ( 'NONE',  ( -0.05138886601527748593, -0.4416142869301858398, 0.1669109982969966266 ) ) ;
#9256 = CARTESIAN_POINT ( 'NONE',  ( 0.4745478738625271697, -1.259349835786171878, 0.7951441819683597867 ) ) ;
#9257 = CARTESIAN_POINT ( 'NONE',  ( 0.1309676594288840534, -0.8283632510577545460, 0.2782064429851813236 ) ) ;
#9258 = DIRECTION ( 'NONE',  ( -0.4999551463232372317, 0.8660512985181135770, -0.000000000000000000 ) ) ;
#9259 = ADVANCED_FACE ( 'NONE', ( #24161 ), #21264, .T. ) ;
#9260 = AXIS2_PLACEMENT_3D ( 'NONE', #7782, #39059, #4894 ) ;
#9261 = APPLIED_PERSON_AND_ORGANIZATION_ASSIGNMENT ( #17101, #20398, ( #24771 ) ) ;
#9262 = CARTESIAN_POINT ( 'NONE',  ( 0.02831927448914906692, -0.5730460782701279898, 0.5331832225423767113 ) ) ;
#9263 = ADVANCED_FACE ( 'NONE', ( #30513 ), #33802, .F. ) ;
#9264 = CARTESIAN_POINT ( 'NONE',  ( 0.3891097478030026147, -1.721120859245148571, 0.4231916600392490180 ) ) ;
#9265 = VECTOR ( 'NONE', #2826, 39.37007874015748143 ) ;
#9266 = CARTESIAN_POINT ( 'NONE',  ( 0.3931005117246323399, -1.715828765679402679, 0.3667417262808779777 ) ) ;
#9267 = EDGE_CURVE ( 'NONE', #4624, #3966, #7965, .T. ) ;
#9268 = CARTESIAN_POINT ( 'NONE',  ( 0.3900778056733008592, -1.134510399567245864, 0.7523592440643727119 ) ) ;
#9269 = CARTESIAN_POINT ( 'NONE',  ( 0.3701597793959978122, -1.743707579621869286, -0.4236181223213599245 ) ) ;
#9270 = AXIS2_PLACEMENT_3D ( 'NONE', #24541, #5793, #40357 ) ;
#9271 = AXIS2_PLACEMENT_3D ( 'NONE', #23425, #32648, #33448 ) ;
#9272 = CARTESIAN_POINT ( 'NONE',  ( 0.04308558661660950168, -0.2425983775171404733, 0.4306836113028234547 ) ) ;
#9273 = CARTESIAN_POINT ( 'NONE',  ( -0.08000000000000000167, -1.518907846805490403, -0.1889969338327479598 ) ) ;
#9274 = CARTESIAN_POINT ( 'NONE',  ( 0.1053607631531530836, -1.334516741563384068, 0.7095644064326338540 ) ) ;
#9275 = CALENDAR_DATE ( 2026, 13, 10 ) ;
#9276 = CARTESIAN_POINT ( 'NONE',  ( 0.3446155261768803491, -0.8529094429884808148, 0.7348996499020890028 ) ) ;
#9277 = CARTESIAN_POINT ( 'NONE',  ( -0.3000000000000000999, -2.375007723916885194, -0.5268601001523036675 ) ) ;
#9278 = CIRCLE ( 'NONE', #21132, 0.01750000000000001554 ) ;
#9279 = CARTESIAN_POINT ( 'NONE',  ( 0.6750313905811581305, -1.555737387944355454, 0.6033254075622310753 ) ) ;
#9280 = CARTESIAN_POINT ( 'NONE',  ( 0.05083665881508999534, -0.3162195626321993580, 0.3525671453250093235 ) ) ;
#9281 = DIRECTION ( 'NONE',  ( 1.000000000000000000, -0.000000000000000000, -0.000000000000000000 ) ) ;
#9282 = VERTEX_POINT ( 'NONE', #15077 ) ;
#9283 = CARTESIAN_POINT ( 'NONE',  ( 0.4705313329396505484, -1.155124162917906538, -0.6196578200117470736 ) ) ;
#9284 = CARTESIAN_POINT ( 'NONE',  ( 0.2351328385853270198, -1.513397575123461403, 0.9164249233862159505 ) ) ;
#9285 = AXIS2_PLACEMENT_3D ( 'NONE', #39221, #7921, #20497 ) ;
#9286 = ADVANCED_FACE ( 'NONE', ( #2342 ), #14881, .F. ) ;
#9287 = CARTESIAN_POINT ( 'NONE',  ( 0.1330058442311542188, -0.5794291578589204628, 0.2619875031982849545 ) ) ;
#9289 = ORIENTED_EDGE ( 'NONE', *, *, #38942, .F. ) ;
#9288 = CARTESIAN_POINT ( 'NONE',  ( 0.3699999999999786793, -2.183180860297921466, -0.4937760292030871079 ) ) ;
#9290 = CARTESIAN_POINT ( 'NONE',  ( 0.5544140612800516621, -1.190962001057203956, 0.5445415982692776158 ) ) ;
#9292 = ORIENTED_EDGE ( 'NONE', *, *, #19196, .F. ) ;
#9291 = VERTEX_POINT ( 'NONE', #8903 ) ;
#9293 = CARTESIAN_POINT ( 'NONE',  ( 0.2006703192425639271, -0.5962780551271036344, 0.3430129484740815360 ) ) ;
#9294 = VECTOR ( 'NONE', #9516, 39.37007874015748143 ) ;
#9295 = CIRCLE ( 'NONE', #3399, 0.4615209409081865166 ) ;
#9296 = CARTESIAN_POINT ( 'NONE',  ( 0.02953079040095700838, 0.4684706630666080063, -0.2484463060367437248 ) ) ;
#9297 = DIRECTION ( 'NONE',  ( 1.060606950627616897E-16, 6.122684696619992497E-17, 1.000000000000000000 ) ) ;
#9298 = COORDINATED_UNIVERSAL_TIME_OFFSET ( 0, 0, .AHEAD. ) ;
#9299 = CIRCLE ( 'NONE', #38202, 0.1033070866141734268 ) ;
#9300 = DIRECTION ( 'NONE',  ( 0.000000000000000000, 0.000000000000000000, 1.000000000000000000 ) ) ;
#9301 = ORIENTED_EDGE ( 'NONE', *, *, #8751, .F. ) ;
#9302 = CARTESIAN_POINT ( 'NONE',  ( 0.1086040402818805040, -0.7941143328802063861, 0.3875077444786869107 ) ) ;
#9303 = FACE_OUTER_BOUND ( 'NONE', #37025, .T. ) ;
#9304 = CARTESIAN_POINT ( 'NONE',  ( 0.4971617628130152178, -1.474698883450294540, 0.7633393513624641136 ) ) ;
#9305 = DIRECTION ( 'NONE',  ( 1.000000000000000000, 1.707404996040164166E-15, 0.000000000000000000 ) ) ;
#9306 = CARTESIAN_POINT ( 'NONE',  ( -0.1524980003305985987, 0.4722686132664217773, 0.1089215716292313701 ) ) ;
#9307 = ORIENTED_EDGE ( 'NONE', *, *, #7735, .T. ) ;
#9308 = ORIENTED_EDGE ( 'NONE', *, *, #23626, .T. ) ;
#9309 = CARTESIAN_POINT ( 'NONE',  ( 0.4341036163735219611, -1.690926254025340691, 0.4262558845157656262 ) ) ;
#9310 = CARTESIAN_POINT ( 'NONE',  ( 0.7139080051254665937, -1.458177603278905332, 0.7675176523170569309 ) ) ;
#9311 = CARTESIAN_POINT ( 'NONE',  ( 0.1084341599040759135, -1.414529908605170361, 0.5685197021117063265 ) ) ;
#9312 = CARTESIAN_POINT ( 'NONE',  ( -0.1653405084325597907, 0.5136906775330227770, 0.3358539725464960157 ) ) ;
#9313 = VECTOR ( 'NONE', #18689, 39.37007874015748143 ) ;
#9314 = EDGE_CURVE ( 'NONE', #33860, #28462, #33698, .T. ) ;
#9315 = CARTESIAN_POINT ( 'NONE',  ( -0.01548846960707524721, 0.000000000000000000, 0.000000000000000000 ) ) ;
#9316 = DIRECTION ( 'NONE',  ( -1.000000000000000000, -0.000000000000000000, -0.000000000000000000 ) ) ;
#9317 = CARTESIAN_POINT ( 'NONE',  ( 0.006005486288604863949, -0.9514584861060970677, 0.4879672165010910390 ) ) ;
#9318 = CARTESIAN_POINT ( 'NONE',  ( 0.4820398931871337500, -1.088803207145679242, 0.6894399345265510570 ) ) ;
#9319 = DATE_AND_TIME ( #24788, #6218 ) ;
#9320 = CONICAL_SURFACE ( 'NONE', #21835, 0.1620173459747806799, 1.047197551196600518 ) ;
#9321 = CIRCLE ( 'NONE', #28403, 0.009999999999999944697 ) ;
#9322 = DIRECTION ( 'NONE',  ( 0.8660512985181135770, 0.4999551463232370652, 0.000000000000000000 ) ) ;
#9323 = AXIS2_PLACEMENT_3D ( 'NONE', #37473, #28226, #93 ) ;
#9324 = ORIENTED_EDGE ( 'NONE', *, *, #17176, .F. ) ;
#9325 = CARTESIAN_POINT ( 'NONE',  ( 0.3893819225029191422, -1.720935294021423978, 0.4231407362055625843 ) ) ;
#9326 = CARTESIAN_POINT ( 'NONE',  ( -0.05616044724337281718, 0.01023656896654763504, 0.4592816919116773922 ) ) ;
#9327 = ORIENTED_EDGE ( 'NONE', *, *, #12922, .F. ) ;
#9328 = CARTESIAN_POINT ( 'NONE',  ( 0.4062230848227149638, -1.145582794160931117, 0.4248905050063955802 ) ) ;
#9329 = DIRECTION ( 'NONE',  ( 2.465190328815661892E-32, 1.000000000000000000, 6.656013887802287108E-31 ) ) ;
#9330 = CARTESIAN_POINT ( 'NONE',  ( 0.08670662847365112613, -0.7414284123014263095, 0.03488965029717239208 ) ) ;
#9331 = VERTEX_POINT ( 'NONE', #39769 ) ;
#9332 = CARTESIAN_POINT ( 'NONE',  ( -0.02238765564325250618, 0.06997643758149711679, -0.5076344429488346410 ) ) ;
#9333 = CARTESIAN_POINT ( 'NONE',  ( 0.1141547338916006765, -1.221815644227830511, 0.7539337555814515923 ) ) ;
#9335 = ORIENTED_EDGE ( 'NONE', *, *, #29419, .F. ) ;
#9334 = ORIENTED_EDGE ( 'NONE', *, *, #19321, .F. ) ;
#9336 = CARTESIAN_POINT ( 'NONE',  ( 0.5462348416196848300, -1.594646255991501560, -0.4868944820179722521 ) ) ;
#9337 = ORIENTED_EDGE ( 'NONE', *, *, #6784, .F. ) ;
#9338 = CARTESIAN_POINT ( 'NONE',  ( 0.4039331521932674751, -1.711434328629108714, 0.5182417262808777236 ) ) ;
#9339 = CARTESIAN_POINT ( 'NONE',  ( 0.3666495184304034427, -1.755770389311256396, -0.5282448765462863793 ) ) ;
#9340 = DIRECTION ( 'NONE',  ( -1.000000000000000000, -2.280301054154495132E-31, 1.664003471950577689E-31 ) ) ;
#9341 = VECTOR ( 'NONE', #24628, 39.37007874015748143 ) ;
#9343 = CARTESIAN_POINT ( 'NONE',  ( 0.1757500541653520265, -1.230771478115229245, -0.5931747813493342125 ) ) ;
#9342 = CARTESIAN_POINT ( 'NONE',  ( 0.03171893264485862313, 0.4702476704888156056, 0.2325692314474981925 ) ) ;
#9344 = CARTESIAN_POINT ( 'NONE',  ( 0.1266021694322588542, -1.239399129679921829, 0.5182417262812423209 ) ) ;
#9345 = ORIENTED_EDGE ( 'NONE', *, *, #22368, .T. ) ;
#9346 = CARTESIAN_POINT ( 'NONE',  ( 0.1044857023475970897, -0.6151305603489410911, 0.3740774240993971489 ) ) ;
#9347 = ORIENTED_EDGE ( 'NONE', *, *, #24878, .F. ) ;
#9348 = CIRCLE ( 'NONE', #10039, 0.1000000000000000194 ) ;
#9349 = SHAPE_REPRESENTATION ( 'Outer shift plate', ( #27819 ), #3510 ) ;
#9350 = DIRECTION ( 'NONE',  ( -0.8660512985181131329, -0.4999551463232376758, 0.000000000000000000 ) ) ;
#9351 = CONICAL_SURFACE ( 'NONE', #225, 0.1499999999999989675, 1.047197551196599408 ) ;
#9352 = CARTESIAN_POINT ( 'NONE',  ( 0.07283724563382382167, -0.5406377204022615457, 0.1457185332388694354 ) ) ;
#9354 = CARTESIAN_POINT ( 'NONE',  ( 0.5680507681239298501, -1.626009195392588591, 0.5004993007562670293 ) ) ;
#9353 = CARTESIAN_POINT ( 'NONE',  ( 0.3327035037690653230, -1.656108012777571359, -0.6420915705233924964 ) ) ;
#9355 = CARTESIAN_POINT ( 'NONE',  ( 0.3465130674089420548, -1.628963608593047230, -0.3702441142993493362 ) ) ;
#9356 = CARTESIAN_POINT ( 'NONE',  ( 0.1853092822385233873, -0.9263384658431096375, 0.3280667635356543377 ) ) ;
#9357 = VECTOR ( 'NONE', #10512, 39.37007874015748854 ) ;
#9358 = DIRECTION ( 'NONE',  ( -1.000000000000000000, -7.857794173099924470E-32, -8.628166150854818811E-32 ) ) ;
#9359 = CARTESIAN_POINT ( 'NONE',  ( 0.3982344888468541955, -1.728315610757950260, -0.3049413784164444197 ) ) ;
#9360 = CARTESIAN_POINT ( 'NONE',  ( 0.1341053683801476104, -0.6137581712303235015, 0.3478286551500012203 ) ) ;
#9361 = CARTESIAN_POINT ( 'NONE',  ( 0.4284705980304526207, -1.706026416638912746, 0.4298431576648689689 ) ) ;
#9362 = CARTESIAN_POINT ( 'NONE',  ( -0.05252049209742703367, 0.2830365943384567373, -0.3740706778132397714 ) ) ;
#9363 = AXIS2_PLACEMENT_3D ( 'NONE', #16406, #16016, #34721 ) ;
#9364 = DIRECTION ( 'NONE',  ( 1.000000000000000000, 1.681422630952712846E-11, -5.294072836416825871E-12 ) ) ;
#9365 = DIRECTION ( 'NONE',  ( 0.000000000000000000, 0.000000000000000000, -1.000000000000000000 ) ) ;
#9366 = CARTESIAN_POINT ( 'NONE',  ( 0.07499999999999960865, -0.01500000000000024925, 0.000000000000000000 ) ) ;
#9367 = CARTESIAN_POINT ( 'NONE',  ( 0.2257333548162994141, -1.236570967228644680, 0.5622049477089006153 ) ) ;
#9368 = EDGE_CURVE ( 'NONE', #553, #31435, #27631, .T. ) ;
#9369 = CARTESIAN_POINT ( 'NONE',  ( 0.6804297327399058126, -1.407484794882680745, 0.5682417262808783232 ) ) ;
#9370 = CARTESIAN_POINT ( 'NONE',  ( -0.03171893264487805203, 0.3665010048041807411, 0.3753642664049919864 ) ) ;
#9371 = CARTESIAN_POINT ( 'NONE',  ( 0.05844749783569043455, -1.323029004274733689, 0.5991599809669244658 ) ) ;
#9372 = ADVANCED_FACE ( 'NONE', ( #20660 ), #21476, .T. ) ;
#9373 = AXIS2_PLACEMENT_3D ( 'NONE', #9638, #31644, #33936 ) ;
#9374 = CARTESIAN_POINT ( 'NONE',  ( -1.019575837292305609, -0.04310840302198155199, 0.3599999999999999867 ) ) ;
#9375 = CARTESIAN_POINT ( 'NONE',  ( 0.4685571881589434273, -1.131435060437132156, -0.3725158680014900026 ) ) ;
#9376 = CARTESIAN_POINT ( 'NONE',  ( 0.1559984031573804775, -0.8964835598961180541, 0.5757252305435468509 ) ) ;
#9377 = EDGE_CURVE ( 'NONE', #19775, #30304, #39510, .T. ) ;
#9378 = FACE_OUTER_BOUND ( 'NONE', #18771, .T. ) ;
#9379 = CARTESIAN_POINT ( 'NONE',  ( -0.1710642718812834251, 0.4986889572247755198, 0.1528658435937002014 ) ) ;
#9380 = CIRCLE ( 'NONE', #10686, 0.02999999999999999542 ) ;
#9381 = VECTOR ( 'NONE', #27269, 39.37007874015748854 ) ;
#9382 = ORIENTED_EDGE ( 'NONE', *, *, #2145, .T. ) ;
#9383 = FACE_OUTER_BOUND ( 'NONE', #28032, .T. ) ;
#9384 = CARTESIAN_POINT ( 'NONE',  ( -0.2136509456379319383, -0.4946207598421927254, 0.08499999999999936773 ) ) ;
#9385 = CIRCLE ( 'NONE', #32377, 0.2200000000000000566 ) ;
#9386 = DIRECTION ( 'NONE',  ( -1.387778780781449423E-15, 6.691181741238501047E-16, -1.000000000000000000 ) ) ;
#9387 = CARTESIAN_POINT ( 'NONE',  ( 0.1834964085430285941, -1.226715333008844055, -0.5155029497116575543 ) ) ;
#9388 = CARTESIAN_POINT ( 'NONE',  ( 0.3679573697808270483, -2.043903617469527312, -0.4804103685335425200 ) ) ;
#9389 = ORIENTED_EDGE ( 'NONE', *, *, #38323, .T. ) ;
#9390 = CARTESIAN_POINT ( 'NONE',  ( 0.3969700875656382300, -1.750093955434189663, -0.5306525527942058673 ) ) ;
#9391 = EDGE_CURVE ( 'NONE', #8526, #30280, #14454, .T. ) ;
#9392 = LINE ( 'NONE', #31610, #17113 ) ;
#9393 = CARTESIAN_POINT ( 'NONE',  ( 0.3460543618422604051, -1.756493685445453146, 0.4557286970618524280 ) ) ;
#9394 = PRODUCT_RELATED_PRODUCT_CATEGORY ( 'detail', '', ( #35054 ) ) ;
#9395 = DIRECTION ( 'NONE',  ( 1.000000000000000000, 1.450080480853946466E-15, -8.881784197001242463E-16 ) ) ;
#9396 = CARTESIAN_POINT ( 'NONE',  ( 0.3852795338934388858, -1.129116621630487760, 0.7334296061308062109 ) ) ;
#9398 = DIRECTION ( 'NONE',  ( 0.000000000000000000, 0.000000000000000000, 1.000000000000000000 ) ) ;
#9397 = DIRECTION ( 'NONE',  ( -1.000000000000000000, 0.000000000000000000, 0.000000000000000000 ) ) ;
#9399 = CARTESIAN_POINT ( 'NONE',  ( 0.4927016384402401195, -1.082581181811578697, 0.5750743434332348247 ) ) ;
#9400 = ORIENTED_EDGE ( 'NONE', *, *, #34137, .F. ) ;
#9401 = COORDINATED_UNIVERSAL_TIME_OFFSET ( 0, 0, .AHEAD. ) ;
#9402 = CARTESIAN_POINT ( 'NONE',  ( -0.2136509456379324934, -0.4946207598421927254, 0.3749999999999996669 ) ) ;
#9403 = VERTEX_POINT ( 'NONE', #9911 ) ;
#9404 = VERTEX_POINT ( 'NONE', #16112 ) ;
#9405 = CARTESIAN_POINT ( 'NONE',  ( 0.2720344517543004104, -1.310141966359744004, 0.9014112804584356597 ) ) ;
#9407 = CARTESIAN_POINT ( 'NONE',  ( 0.1846989274142681881, -0.8380492819789600034, 0.07482513216622958818 ) ) ;
#9406 = CARTESIAN_POINT ( 'NONE',  ( -2.775557561562891351E-16, 1.318030225331671786E-16, -0.1999999999999994837 ) ) ;
#9408 = CARTESIAN_POINT ( 'NONE',  ( 0.3397077535880359545, -1.654685348432989089, -0.3858274525146626055 ) ) ;
#9409 = VERTEX_POINT ( 'NONE', #28049 ) ;
#9410 = VECTOR ( 'NONE', #39383, 39.37007874015748143 ) ;
#9411 = VERTEX_POINT ( 'NONE', #37478 ) ;
#9412 = ORIENTED_EDGE ( 'NONE', *, *, #4363, .T. ) ;
#9413 = CARTESIAN_POINT ( 'NONE',  ( 0.4231691825188668710, -1.033889518165662436, 0.6356716544661608070 ) ) ;
#9414 = CARTESIAN_POINT ( 'NONE',  ( 0.2607777723285606419, -0.9519272446484895456, 0.7368745005339746301 ) ) ;
#9415 = VERTEX_POINT ( 'NONE', #12812 ) ;
#9416 = CARTESIAN_POINT ( 'NONE',  ( 0.1872737887141963653, -0.7022237677290258384, 0.03102906701263268355 ) ) ;
#9417 = DIRECTION ( 'NONE',  ( 8.881784197001246407E-16, -2.361472542561082612E-16, 1.000000000000000000 ) ) ;
#9418 = CARTESIAN_POINT ( 'NONE',  ( 0.6123118846157344919, -1.441347382273072908, -0.6250000000000000000 ) ) ;
#9419 = AXIS2_PLACEMENT_3D ( 'NONE', #40036, #18041, #8989 ) ;
#9420 = CARTESIAN_POINT ( 'NONE',  ( -0.2746410161513782033, -2.294529520598973082, -0.6534431116140350104 ) ) ;
#9421 = CARTESIAN_POINT ( 'NONE',  ( 0.3784118722789395206, -1.581834032482531738, -0.2869361388274794256 ) ) ;
#9422 = AXIS2_PLACEMENT_3D ( 'NONE', #34482, #25849, #3410 ) ;
#9423 = CARTESIAN_POINT ( 'NONE',  ( -0.05464101615137761936, -1.845925619402022155, -0.3444148183989317880 ) ) ;
#9424 = ADVANCED_FACE ( 'NONE', ( #37692 ), #9320, .T. ) ;
#9425 = CYLINDRICAL_SURFACE ( 'NONE', #29201, 0.1249999999999999584 ) ;
#9426 = CARTESIAN_POINT ( 'NONE',  ( 0.04582889109739302080, 0.3361233334070958811, -0.3523147457849521991 ) ) ;
#9427 = AXIS2_PLACEMENT_3D ( 'NONE', #27416, #5577, #40129 ) ;
#9428 = CARTESIAN_POINT ( 'NONE',  ( 0.1161415672770640256, -1.518500864528294914, -0.6476785841699168600 ) ) ;
#9429 = CARTESIAN_POINT ( 'NONE',  ( 0.3459163166870670159, -1.704669448431704648, -0.4228134667771305533 ) ) ;
#9430 = DATE_AND_TIME ( #15618, #5570 ) ;
#9431 = EDGE_CURVE ( 'NONE', #6766, #9411, #32313, .T. ) ;
#9432 = CARTESIAN_POINT ( 'NONE',  ( 0.4835150722484384267, -1.077540828773440484, 0.6059843185820091849 ) ) ;
#9433 = CARTESIAN_POINT ( 'NONE',  ( -0.2399999999999999079, -2.183180860297908144, -0.4937760292030871079 ) ) ;
#9434 = ADVANCED_FACE ( 'NONE', ( #15891 ), #28435, .F. ) ;
#9435 = CARTESIAN_POINT ( 'NONE',  ( 0.5465059510172681767, -1.167163004870445331, 0.6057417262810063097 ) ) ;
#9436 = CARTESIAN_POINT ( 'NONE',  ( 0.5925625413354431714, -1.513297660314260940, -0.6339996871210799023 ) ) ;
#9437 = CARTESIAN_POINT ( 'NONE',  ( 0.002166586416275674380, -0.8510908774931603693, 0.4206164911499951642 ) ) ;
#9438 = DIRECTION ( 'NONE',  ( 1.000000000000000000, -0.000000000000000000, -0.000000000000000000 ) ) ;
#9439 = AXIS2_PLACEMENT_3D ( 'NONE', #773, #4419, #12886 ) ;
#9440 = CARTESIAN_POINT ( 'NONE',  ( -0.2746410161513770931, -2.768941938641841904, -0.5551618215276492574 ) ) ;
#9441 = ORIENTED_EDGE ( 'NONE', *, *, #25225, .F. ) ;
#9442 = TOROIDAL_SURFACE ( 'NONE', #2873, 1.986674066779348768, 0.01499999999999999944 ) ;
#9443 = ORIENTED_EDGE ( 'NONE', *, *, #26822, .F. ) ;
#9444 = AXIS2_PLACEMENT_3D ( 'NONE', #25310, #7158, #10283 ) ;
#9445 = ADVANCED_FACE ( 'NONE', ( #18788 ), #24522, .T. ) ;
#9446 = LINE ( 'NONE', #7153, #38760 ) ;
#9447 = ORIENTED_EDGE ( 'NONE', *, *, #38540, .T. ) ;
#9448 = DIRECTION ( 'NONE',  ( -1.416619696839552082E-11, 0.9510565162951502005, -0.3090169943749580539 ) ) ;
#9449 = CARTESIAN_POINT ( 'NONE',  ( 0.01548846960721252282, 0.2450655194478999765, 0.4674710490746267211 ) ) ;
#9450 = DIRECTION ( 'NONE',  ( 0.000000000000000000, 0.000000000000000000, -1.000000000000000000 ) ) ;
#9452 = VERTEX_POINT ( 'NONE', #9717 ) ;
#9451 = LINE ( 'NONE', #24903, #39018 ) ;
#9453 = AXIS2_PLACEMENT_3D ( 'NONE', #7906, #39205, #35486 ) ;
#9454 = ORIENTED_EDGE ( 'NONE', *, *, #22847, .F. ) ;
#9455 = CARTESIAN_POINT ( 'NONE',  ( -0.09579104668929040722, -0.04310840302197994911, 0.3749999999999998890 ) ) ;
#9456 = ORIENTED_EDGE ( 'NONE', *, *, #6182, .T. ) ;
#9457 = AXIS2_PLACEMENT_3D ( 'NONE', #4966, #17324, #30081 ) ;
#9458 = CARTESIAN_POINT ( 'NONE',  ( 0.3014272484937131624, -1.653539857075366326, 0.6572327318754673797 ) ) ;
#9460 = CARTESIAN_POINT ( 'NONE',  ( 0.1892549258828873926, -0.8411929458066104148, 0.2428197129412378030 ) ) ;
#9459 = CARTESIAN_POINT ( 'NONE',  ( 0.5185821078642816051, -1.679889620532657224, -0.4521106403573806887 ) ) ;
#9461 = CARTESIAN_POINT ( 'NONE',  ( -0.1304423469995342755, -0.5262799683630393632, 0.08499999999999922895 ) ) ;
#9462 = CARTESIAN_POINT ( 'NONE',  ( 0.01212422548420533965, -0.4367320064996455531, 0.07838015645872611903 ) ) ;
#9463 = PERSON_AND_ORGANIZATION ( #27487, #38574 ) ;
#9464 = CARTESIAN_POINT ( 'NONE',  ( 0.4140578086700125171, -1.707491598636114327, -0.4205192078341298267 ) ) ;
#9466 = EDGE_LOOP ( 'NONE', ( #12316, #20967, #35966, #31777 ) ) ;
#9465 = ORIENTED_EDGE ( 'NONE', *, *, #33873, .F. ) ;
#9467 = CARTESIAN_POINT ( 'NONE',  ( 0.4525225916027839634, -1.089042801799552374, -0.4103247334897814347 ) ) ;
#9468 = CARTESIAN_POINT ( 'NONE',  ( -0.2399999999999999079, -3.941790907013290823, -0.4709369376873030477 ) ) ;
#9469 = CARTESIAN_POINT ( 'NONE',  ( -0.2746410161513779258, -4.394818335734379744, -0.8816972205720928768 ) ) ;
#9470 = CARTESIAN_POINT ( 'NONE',  ( 0.5925686224617396913, -1.450288384180856038, 0.6546787349964396929 ) ) ;
#9471 = CARTESIAN_POINT ( 'NONE',  ( 0.1340157750494070377, -0.8309105032810858438, 0.3116155039148025274 ) ) ;
#9472 = CARTESIAN_POINT ( 'NONE',  ( 0.5368241747238033934, -1.669358818002142364, -0.4818844110413548210 ) ) ;
#9473 = VECTOR ( 'NONE', #38780, 39.37007874015748854 ) ;
#9474 = CARTESIAN_POINT ( 'NONE',  ( 0.3240187991416175750, -1.728356536110253971, 0.7856525166496111101 ) ) ;
#9475 = AXIS2_PLACEMENT_3D ( 'NONE', #13239, #22729, #7057 ) ;
#9476 = DIRECTION ( 'NONE',  ( -0.8660512985181177958, -0.4999551463232295712, 0.000000000000000000 ) ) ;
#9477 = EDGE_CURVE ( 'NONE', #14915, #19986, #33604, .T. ) ;
#9478 = CARTESIAN_POINT ( 'NONE',  ( 0.07954574449638877887, -1.328936272382664097, 0.4736275662433468425 ) ) ;
#9479 = CIRCLE ( 'NONE', #25920, 0.01500000000000001159 ) ;
#9480 = CARTESIAN_POINT ( 'NONE',  ( 0.4108705347506164118, -1.163082222544741917, 0.7368721330335714637 ) ) ;
#9481 = CARTESIAN_POINT ( 'NONE',  ( 0.07216878364870311924, 0.08000000000000023759, 0.1249999999999999029 ) ) ;
#9482 = DIRECTION ( 'NONE',  ( 0.000000000000000000, 0.000000000000000000, 1.000000000000000000 ) ) ;
#9483 = LOCAL_TIME ( 0, 53, 7.000000000000000000, #39285 ) ;
#9484 = EDGE_CURVE ( 'NONE', #18990, #38792, #14578, .T. ) ;
#9485 = CARTESIAN_POINT ( 'NONE',  ( -0.05464101615137773038, -1.659335422034822205, 0.2169804935274543545 ) ) ;
#9486 = EDGE_CURVE ( 'NONE', #22735, #24392, #15496, .T. ) ;
#9487 = LINE ( 'NONE', #12782, #17231 ) ;
#9488 = CARTESIAN_POINT ( 'NONE',  ( 0.1069896402632359023, -1.343652384576294212, 0.7022810525467199083 ) ) ;
#9489 = PERSON_AND_ORGANIZATION ( #28500, #32463 ) ;
#9490 = CIRCLE ( 'NONE', #29844, 0.1000000000000000194 ) ;
#9491 = EDGE_CURVE ( 'NONE', #23895, #19429, #22286, .T. ) ;
#9492 = CARTESIAN_POINT ( 'NONE',  ( -0.03170874437002482032, 0.4481116538287114315, 0.2027256324086049999 ) ) ;
#9493 = CARTESIAN_POINT ( 'NONE',  ( -0.3000000000000000999, -2.595429044015121534, -0.5484989581857646623 ) ) ;
#9494 = CARTESIAN_POINT ( 'NONE',  ( -0.3000000000000000999, -4.121841830394775030, -0.5449218438908057793 ) ) ;
#9495 = EDGE_CURVE ( 'NONE', #15275, #5559, #4702, .T. ) ;
#9496 = CARTESIAN_POINT ( 'NONE',  ( 0.3436318669657925096, -1.639703809451618088, -0.4374757763236017394 ) ) ;
#9497 = ORIENTED_EDGE ( 'NONE', *, *, #40301, .F. ) ;
#9498 = CARTESIAN_POINT ( 'NONE',  ( 0.01548846960707511190, -0.5346638663566677385, -0.07572681171513533094 ) ) ;
#9499 = CARTESIAN_POINT ( 'NONE',  ( 0.2695576056624507943, -1.654889899364205608, 0.7708593280864846076 ) ) ;
#9500 = EDGE_CURVE ( 'NONE', #28258, #28471, #23124, .T. ) ;
#9501 = CARTESIAN_POINT ( 'NONE',  ( 0.5949489883904641729, -1.487197279388327686, 0.5733659136327053929 ) ) ;
#9503 = VERTEX_POINT ( 'NONE', #31726 ) ;
#9502 = DIRECTION ( 'NONE',  ( -0.5000000000000003331, -6.162975822039154730E-31, -0.8660254037844383745 ) ) ;
#9504 = EDGE_CURVE ( 'NONE', #15275, #38229, #10618, .T. ) ;
#9505 = CONICAL_SURFACE ( 'NONE', #33146, 0.1500000000000009659, 1.047197551196599186 ) ;
#9506 = CARTESIAN_POINT ( 'NONE',  ( 0.4340563226180833012, -1.025953197730038458, 0.7364845616659437821 ) ) ;
#9508 = ORIENTED_EDGE ( 'NONE', *, *, #17805, .F. ) ;
#9507 = VERTEX_POINT ( 'NONE', #31127 ) ;
#9509 = CARTESIAN_POINT ( 'NONE',  ( 0.2043052629501167783, -0.6086048778238046797, 0.3675695283820143433 ) ) ;
#9510 = AXIS2_PLACEMENT_3D ( 'NONE', #3033, #21558, #34077 ) ;
#9511 = AXIS2_PLACEMENT_3D ( 'NONE', #11739, #14216, #36019 ) ;
#9512 = LINE ( 'NONE', #19935, #32244 ) ;
#9513 = APPLIED_APPROVAL_ASSIGNMENT ( #22763, ( #17414 ) ) ;
#9514 = CARTESIAN_POINT ( 'NONE',  ( 0.6343156381093978391, -1.595758837318228540, -0.5875140676452393906 ) ) ;
#9515 = DATE_AND_TIME ( #31936, #33263 ) ;
#9516 = DIRECTION ( 'NONE',  ( 0.000000000000000000, -0.6595282642760668113, -0.7516797646744246553 ) ) ;
#9517 = ORIENTED_EDGE ( 'NONE', *, *, #13262, .T. ) ;
#9518 = CARTESIAN_POINT ( 'NONE',  ( 0.08587344643816560708, -0.7676835104866827075, 0.1818131584873270978 ) ) ;
#9519 = CONICAL_SURFACE ( 'NONE', #22024, 0.1600000000000015854, 1.047197551196600296 ) ;
#9520 = DIRECTION ( 'NONE',  ( 0.8660512985181133550, 0.4999551463232370652, 0.000000000000000000 ) ) ;
#9521 = CARTESIAN_POINT ( 'NONE',  ( 0.1038461025547568750, -0.5461054185183505938, 0.1457185332388694909 ) ) ;
#9522 = CARTESIAN_POINT ( 'NONE',  ( 0.5788902524971968333, -1.608766677709437598, -0.5587703673255073333 ) ) ;
#9523 = CARTESIAN_POINT ( 'NONE',  ( -0.3000000000000000999, -3.705001275441084818, -0.3950781284944322458 ) ) ;
#9524 = VERTEX_POINT ( 'NONE', #38093 ) ;
#9525 = CARTESIAN_POINT ( 'NONE',  ( 0.4279390326040263259, -1.697518787232198179, 0.6054493271085924500 ) ) ;
#9526 = CARTESIAN_POINT ( 'NONE',  ( 0.6984602154402382856, -1.438837821160460217, 0.5667713030031571453 ) ) ;
#9527 = DIRECTION ( 'NONE',  ( 0.4999551463232373427, -0.8660512985181134660, 0.000000000000000000 ) ) ;
#9528 = CARTESIAN_POINT ( 'NONE',  ( 0.6088374871291468704, -1.478988480944025241, 0.5690365700181255759 ) ) ;
#9529 = DIRECTION ( 'NONE',  ( 1.000000000000000000, 0.000000000000000000, 1.138269997360110167E-15 ) ) ;
#9530 =( NAMED_UNIT ( * ) PLANE_ANGLE_UNIT ( ) SI_UNIT ( $, .RADIAN. ) );
#9531 = CIRCLE ( 'NONE', #32514, 0.05000000000000000971 ) ;
#9532 = EDGE_CURVE ( 'NONE', #38042, #21695, #2108, .T. ) ;
#9533 = CARTESIAN_POINT ( 'NONE',  ( 0.4091335057472371695, -1.131547141905885789, 0.4177417262808780229 ) ) ;
#9534 = CIRCLE ( 'NONE', #5561, 0.01500000000000003587 ) ;
#9535 = CARTESIAN_POINT ( 'NONE',  ( 0.07293838214825623667, -1.413098248535316070, -0.6555667331668242337 ) ) ;
#9536 = ADVANCED_FACE ( 'NONE', ( #16309 ), #37282, .T. ) ;
#9537 = CARTESIAN_POINT ( 'NONE',  ( 0.05992090360963518020, -1.332693131100006312, 0.5739722883257112329 ) ) ;
#9538 = CARTESIAN_POINT ( 'NONE',  ( 0.2974794542262550467, -0.9002722561939086043, 0.5860092920552725237 ) ) ;
#9539 = CIRCLE ( 'NONE', #8208, 0.1000000000000000194 ) ;
#9540 = SHAPE_DEFINITION_REPRESENTATION ( #20986, #30390 ) ;
#9541 = DIRECTION ( 'NONE',  ( -0.4999551463232372317, 0.8660512985181135770, -0.000000000000000000 ) ) ;
#9542 = SECURITY_CLASSIFICATION ( '', '', #29890 ) ;
#9543 = VERTEX_POINT ( 'NONE', #20205 ) ;
#9544 = CARTESIAN_POINT ( 'NONE',  ( 0.4903692945236159395, -1.545726006398236985, 0.5613691942562457626 ) ) ;
#9545 =( REPRESENTATION_RELATIONSHIP ('NONE','NONE', #27514, #25967 ) REPRESENTATION_RELATIONSHIP_WITH_TRANSFORMATION ( #38391 )SHAPE_REPRESENTATION_RELATIONSHIP( ) );
#9546 = AXIS2_PLACEMENT_3D ( 'NONE', #33310, #2048, #18090 ) ;
#9547 = CARTESIAN_POINT ( 'NONE',  ( -0.04047076529493080083, -0.06272252650431732468, 0.4973259435627372382 ) ) ;
#9548 = ORIENTED_EDGE ( 'NONE', *, *, #36368, .F. ) ;
#9549 = DIRECTION ( 'NONE',  ( -2.465190328815661892E-32, -1.000000000000000000, -6.656013887802287108E-31 ) ) ;
#9550 = CARTESIAN_POINT ( 'NONE',  ( 0.6179353394495009644, -1.299228382567916285, 0.5682417262808779901 ) ) ;
#9551 = CARTESIAN_POINT ( 'NONE',  ( 0.1851279770616925946, -0.8484560160152216923, 0.1977347518530706560 ) ) ;
#9552 = ORIENTED_EDGE ( 'NONE', *, *, #5147, .T. ) ;
#9553 = CARTESIAN_POINT ( 'NONE',  ( 0.3453377680718429099, -1.749458763706847497, 0.4498113177182618272 ) ) ;
#9554 = CARTESIAN_POINT ( 'NONE',  ( 0.1730569967620999294, -1.381888235275370080, 0.5814882153268127185 ) ) ;
#9556 = EDGE_LOOP ( 'NONE', ( #18930, #21529, #31242, #15603 ) ) ;
#9555 = ORIENTED_EDGE ( 'NONE', *, *, #19530, .F. ) ;
#9557 = FACE_OUTER_BOUND ( 'NONE', #8579, .T. ) ;
#9558 = CARTESIAN_POINT ( 'NONE',  ( 0.08146015332400738385, -1.318321297778865864, 0.4704503523288164346 ) ) ;
#9559 = CARTESIAN_POINT ( 'NONE',  ( 0.3646343803856678112, -1.994732639415563558, -0.3188592562828334587 ) ) ;
#9561 = PLANE ( 'NONE',  #3024 ) ;
#9560 = DIRECTION ( 'NONE',  ( 0.000000000000000000, 0.000000000000000000, 1.000000000000000000 ) ) ;
#9562 = CARTESIAN_POINT ( 'NONE',  ( -2.112273405726188513E-14, -1.837418632672298768, -0.6339733133327630776 ) ) ;
#9563 = ORIENTED_EDGE ( 'NONE', *, *, #15020, .T. ) ;
#9564 = CARTESIAN_POINT ( 'NONE',  ( 0.3462147144707520829, -1.728761431451053321, -0.5787996928876401048 ) ) ;
#9565 = VECTOR ( 'NONE', #25217, 39.37007874015748854 ) ;
#9566 = CARTESIAN_POINT ( 'NONE',  ( 0.09266809627140198957, -0.6152261176636174556, 0.2439027869080791222 ) ) ;
#9567 = ORIENTED_EDGE ( 'NONE', *, *, #25142, .F. ) ;
#9568 = ORIENTED_EDGE ( 'NONE', *, *, #10518, .T. ) ;
#9569 = FACE_OUTER_BOUND ( 'NONE', #522, .T. ) ;
#9570 = CARTESIAN_POINT ( 'NONE',  ( 0.07625856036271293215, -0.5806278947743503949, 0.2951979850929375426 ) ) ;
#9572 = DIRECTION ( 'NONE',  ( 0.000000000000000000, 0.000000000000000000, -1.000000000000000000 ) ) ;
#9571 = CARTESIAN_POINT ( 'NONE',  ( 0.4732169041981261759, -1.632014213049435281, -0.4230577161329019953 ) ) ;
#9573 = DIRECTION ( 'NONE',  ( 0.000000000000000000, -2.275957200481562704E-14, 1.000000000000000000 ) ) ;
#9574 = CARTESIAN_POINT ( 'NONE',  ( 0.1875000000000003331, -0.9151275355372965326, 0.1457185332388701848 ) ) ;
#9575 = APPROVAL_PERSON_ORGANIZATION ( #18670, #24017, #21572 ) ;
#9576 = DIRECTION ( 'NONE',  ( -0.8660254037844412611, 0.1781528605886697758, 0.4671847153579293810 ) ) ;
#9577 = B_SPLINE_CURVE_WITH_KNOTS ( 'NONE', 3,
 ( #33300, #30209, #1658, #5107, #17662, #35575, #26330, #4693 ),
 .UNSPECIFIED., .F., .F.,
 ( 4, 2, 2, 4 ),
 ( -6.000000000156461008E-08, 0.0008322485881172374776, 0.001664557176234476550, 0.003329174352468955780 ),
 .UNSPECIFIED. ) ;
#9578 = CARTESIAN_POINT ( 'NONE',  ( 0.1153529736793553612, -0.4467512060742309665, 0.1565319484199297895 ) ) ;
#9579 = CARTESIAN_POINT ( 'NONE',  ( 0.5802862917196511816, -1.495087218360813042, 0.5610704458703436037 ) ) ;
#9580 = CARTESIAN_POINT ( 'NONE',  ( -0.05634115714581183765, 0.2739512608647006742, -0.3681776108866004482 ) ) ;
#9581 = CARTESIAN_POINT ( 'NONE',  ( -0.2300000000000004818, 0.5182417262804733804, 0.3599999999999999867 ) ) ;
#9582 = CARTESIAN_POINT ( 'NONE',  ( -0.03303708955568357419, -0.4610021654188251605, -0.2426024699083967617 ) ) ;
#9583 = CARTESIAN_POINT ( 'NONE',  ( 0.06923712653936904549, -0.5400029222721455247, 0.1457185332388703236 ) ) ;
#9584 = DIRECTION ( 'NONE',  ( 0.000000000000000000, 0.8438867430782092116, 0.5365213554527465956 ) ) ;
#9585 = CARTESIAN_POINT ( 'NONE',  ( 0.2968044078846433509, -0.7977486025825716309, 0.6363905851602879027 ) ) ;
#9586 = CARTESIAN_POINT ( 'NONE',  ( -0.04762200653274744483, 0.3170437565186472462, 0.3633076762442032370 ) ) ;
#9587 = CARTESIAN_POINT ( 'NONE',  ( 0.02584783977369822794, -1.092114942298472169, 0.6499590385907687562 ) ) ;
#9588 = CLOSED_SHELL ( 'NONE', ( #26324, #21348, #25064, #36128, #2152, #8176 ) ) ;
#9589 = CARTESIAN_POINT ( 'NONE',  ( 0.6025502600592794744, -1.571821872759174621, -0.4181649500142127773 ) ) ;
#9590 = CIRCLE ( 'NONE', #12887, 0.5400000000000007017 ) ;
#9591 = CARTESIAN_POINT ( 'NONE',  ( 0.3918182118607624331, -1.107073211027153725, 0.6042946153017959565 ) ) ;
#9592 = CARTESIAN_POINT ( 'NONE',  ( 0.08435616334553369677, -0.8469091540353979042, 0.3709842075955784857 ) ) ;
#9593 = PLANE ( 'NONE',  #37636 ) ;
#9594 = CARTESIAN_POINT ( 'NONE',  ( 0.1893026375364066649, -1.254248048989826225, -0.6328096728701395612 ) ) ;
#9595 = SECURITY_CLASSIFICATION ( '', '', #15495 ) ;
#9596 = VERTEX_POINT ( 'NONE', #4349 ) ;
#9597 = CARTESIAN_POINT ( 'NONE',  ( 0.3599725030089058753, -1.738129011639496291, -0.5054791832264183826 ) ) ;
#9598 = CARTESIAN_POINT ( 'NONE',  ( 0.3779900952041616025, -1.610792511722474840, -0.4148273735560925601 ) ) ;
#9599 = CARTESIAN_POINT ( 'NONE',  ( 0.6544078563150441674, -1.544269123161570390, 0.4241055859090137603 ) ) ;
#9600 = CARTESIAN_POINT ( 'NONE',  ( 0.5358573072157438721, -1.635276992059453427, -0.4933326546058601769 ) ) ;
#9601 = CARTESIAN_POINT ( 'NONE',  ( -1.502516396515344672E-15, -0.3899999999999999578, 0.04000000000000055594 ) ) ;
#9602 = CIRCLE ( 'NONE', #33935, 0.1012268159172230869 ) ;
#9603 = ORIENTED_EDGE ( 'NONE', *, *, #34902, .F. ) ;
#9604 = CARTESIAN_POINT ( 'NONE',  ( 0.3740544490715725923, -1.618991780640511635, -0.6658790255296196392 ) ) ;
#9605 =( BOUNDED_SURFACE ( )  B_SPLINE_SURFACE ( 3, 2, ( 
 ( #33193, #29697, #20047 ),
 ( #36482, #8295, #7688 ),
 ( #26417, #30107, #35665 ),
 ( #20252, #36261, #20867 ) ),
 .UNSPECIFIED., .F., .F., .T. ) 
 B_SPLINE_SURFACE_WITH_KNOTS ( ( 4, 4 ),
 ( 3, 3 ),
 ( 7.502679033599690683E-16, 0.004712633340305917920 ),
 ( 0.000000000000000000, 1.000000000000000000 ),
 .UNSPECIFIED. ) 
 GEOMETRIC_REPRESENTATION_ITEM ( )  RATIONAL_B_SPLINE_SURFACE ( (
 ( 1.000000000000000000, 0.7064740011956678334, 1.000000000000000000),
 ( 1.000000000000000000, 0.7068967119107782970, 1.000000000000000000),
 ( 1.000000000000000000, 0.7076183925776566852, 1.000000000000000000),
 ( 1.000000000000000000, 0.7079223141425841082, 1.000000000000000000) ) ) 
 REPRESENTATION_ITEM ( '' )  SURFACE ( )  );
#9606 = CARTESIAN_POINT ( 'NONE',  ( 0.2950576522027442139, -1.312148821418196443, 0.5683580896351703160 ) ) ;
#9607 = CARTESIAN_POINT ( 'NONE',  ( -0.2399999999999999079, -3.478759481804464038, -0.3573324461326447543 ) ) ;
#9608 = CARTESIAN_POINT ( 'NONE',  ( 0.000000000000000000, -0.02383748379410547888, -0.1985743547550029575 ) ) ;
#9609 = CARTESIAN_POINT ( 'NONE',  ( 0.3940236569407176148, -1.140246238217890840, 0.7425364925414594808 ) ) ;
#9611 = DIRECTION ( 'NONE',  ( 8.881784197001246407E-16, -2.361472542561082612E-16, 1.000000000000000000 ) ) ;
#9610 = CARTESIAN_POINT ( 'NONE',  ( 0.2614468074032732514, -0.7584085742687330933, 0.1932256475537141860 ) ) ;
#9612 = CARTESIAN_POINT ( 'NONE',  ( 0.4871018846440973715, -1.079508789421436799, 0.5988988590622403851 ) ) ;
#9613 = ORIENTED_EDGE ( 'NONE', *, *, #30340, .T. ) ;
#9614 = PERSON_AND_ORGANIZATION_ROLE ( 'creator' ) ;
#9615 = CARTESIAN_POINT ( 'NONE',  ( 0.4123503261003252374, -1.705581556875543914, -0.3887263060331934139 ) ) ;
#9616 = VERTEX_POINT ( 'NONE', #32930 ) ;
#9617 = B_SPLINE_CURVE_WITH_KNOTS ( 'NONE', 3,
 ( #22570, #34688, #19511, #3819, #32201, #4015, #12471, #28915, #38377, #780, #25644, #38174, #25236, #31412, #28126, #13286, #3416, #25026, #37558, #35100, #9792, #6493, #15975, #21962 ),
 .UNSPECIFIED., .F., .F.,
 ( 4, 2, 2, 2, 2, 2, 2, 2, 2, 2, 2, 4 ),
 ( 3.541895844777533420E-16, 0.001886868708433897144, 0.002830303062650669967, 0.003773737416867442140, 0.005660606125300986918, 0.006604040479517757356, 0.007547474833734527794, 0.008490909187951298231, 0.009434343542168068669, 0.01132121225060160261, 0.01320808095903513654, 0.01509494966746866874 ),
 .UNSPECIFIED. ) ;
#9618 = ORIENTED_EDGE ( 'NONE', *, *, #820, .F. ) ;
#9619 = CARTESIAN_POINT ( 'NONE',  ( 0.1999031773436300563, -1.118309514668103466, 0.8646612173229440979 ) ) ;
#9621 = CARTESIAN_POINT ( 'NONE',  ( 0.1755124995118596265, -0.7841637173364213176, -0.06301638288098621032 ) ) ;
#9620 = CARTESIAN_POINT ( 'NONE',  ( 0.08622878581753390392, -0.7696919062817791923, 0.05383970079421885463 ) ) ;
#9622 = CARTESIAN_POINT ( 'NONE',  ( 0.1929960976912158399, -1.971902824862748593, -0.3252172897420532727 ) ) ;
#9623 = ORIENTED_EDGE ( 'NONE', *, *, #11931, .T. ) ;
#9624 = ORIENTED_EDGE ( 'NONE', *, *, #216, .F. ) ;
#9625 = TOROIDAL_SURFACE ( 'NONE', #33924, 0.1333070866141734256, 0.02999999999999999889 ) ;
#9626 = CARTESIAN_POINT ( 'NONE',  ( 0.1266021694322588542, -1.239399129679921829, 0.5182417262812423209 ) ) ;
#9627 = CARTESIAN_POINT ( 'NONE',  ( 0.5674053191207506508, -1.503247083075981205, 0.5820947328701803203 ) ) ;
#9628 = ORIENTED_EDGE ( 'NONE', *, *, #19319, .T. ) ;
#9629 = CARTESIAN_POINT ( 'NONE',  ( 0.01251651876921019806, -0.9543982913104013255, 0.3144092334379698372 ) ) ;
#9630 = DIRECTION ( 'NONE',  ( 1.000000000000000000, 0.000000000000000000, 0.000000000000000000 ) ) ;
#9631 = DIRECTION ( 'NONE',  ( 0.3468893892380796040, 0.3199132558029604834, -0.8816593788961709643 ) ) ;
#9632 = ORGANIZATION ( 'NAUO-ORG11', 'UNSPECIFIED', 'UNSPECIFIED' ) ;
#9633 = DIRECTION ( 'NONE',  ( 7.771561172376107616E-16, -7.170354002788761615E-17, 1.000000000000000000 ) ) ;
#9634 = DIRECTION ( 'NONE',  ( -1.000000000000000000, 0.000000000000000000, 0.000000000000000000 ) ) ;
#9635 = CARTESIAN_POINT ( 'NONE',  ( -0.1127323924368537483, -0.5155369761421360053, 0.3191796960528350824 ) ) ;
#9636 = CARTESIAN_POINT ( 'NONE',  ( 0.1185062575666918222, -1.414355497448371413, 0.4982023605334466865 ) ) ;
#9637 = CIRCLE ( 'NONE', #33296, 0.1033070866141734129 ) ;
#9638 = CARTESIAN_POINT ( 'NONE',  ( 2.048885995248197414E-16, 0.2981948553318907735, -1.707404996040164512E-16 ) ) ;
#9639 = CARTESIAN_POINT ( 'NONE',  ( 0.3999999999999783729, -2.097675824466503691, -0.5196396315034579327 ) ) ;
#9640 = CARTESIAN_POINT ( 'NONE',  ( 0.1037868704622257193, -1.285705572052544543, 0.6122442384440756058 ) ) ;
#9641 = EDGE_CURVE ( 'NONE', #29368, #13497, #16910, .T. ) ;
#9642 = CARTESIAN_POINT ( 'NONE',  ( 0.07652314640228294329, -2.107936428766273629, -0.7005084057759866090 ) ) ;
#9643 = CARTESIAN_POINT ( 'NONE',  ( 0.1133199752903892021, -1.408071044610375466, 0.6174663899997400174 ) ) ;
#9644 = APPROVAL_DATE_TIME ( #18915, #40334 ) ;
#9645 = APPLIED_PERSON_AND_ORGANIZATION_ASSIGNMENT ( #24160, #38092, ( #31951 ) ) ;
#9646 = CARTESIAN_POINT ( 'NONE',  ( 0.3238203105384647174, -0.9899218032796638367, 0.5856430185708639824 ) ) ;
#9647 = CARTESIAN_POINT ( 'NONE',  ( 0.3190393728410141350, -1.171751842138375244, 0.4809317249889470958 ) ) ;
#9648 = CARTESIAN_POINT ( 'NONE',  ( 0.5435131371594662530, -1.168890700092135804, 0.6057417262810184111 ) ) ;
#9649 = CARTESIAN_POINT ( 'NONE',  ( -0.1743922129835729085, -0.5166151207188712791, 0.3750000000000001110 ) ) ;
#9650 = CARTESIAN_POINT ( 'NONE',  ( 0.02591418161326580066, -1.064383994110095877, 0.6545759956939124491 ) ) ;
#9651 = CARTESIAN_POINT ( 'NONE',  ( -8.431455208089989601E-05, -0.7678062237554516001, -0.09016270909632642661 ) ) ;
#9652 = CARTESIAN_POINT ( 'NONE',  ( 0.6790301733516745930, -1.437036692487801526, 0.4793159731800502588 ) ) ;
#9653 = VECTOR ( 'NONE', #35856, 39.37007874015748143 ) ;
#9654 = DIRECTION ( 'NONE',  ( 0.000000000000000000, 0.9437421848352475218, -0.3306821564015722803 ) ) ;
#9655 = ORIENTED_EDGE ( 'NONE', *, *, #37754, .F. ) ;
#9656 = EDGE_LOOP ( 'NONE', ( #8521, #4448, #26641, #34495 ) ) ;
#9657 = CYLINDRICAL_SURFACE ( 'NONE', #34832, 0.1000000000000000056 ) ;
#9658 = ORIENTED_EDGE ( 'NONE', *, *, #37555, .T. ) ;
#9659 = LINE ( 'NONE', #13742, #740 ) ;
#9660 = CARTESIAN_POINT ( 'NONE',  ( -0.05083665881508995371, -0.4630607685881625857, -0.09936361682460898015 ) ) ;
#9661 = CARTESIAN_POINT ( 'NONE',  ( 0.6164308040309282033, -1.473203056481420692, 0.5449326099368130283 ) ) ;
#9662 = B_SPLINE_CURVE_WITH_KNOTS ( 'NONE', 3,
 ( #23483, #24086, #17875, #37007, #36193, #8007, #30650, #33718, #36402, #27561 ),
 .UNSPECIFIED., .F., .F.,
 ( 4, 2, 2, 2, 4 ),
 ( 0.0001365264101772900964, 0.0006734250193805398814, 0.001210323628583789531, 0.001747222237787039289, 0.002284120846990289264 ),
 .UNSPECIFIED. ) ;
#9664 = ORIENTED_EDGE ( 'NONE', *, *, #6230, .F. ) ;
#9663 = CARTESIAN_POINT ( 'NONE',  ( -0.1059790098053068758, -0.4816261856389994489, 0.09813923389061053604 ) ) ;
#9665 = ADVANCED_FACE ( 'NONE', ( #13804 ), #35419, .T. ) ;
#9666 = VERTEX_POINT ( 'NONE', #19997 ) ;
#9667 = CARTESIAN_POINT ( 'NONE',  ( 0.2028766461682649236, -0.6553055420477189585, 0.3449445657290035050 ) ) ;
#9668 = ADVANCED_FACE ( 'NONE', ( #1107 ), #29454, .F. ) ;
#9669 = ORIENTED_EDGE ( 'NONE', *, *, #25370, .F. ) ;
#9670 = CARTESIAN_POINT ( 'NONE',  ( 0.01099302296002880285, -0.5422623884125030713, 0.2194225212593840790 ) ) ;
#9672 = CARTESIAN_POINT ( 'NONE',  ( 0.07975072596342917819, -1.320959035748987098, 0.5731222016746064796 ) ) ;
#9671 = CARTESIAN_POINT ( 'NONE',  ( 0.2498278802431492807, -0.9843056470458266816, 0.7020538874898170079 ) ) ;
#9673 = CARTESIAN_POINT ( 'NONE',  ( 0.3925301276612754298, -1.756377271995033684, -0.4843757382520948451 ) ) ;
#9674 = CARTESIAN_POINT ( 'NONE',  ( 0.1870989724938920962, -0.8266995537623093027, -0.08446770797961487831 ) ) ;
#9675 = DATE_AND_TIME ( #25104, #36616 ) ;
#9676 = EDGE_CURVE ( 'NONE', #22855, #19587, #13269, .T. ) ;
#9677 = ADVANCED_FACE ( 'NONE', ( #29650 ), #16567, .T. ) ;
#9678 = FACE_OUTER_BOUND ( 'NONE', #8187, .T. ) ;
#9680 = ORIENTED_EDGE ( 'NONE', *, *, #23081, .F. ) ;
#9679 = ORIENTED_EDGE ( 'NONE', *, *, #14080, .T. ) ;
#9681 = ADVANCED_FACE ( 'NONE', ( #7641 ), #30326, .F. ) ;
#9682 = DIRECTION ( 'NONE',  ( 0.000000000000000000, 1.000000000000000000, -3.330669073875470607E-16 ) ) ;
#9683 = CARTESIAN_POINT ( 'NONE',  ( 0.1856930765046928833, -0.8391312611259635901, 0.1792070938244055278 ) ) ;
#9684 = CARTESIAN_POINT ( 'NONE',  ( 0.1999999999999786393, -2.081198020765314460, -0.7227018020631825745 ) ) ;
#9685 = CARTESIAN_POINT ( 'NONE',  ( 0.5611967014548586707, -1.396901917415622973, 0.7440408781994463094 ) ) ;
#9686 = CARTESIAN_POINT ( 'NONE',  ( 0.1483787585013065236, -0.8436283734347517216, 0.4121418770343379112 ) ) ;
#9687 = CARTESIAN_POINT ( 'NONE',  ( 0.2658650419925461250, -1.607106637764143420, 0.8265052428267256612 ) ) ;
#9688 = CARTESIAN_POINT ( 'NONE',  ( 0.3253107118822870514, -1.742078995693881138, 0.7432966274578529653 ) ) ;
#9689 = PLANE ( 'NONE',  #13321 ) ;
#9690 = CARTESIAN_POINT ( 'NONE',  ( 0.07734939284328633258, -1.330214815144483698, 0.4791517717473012805 ) ) ;
#9691 = CARTESIAN_POINT ( 'NONE',  ( 0.1850732001874748345, -0.8229804149772106392, 0.1457185332388700183 ) ) ;
#9692 = EDGE_CURVE ( 'NONE', #9666, #3317, #10947, .T. ) ;
#9693 = DIRECTION ( 'NONE',  ( 4.503376743791639448E-15, 0.9613939893712163398, -0.2751755752258865373 ) ) ;
#9694 = DIRECTION ( 'NONE',  ( -0.3571676571814509371, -0.2061861792870984811, -0.9109986411265946771 ) ) ;
#9695 = CARTESIAN_POINT ( 'NONE',  ( 0.01548846960706648165, -0.3688619771573060646, 0.3775276577327108529 ) ) ;
#9696 = CARTESIAN_POINT ( 'NONE',  ( 0.002083146443013456344, -0.4777046557262296100, 0.09357736723029726200 ) ) ;
#9697 = CARTESIAN_POINT ( 'NONE',  ( 0.1857471242690073021, -1.941376881060412174, -0.6624637124125288823 ) ) ;
#9698 = PERSON_AND_ORGANIZATION_ROLE ( 'design_owner' ) ;
#9699 = CARTESIAN_POINT ( 'NONE',  ( -0.04157078424165206593, 0.4522175634759015850, 0.1290209392672064526 ) ) ;
#9700 = CARTESIAN_POINT ( 'NONE',  ( 0.6817109428167473784, -1.507712782526625883, 0.4506074055298545655 ) ) ;
#9701 = ORIENTED_EDGE ( 'NONE', *, *, #20550, .F. ) ;
#9702 = DIRECTION ( 'NONE',  ( -0.000000000000000000, -0.6595282642760673664, -0.7516797646744242112 ) ) ;
#9703 = ORIENTED_EDGE ( 'NONE', *, *, #38815, .F. ) ;
#9704 = CARTESIAN_POINT ( 'NONE',  ( 0.4450935511747624584, -1.144980177316206049, -0.3864693716766450793 ) ) ;
#9705 = CARTESIAN_POINT ( 'NONE',  ( 0.1911888169624559319, -1.364106057445899856, 0.9496954658188896392 ) ) ;
#9706 = CARTESIAN_POINT ( 'NONE',  ( 0.3701761278964109114, -1.124337411362599015, 0.8051996703508850217 ) ) ;
#9708 = ORIENTED_EDGE ( 'NONE', *, *, #38475, .T. ) ;
#9707 = CARTESIAN_POINT ( 'NONE',  ( 0.3577715969228448256, -1.744183799078588226, 0.4401225512775638338 ) ) ;
#9710 = ORIENTED_EDGE ( 'NONE', *, *, #12462, .F. ) ;
#9709 = VERTEX_POINT ( 'NONE', #5766 ) ;
#9711 = CARTESIAN_POINT ( 'NONE',  ( 0.2484857473122377980, -1.339293634572156000, -0.5155029497116575543 ) ) ;
#9712 = EDGE_CURVE ( 'NONE', #2630, #17210, #39531, .T. ) ;
#9713 = ORIENTED_EDGE ( 'NONE', *, *, #39876, .F. ) ;
#9714 = CARTESIAN_POINT ( 'NONE',  ( 0.6315454840034280259, -1.614677985444239239, -0.5441907603584862363 ) ) ;
#9715 = DATE_AND_TIME ( #37903, #10928 ) ;
#9716 = EDGE_CURVE ( 'NONE', #8839, #3591, #2239, .T. ) ;
#9717 = CARTESIAN_POINT ( 'NONE',  ( 0.1802350563441833808, -0.5022327775090948965, 0.1477559389858786043 ) ) ;
#9718 = EDGE_LOOP ( 'NONE', ( #21043, #25155, #22730, #36158, #20915, #14977, #14939, #36765 ) ) ;
#9719 = EDGE_CURVE ( 'NONE', #38543, #12918, #2736, .T. ) ;
#9720 = CARTESIAN_POINT ( 'NONE',  ( 0.1691926429880553362, -0.8469287021894142953, 0.5696781129675587696 ) ) ;
#9721 = DIRECTION ( 'NONE',  ( 1.000000000000000000, 0.000000000000000000, 0.000000000000000000 ) ) ;
#9722 = CARTESIAN_POINT ( 'NONE',  ( 0.5257712170263993956, -1.526907663539789572, 0.5830379435895678419 ) ) ;
#9723 = CARTESIAN_POINT ( 'NONE',  ( -0.02000000000000000042, -2.183180860297908144, -0.5562760292030870524 ) ) ;
#9724 = CARTESIAN_POINT ( 'NONE',  ( -0.1603938765018643187, 0.4636889572248043545, 0.1178658435936973670 ) ) ;
#9725 = EDGE_LOOP ( 'NONE', ( #14989, #34786, #40622, #24019 ) ) ;
#9726 = CARTESIAN_POINT ( 'NONE',  ( 0.4395714512744828273, -1.702217766737038174, 0.6022144385477095074 ) ) ;
#9727 = CARTESIAN_POINT ( 'NONE',  ( 0.6399309177019067985, -1.482104228856624406, 0.8013445891425567957 ) ) ;
#9728 = CARTESIAN_POINT ( 'NONE',  ( 0.08016251834805442067, -1.309203902574839207, 0.5631135398343307674 ) ) ;
#9729 = CARTESIAN_POINT ( 'NONE',  ( 0.2558199171275122308, -0.8856984187707415135, 0.6867119623177011523 ) ) ;
#9730 = CARTESIAN_POINT ( 'NONE',  ( 0.06980746140711582837, 0.000000000000000000, 0.000000000000000000 ) ) ;
#9731 = EDGE_CURVE ( 'NONE', #23498, #2485, #26799, .T. ) ;
#9732 =( LENGTH_UNIT ( ) NAMED_UNIT ( * ) SI_UNIT ( $, .METRE. ) );
#9733 = EDGE_CURVE ( 'NONE', #28983, #23947, #38223, .T. ) ;
#9734 = DIRECTION ( 'NONE',  ( 0.000000000000000000, -0.9510565162951585272, 0.3090169943749324633 ) ) ;
#9735 = EDGE_CURVE ( 'NONE', #34794, #35264, #9074, .T. ) ;
#9736 = CARTESIAN_POINT ( 'NONE',  ( 0.01895494625228212604, -0.4667936258712412911, -0.2292799240428205210 ) ) ;
#9737 = DIRECTION ( 'NONE',  ( 1.000000000000000000, 2.341930812374887555E-31, -1.664003471950578127E-31 ) ) ;
#9738 = CARTESIAN_POINT ( 'NONE',  ( 0.2017226021742919428, -0.8083333955854449249, 0.3447374551949819454 ) ) ;
#9739 = DATE_AND_TIME ( #29061, #28615 ) ;
#9740 = DIRECTION ( 'NONE',  ( 0.8660512985181135770, 0.4999551463232371207, 1.024644699336566956E-15 ) ) ;
#9741 = DIRECTION ( 'NONE',  ( 0.000000000000000000, 0.3882559824134195758, -0.9215515678030125057 ) ) ;
#9742 = CARTESIAN_POINT ( 'NONE',  ( -0.04945776359514338083, -0.03517487494623300348, 0.4760216296475739406 ) ) ;
#9743 = ORIENTED_EDGE ( 'NONE', *, *, #21070, .T. ) ;
#9744 = CARTESIAN_POINT ( 'NONE',  ( 0.4322485342602996883, -1.579783117282272720, 0.5939163760578864970 ) ) ;
#9745 = DIRECTION ( 'NONE',  ( -1.000000000000000000, -2.280301054154496446E-31, -1.355854680848613603E-31 ) ) ;
#9746 = CARTESIAN_POINT ( 'NONE',  ( 0.08536139700232568683, -0.8064920420962284897, 0.1131592819080732837 ) ) ;
#9747 = ORIENTED_EDGE ( 'NONE', *, *, #20572, .F. ) ;
#9748 = FACE_OUTER_BOUND ( 'NONE', #7315, .T. ) ;
#9749 = CARTESIAN_POINT ( 'NONE',  ( 0.1402368025282916819, -1.302452809619852436, 0.7172172189790673169 ) ) ;
#9751 = ORIENTED_EDGE ( 'NONE', *, *, #35938, .F. ) ;
#9750 = ORIENTED_EDGE ( 'NONE', *, *, #1971, .T. ) ;
#9752 = FACE_OUTER_BOUND ( 'NONE', #12585, .T. ) ;
#9753 = ORIENTED_EDGE ( 'NONE', *, *, #29028, .T. ) ;
#9754 = DIRECTION ( 'NONE',  ( -1.000000000000000000, -2.280301054154495132E-31, 1.664003471950577689E-31 ) ) ;
#9755 = FACE_OUTER_BOUND ( 'NONE', #8934, .T. ) ;
#9756 = EDGE_CURVE ( 'NONE', #8954, #35941, #5345, .T. ) ;
#9758 = CARTESIAN_POINT ( 'NONE',  ( 0.4170115945640069932, -1.702980413955156758, -0.6123808887097255127 ) ) ;
#9757 = CARTESIAN_POINT ( 'NONE',  ( 0.6011812487780853198, -1.595544227086114653, 0.4276680258713908001 ) ) ;
#9759 = CARTESIAN_POINT ( 'NONE',  ( 0.05201782277453038256, -0.2617104306118866464, -0.3909705171288733738 ) ) ;
#9760 = VERTEX_POINT ( 'NONE', #11553 ) ;
#9761 = CARTESIAN_POINT ( 'NONE',  ( -0.03159140494780148661, 0.3316214887069900419, -0.3635694333040939141 ) ) ;
#9762 = VERTEX_POINT ( 'NONE', #29862 ) ;
#9763 = ORIENTED_EDGE ( 'NONE', *, *, #1920, .T. ) ;
#9764 = CARTESIAN_POINT ( 'NONE',  ( 0.09001134929717277688, -0.6059489090321513727, 0.1642870258393102911 ) ) ;
#9765 = ORIENTED_EDGE ( 'NONE', *, *, #37029, .T. ) ;
#9766 = CARTESIAN_POINT ( 'NONE',  ( 0.01053196809506632727, -0.5372589727095348211, 0.4763883693587342427 ) ) ;
#9767 = CARTESIAN_POINT ( 'NONE',  ( 0.4417054119102772902, -1.573775560800656059, 0.5739987501060517250 ) ) ;
#9769 = CARTESIAN_POINT ( 'NONE',  ( 0.1987206965304505746, -1.209313118825164235, 0.5182417262812423209 ) ) ;
#9768 = CARTESIAN_POINT ( 'NONE',  ( 0.003322744920643190894, -0.5573345580546938960, 0.2952108599035634939 ) ) ;
#9770 = CARTESIAN_POINT ( 'NONE',  ( 0.005974780502986185536, -0.8455926682250717308, 0.1923417552807378805 ) ) ;
#9771 = CARTESIAN_POINT ( 'NONE',  ( 0.1804200693113137133, -0.9232518763482380209, 0.2929062103565514552 ) ) ;
#9772 = DIRECTION ( 'NONE',  ( 0.4999999999999972800, -0.5122356157878119598, -0.6982941170584811008 ) ) ;
#9773 = CARTESIAN_POINT ( 'NONE',  ( 0.4271757566612302548, -1.700307850918723274, -0.5150901720920313398 ) ) ;
#9774 = CARTESIAN_POINT ( 'NONE',  ( 0.5813445478835994606, -1.495260542201000131, 0.5817699383783053735 ) ) ;
#9775 = CARTESIAN_POINT ( 'NONE',  ( -0.02953079040095687308, 0.3810518745593911571, 0.3687679460475725701 ) ) ;
#9776 = PLANE ( 'NONE',  #26451 ) ;
#9777 = CARTESIAN_POINT ( 'NONE',  ( -0.03474824846561417463, -0.4640677240217945809, -0.2268448004460654477 ) ) ;
#9778 = EDGE_CURVE ( 'NONE', #7881, #14101, #24116, .T. ) ;
#9779 = CARTESIAN_POINT ( 'NONE',  ( 0.07240097019314004068, -0.5694418211797861451, 0.2666026808772828938 ) ) ;
#9780 = SPHERICAL_SURFACE ( 'NONE', #6267, 0.01499999999999999944 ) ;
#9781 = EDGE_CURVE ( 'NONE', #21164, #28482, #32961, .T. ) ;
#9782 = CARTESIAN_POINT ( 'NONE',  ( 0.5969179818652998737, -1.265625243575819514, 0.7915741918176316672 ) ) ;
#9783 = CARTESIAN_POINT ( 'NONE',  ( 0.4516518293581444632, -1.119247471017704942, 0.5164366663489963205 ) ) ;
#9784 = CARTESIAN_POINT ( 'NONE',  ( 0.05499745022826314084, -1.300966059534855113, 0.6243749980364792229 ) ) ;
#9785 = CARTESIAN_POINT ( 'NONE',  ( 0.05268932808079793140, 0.4428506128075155868, -0.1535014714533980418 ) ) ;
#9786 = DIRECTION ( 'NONE',  ( 1.000000000000000000, 0.000000000000000000, 0.000000000000000000 ) ) ;
#9787 = DIRECTION ( 'NONE',  ( 0.000000000000000000, 0.9396926207858876667, -0.3420201433257257229 ) ) ;
#9788 = LINE ( 'NONE', #18869, #13991 ) ;
#9789 = CARTESIAN_POINT ( 'NONE',  ( 0.6954966302589218330, -1.498494318102867595, 0.4775031782631350974 ) ) ;
#9790 = ORIENTED_EDGE ( 'NONE', *, *, #29588, .T. ) ;
#9791 = CARTESIAN_POINT ( 'NONE',  ( 0.05999999999999990757, -0.004731704300309400382, -0.008387989767859833218 ) ) ;
#9792 = CARTESIAN_POINT ( 'NONE',  ( 0.3877735588591806337, -1.128227633100496785, 0.7844172370806664629 ) ) ;
#9793 = CARTESIAN_POINT ( 'NONE',  ( 0.6672745098620159743, -1.495646976912385906, 0.4226893254941921363 ) ) ;
#9794 = CARTESIAN_POINT ( 'NONE',  ( 0.5584481223773475334, -1.622235738823061491, -0.4750859664929777404 ) ) ;
#9795 = CARTESIAN_POINT ( 'NONE',  ( -0.05634304521267749499, -0.01028123094841905914, 0.4588823192046724841 ) ) ;
#9796 = ORIENTED_EDGE ( 'NONE', *, *, #14316, .F. ) ;
#9797 = DIRECTION ( 'NONE',  ( 0.000000000000000000, 0.2751755752258863708, 0.9613939893712163398 ) ) ;
#9798 = DIRECTION ( 'NONE',  ( 0.8660512985181126888, 0.4999551463232384529, 0.000000000000000000 ) ) ;
#9799 = DIRECTION ( 'NONE',  ( 7.771561172376107616E-16, -7.170354002788761615E-17, 1.000000000000000000 ) ) ;
#9800 = CARTESIAN_POINT ( 'NONE',  ( 0.1499999999999993561, 0.09061086148575100974, -0.5171215251571038563 ) ) ;
#9801 = CARTESIAN_POINT ( 'NONE',  ( 0.4865325576204800884, -1.269899856794043824, 0.6586424791840079784 ) ) ;
#9802 = EDGE_CURVE ( 'NONE', #20865, #10794, #39314, .T. ) ;
#9804 = CARTESIAN_POINT ( 'NONE',  ( 0.5779297624755960205, -1.623152544610868109, 0.5629341535590222101 ) ) ;
#9803 = DIRECTION ( 'NONE',  ( -1.000000000000000000, 9.772892703439654860E-15, -7.801168736956215639E-16 ) ) ;
#9805 = CARTESIAN_POINT ( 'NONE',  ( 0.4003901567941702822, -1.031933045472551269, 0.6312919426632347397 ) ) ;
#9806 = ORIENTED_EDGE ( 'NONE', *, *, #37813, .T. ) ;
#9807 = CALENDAR_DATE ( 2026, 13, 10 ) ;
#9808 = CARTESIAN_POINT ( 'NONE',  ( -0.002282498291095993656, -0.8555267327002353817, 0.1457185332388701293 ) ) ;
#9809 = VERTEX_POINT ( 'NONE', #36433 ) ;
#9810 = VERTEX_POINT ( 'NONE', #30676 ) ;
#9811 = CARTESIAN_POINT ( 'NONE',  ( 0.3728324473123414973, -1.558310038709751710, 0.7835862474759246465 ) ) ;
#9813 = CYLINDRICAL_SURFACE ( 'NONE', #24215, 0.1033070866141734129 ) ;
#9812 = CARTESIAN_POINT ( 'NONE',  ( 0.08541475502865693292, -0.8049639420879202145, 0.1080243483262872811 ) ) ;
#9814 = CARTESIAN_POINT ( 'NONE',  ( 0.3404871394918290717, -1.648910532809566787, -0.3823052341430687728 ) ) ;
#9815 = B_SPLINE_CURVE_WITH_KNOTS ( 'NONE', 3,
 ( #39077, #10904, #23474, #4502, #32697, #32887 ),
 .UNSPECIFIED., .F., .F.,
 ( 4, 2, 4 ),
 ( 0.000000000000000000, 0.0006158527847097438647, 0.001231705569419487729 ),
 .UNSPECIFIED. ) ;
#9816 = ORIENTED_EDGE ( 'NONE', *, *, #5165, .F. ) ;
#9817 = ORIENTED_EDGE ( 'NONE', *, *, #21009, .T. ) ;
#9818 = ORIENTED_EDGE ( 'NONE', *, *, #23072, .T. ) ;
#9819 = DIRECTION ( 'NONE',  ( 5.546678239835219551E-32, 0.9849933812516251663, -0.1725921171157328571 ) ) ;
#9820 = CARTESIAN_POINT ( 'NONE',  ( 0.1252239888084831498, -0.6131032844985105923, 0.3504799705789324871 ) ) ;
#9821 = ORIENTED_EDGE ( 'NONE', *, *, #35879, .T. ) ;
#9822 = CARTESIAN_POINT ( 'NONE',  ( 0.07014435923140931173, -1.325199841737229711, 0.5075297796643253312 ) ) ;
#9823 = CARTESIAN_POINT ( 'NONE',  ( -0.2746410161513776482, -4.385325017590463226, -0.5985264029706663935 ) ) ;
#9824 = DIRECTION ( 'NONE',  ( 1.000000000000000000, 2.280301054154495132E-31, -1.664003471950577689E-31 ) ) ;
#9825 = CARTESIAN_POINT ( 'NONE',  ( 0.1863335705363715067, -0.7656576722580051841, 0.1913830803212247800 ) ) ;
#9826 = FACE_OUTER_BOUND ( 'NONE', #32731, .T. ) ;
#9827 = CARTESIAN_POINT ( 'NONE',  ( 0.3311983384110263606, -1.753850171096680288, 0.5836116394440121757 ) ) ;
#9828 = DIRECTION ( 'NONE',  ( 0.000000000000000000, 0.7185945389471846134, 0.6954292836768403152 ) ) ;
#9829 = DIRECTION ( 'NONE',  ( 1.000000000000000000, -0.000000000000000000, -0.000000000000000000 ) ) ;
#9830 = CARTESIAN_POINT ( 'NONE',  ( 0.3961214603528522837, -2.010890533879527098, -0.7066937474304769706 ) ) ;
#9831 = LINE ( 'NONE', #6132, #5374 ) ;
#9832 = CARTESIAN_POINT ( 'NONE',  ( 0.01548846960703768524, -0.5198120922912046193, 0.07362328916749273644 ) ) ;
#9833 = CARTESIAN_POINT ( 'NONE',  ( -0.01548846960707463312, 0.3772621329472714558, -0.3651003739303419482 ) ) ;
#9834 = PERSON_AND_ORGANIZATION_ROLE ( 'design_owner' ) ;
#9835 = EDGE_CURVE ( 'NONE', #13144, #23421, #35589, .T. ) ;
#9836 = CARTESIAN_POINT ( 'NONE',  ( 0.4765072543226545609, -1.073695880004174930, 0.6154142099768207252 ) ) ;
#9837 = CARTESIAN_POINT ( 'NONE',  ( -0.1731185243557762099, 0.5373335498847187086, 0.1000000000000000194 ) ) ;
#9838 = CARTESIAN_POINT ( 'NONE',  ( -0.2300000000000004818, 0.5182417262804733804, 0.3599999999999999867 ) ) ;
#9839 = DIRECTION ( 'NONE',  ( -0.4999999999999962808, 0.6386147891223726836, -0.5849539735006431540 ) ) ;
#9840 = PERSON ( 'NAUO-PER1', 'UNSPECIFIED', 'UNSPECIFIED', ('UNSPECIFIED'), ('UNSPECIFIED'), ('UNSPECIFIED') ) ;
#9841 =( BOUNDED_SURFACE ( )  B_SPLINE_SURFACE ( 3, 2, ( 
 ( #3477, #28581, #32063 ),
 ( #1044, #16422, #28963 ),
 ( #829, #13550, #454 ),
 ( #35355, #26121, #34543 ),
 ( #18923, #12950, #9843 ),
 ( #22412, #34943, #14543 ),
 ( #32454, #36147, #30186 ),
 ( #26718, #1233, #11262 ),
 ( #1625, #29995, #17038 ),
 ( #14147, #8170, #13731 ),
 ( #7342, #7565, #26505 ),
 ( #19919, #4279, #2016 ),
 ( #5079, #35538, #23832 ),
 ( #35958, #7767, #16847 ),
 ( #20333, #4872, #7957 ),
 ( #1828, #26907, #32855 ),
 ( #29387, #32666, #27108 ),
 ( #23443, #39247, #20750 ),
 ( #14344, #38823, #4658 ),
 ( #33065, #10451, #39439 ),
 ( #26298, #35751, #33273 ),
 ( #36353, #23018, #10655 ),
 ( #17639, #23227, #20139 ),
 ( #4470, #13934, #29577 ),
 ( #17233, #17443, #1419 ),
 ( #39037, #10870, #20531 ),
 ( #11068, #29784, #23630 ),
 ( #18251, #15155, #2818 ) ),
 .UNSPECIFIED., .F., .F., .T. ) 
 B_SPLINE_SURFACE_WITH_KNOTS ( ( 4, 2, 2, 2, 2, 2, 2, 2, 2, 2, 2, 2, 2, 4 ),
 ( 3, 3 ),
 ( 0.008694144295605974598, 0.009671288477786803284, 0.01015986056887721936, 0.01064843265996763370, 0.01113700475105804805, 0.01162557684214846412, 0.01211414893323887847, 0.01260272102432929281, 0.01309129311541970715, 0.01357986520651012149, 0.01406843729760053757, 0.01455700938869095191, 0.01553415357087178233, 0.01651129775305261102 ),
 ( 0.000000000000000000, 1.000000000000000000 ),
 .UNSPECIFIED. ) 
 GEOMETRIC_REPRESENTATION_ITEM ( )  RATIONAL_B_SPLINE_SURFACE ( (
 ( 1.000000000000000000, 0.6470169433091488287, 1.000000000000000000),
 ( 1.000000000000000000, 0.6654672097952949450, 1.000000000000000000),
 ( 1.000000000000000000, 0.6852032907093373870, 1.000000000000000000),
 ( 1.000000000000000000, 0.7106118140251836968, 1.000000000000000000),
 ( 1.000000000000000000, 0.7184497985660520669, 1.000000000000000000),
 ( 1.000000000000000000, 0.7321196217632601755, 1.000000000000000000),
 ( 1.000000000000000000, 0.7378276987527578878, 1.000000000000000000),
 ( 1.000000000000000000, 0.7460113087339939053, 1.000000000000000000),
 ( 1.000000000000000000, 0.7485381724456307007, 1.000000000000000000),
 ( 1.000000000000000000, 0.7496653861197896118, 1.000000000000000000),
 ( 1.000000000000000000, 0.7481474087358157554, 1.000000000000000000),
 ( 1.000000000000000000, 0.7416790020604431266, 1.000000000000000000),
 ( 1.000000000000000000, 0.7366135046999445768, 1.000000000000000000),
 ( 1.000000000000000000, 0.7274392094783487250, 1.000000000000000000),
 ( 1.000000000000000000, 0.7238593899674543586, 1.000000000000000000),
 ( 1.000000000000000000, 0.7238140619247546148, 1.000000000000000000),
 ( 1.000000000000000000, 0.7273137035903693981, 1.000000000000000000),
 ( 1.000000000000000000, 0.7363604236068268527, 1.000000000000000000),
 ( 1.000000000000000000, 0.7415226458536995358, 1.000000000000000000),
 ( 1.000000000000000000, 0.7480748423670980918, 1.000000000000000000),
 ( 1.000000000000000000, 0.7496261409616462590, 1.000000000000000000),
 ( 1.000000000000000000, 0.7486302821632393467, 1.000000000000000000),
 ( 1.000000000000000000, 0.7461034829534261004, 1.000000000000000000),
 ( 1.000000000000000000, 0.7338444141171208690, 1.000000000000000000),
 ( 1.000000000000000000, 0.7192226083161986638, 1.000000000000000000),
 ( 1.000000000000000000, 0.6852364196241883532, 1.000000000000000000),
 ( 1.000000000000000000, 0.6655055671846430432, 1.000000000000000000),
 ( 1.000000000000000000, 0.6469660273759296754, 1.000000000000000000) ) ) 
 REPRESENTATION_ITEM ( '' )  SURFACE ( )  );
#9842 = CARTESIAN_POINT ( 'NONE',  ( -0.001733054258001554731, -0.9004704535694999512, 0.2409329515054920989 ) ) ;
#9843 = CARTESIAN_POINT ( 'NONE',  ( 0.5825939818895130573, -1.511660705017517037, -0.4462983586487643817 ) ) ;
#9844 = CARTESIAN_POINT ( 'NONE',  ( 0.4268980379306122064, -1.643599345667950962, -0.4092648393969009479 ) ) ;
#9845 = CARTESIAN_POINT ( 'NONE',  ( 0.2798936374030868146, -1.205716238392265938, 0.4282426334535158197 ) ) ;
#9846 = ORIENTED_EDGE ( 'NONE', *, *, #19209, .T. ) ;
#9847 = ORIENTED_EDGE ( 'NONE', *, *, #16933, .T. ) ;
#9848 = CARTESIAN_POINT ( 'NONE',  ( 0.03654364704248821982, -0.2290829176602880712, -0.4574690890339243587 ) ) ;
#9849 = ORIENTED_EDGE ( 'NONE', *, *, #19596, .T. ) ;
#9850 = DIRECTION ( 'NONE',  ( 1.000000000000000000, 0.000000000000000000, 0.000000000000000000 ) ) ;
#9851 = CARTESIAN_POINT ( 'NONE',  ( -0.02000000000000000042, -2.177105168660885326, -0.2518349584362399862 ) ) ;
#9852 = FACE_OUTER_BOUND ( 'NONE', #35185, .T. ) ;
#9853 = AXIS2_PLACEMENT_3D ( 'NONE', #27983, #6552, #25309 ) ;
#9855 = EDGE_LOOP ( 'NONE', ( #22381, #13529, #8233 ) ) ;
#9854 = FACE_OUTER_BOUND ( 'NONE', #3492, .T. ) ;
#9856 = EDGE_LOOP ( 'NONE', ( #40091, #27230, #3657, #27388 ) ) ;
#9857 = CARTESIAN_POINT ( 'NONE',  ( -0.02000000000000000042, -2.263760933879813919, -0.5090783786781539755 ) ) ;
#9858 = ORIENTED_EDGE ( 'NONE', *, *, #36821, .F. ) ;
#9859 = AXIS2_PLACEMENT_3D ( 'NONE', #39295, #26561, #36005 ) ;
#9860 = CARTESIAN_POINT ( 'NONE',  ( 0.01082649148626377289, -0.5336901187179717843, 0.1852521559336037515 ) ) ;
#9862 = CARTESIAN_POINT ( 'NONE',  ( 0.1984280195443378358, -1.270055564915130608, -0.3194734774171836822 ) ) ;
#9861 = DIRECTION ( 'NONE',  ( 0.9998941247116546194, -0.01455087607601020239, 0.0001066420868422379362 ) ) ;
#9863 = CARTESIAN_POINT ( 'NONE',  ( 0.3187641638634979291, -1.760284878867078184, 0.5597302103697513465 ) ) ;
#9864 = CARTESIAN_POINT ( 'NONE',  ( -2.696301922142130194E-33, -2.357338251929976383E-33, 0.06250000000000000000 ) ) ;
#9865 = CARTESIAN_POINT ( 'NONE',  ( 0.4173132459375102354, -1.699444977922911493, 0.4182417262808778013 ) ) ;
#9867 = EDGE_LOOP ( 'NONE', ( #21690, #37799, #22902, #35009 ) ) ;
#9866 = ORIENTED_EDGE ( 'NONE', *, *, #32275, .T. ) ;
#9868 = CARTESIAN_POINT ( 'NONE',  ( 0.3897459579033060728, -1.931687273480471312, -0.4920516470159677080 ) ) ;
#9869 = CARTESIAN_POINT ( 'NONE',  ( 0.2267725030444622258, -0.9370487796004768333, 0.4246761745800142762 ) ) ;
#9870 = CARTESIAN_POINT ( 'NONE',  ( -0.02869942827333608198, 0.06034320897027863062, -0.4947801815387833924 ) ) ;
#9871 = CARTESIAN_POINT ( 'NONE',  ( 0.5903457776621824360, -1.446032249997192265, 0.6697935441370801435 ) ) ;
#9872 = FACE_OUTER_BOUND ( 'NONE', #26427, .T. ) ;
#9873 = CARTESIAN_POINT ( 'NONE',  ( 0.03743290345340095221, -0.7527584146679924260, 0.6138086348110104451 ) ) ;
#9874 = CARTESIAN_POINT ( 'NONE',  ( 0.4811037392677499636, -1.175372539374476277, 0.4182417262808778013 ) ) ;
#9875 = CARTESIAN_POINT ( 'NONE',  ( 0.001519927481451859626, -0.8472461526284917888, 0.1457185332388711008 ) ) ;
#9876 = FACE_OUTER_BOUND ( 'NONE', #3146, .T. ) ;
#9877 = FACE_OUTER_BOUND ( 'NONE', #4486, .T. ) ;
#9878 = DIRECTION ( 'NONE',  ( 0.000000000000000000, 0.000000000000000000, -1.000000000000000000 ) ) ;
#9879 = CARTESIAN_POINT ( 'NONE',  ( -0.1700000000000000400, 6.829619984160658046E-17, 2.048885995248197414E-16 ) ) ;
#9880 = AXIS2_PLACEMENT_3D ( 'NONE', #26677, #16587, #39211 ) ;
#9881 = B_SPLINE_CURVE_WITH_KNOTS ( 'NONE', 3,
 ( #31754, #3574, #3360, #16742, #29070, #19014, #16142, #35442 ),
 .UNSPECIFIED., .F., .F.,
 ( 4, 2, 2, 4 ),
 ( 2.350980519117237965E-07, 0.001838925622864737370, 0.002758270885271150389, 0.003677616147677563625 ),
 .UNSPECIFIED. ) ;
#9882 = CARTESIAN_POINT ( 'NONE',  ( -0.0004424791507732630863, -0.9367167129038177498, 0.1813186842804689336 ) ) ;
#9883 = EDGE_CURVE ( 'NONE', #14004, #4299, #26788, .T. ) ;
#9884 = CARTESIAN_POINT ( 'NONE',  ( 0.3165986513250982903, -1.745708308064116920, 0.7545403346239585307 ) ) ;
#9885 = CARTESIAN_POINT ( 'NONE',  ( 0.1988350626189778203, -1.655126656547283082, -0.6577951576610993056 ) ) ;
#9886 = ADVANCED_FACE ( 'NONE', ( #11335 ), #8039, .T. ) ;
#9887 = COORDINATED_UNIVERSAL_TIME_OFFSET ( 0, 0, .AHEAD. ) ;
#9888 = CIRCLE ( 'NONE', #21731, 0.09999999999999999167 ) ;
#9889 = CARTESIAN_POINT ( 'NONE',  ( 0.3716760655518760448, -1.720866715815103420, -0.6853003695678743235 ) ) ;
#9891 = ADVANCED_FACE ( 'NONE', ( #9678 ), #18754, .T. ) ;
#9890 = AXIS2_PLACEMENT_3D ( 'NONE', #3550, #34412, #31521 ) ;
#9892 = CARTESIAN_POINT ( 'NONE',  ( -0.04285427992854486112, 0.4878399728613377340, 0.08281491827193812605 ) ) ;
#9893 = CARTESIAN_POINT ( 'NONE',  ( -0.3000000000000000999, -3.527715956914472706, -0.3920205355121876289 ) ) ;
#9894 = EDGE_CURVE ( 'NONE', #25917, #30159, #263, .T. ) ;
#9895 = ORIENTED_EDGE ( 'NONE', *, *, #33780, .F. ) ;
#9896 = CARTESIAN_POINT ( 'NONE',  ( 0.1950037666476622522, -0.5640115203604925131, 0.3061966258278945863 ) ) ;
#9897 = ORIENTED_EDGE ( 'NONE', *, *, #10296, .F. ) ;
#9898 = CARTESIAN_POINT ( 'NONE',  ( 0.4555369797039701685, -1.145095616941093297, -0.3997359831693639842 ) ) ;
#9899 = CARTESIAN_POINT ( 'NONE',  ( 0.2664135068126231021, -1.673169779535225166, 0.5456938477760421291 ) ) ;
#9900 = CARTESIAN_POINT ( 'NONE',  ( 0.1341641613487604967, -0.5874067381197118909, 0.2837651016474003196 ) ) ;
#9902 = EDGE_LOOP ( 'NONE', ( #8957, #18781, #20359, #38008 ) ) ;
#9901 = CARTESIAN_POINT ( 'NONE',  ( -0.1743922129835737966, -0.5166151207188712791, 0.08499999999999977018 ) ) ;
#9903 = VECTOR ( 'NONE', #11606, 39.37007874015748854 ) ;
#9905 = ORIENTED_EDGE ( 'NONE', *, *, #21991, .T. ) ;
#9904 = ORIENTED_EDGE ( 'NONE', *, *, #3338, .T. ) ;
#9906 = CARTESIAN_POINT ( 'NONE',  ( 0.6623042051160524801, -1.539866302937538789, 0.7062118603361370317 ) ) ;
#9907 = ORIENTED_EDGE ( 'NONE', *, *, #18860, .T. ) ;
#9908 = EDGE_CURVE ( 'NONE', #37075, #9543, #31655, .T. ) ;
#9909 = PRODUCT_RELATED_PRODUCT_CATEGORY ( 'detail', '', ( #27234 ) ) ;
#9910 = CARTESIAN_POINT ( 'NONE',  ( -0.1696282724551476662, 0.4941130859153646249, 0.1349535128744427936 ) ) ;
#9911 = CARTESIAN_POINT ( 'NONE',  ( 0.5455881031540378290, -1.595019605959082654, -0.5473203437262895710 ) ) ;
#9912 = VERTEX_POINT ( 'NONE', #30866 ) ;
#9913 = CARTESIAN_POINT ( 'NONE',  ( 0.08963489136116924161, -0.7509102906732701976, 0.2481878857498304447 ) ) ;
#9914 = CARTESIAN_POINT ( 'NONE',  ( 0.08990536851188021816, -0.5646295468556834507, 0.1408780685345830397 ) ) ;
#9915 = AXIS2_PLACEMENT_3D ( 'NONE', #39649, #5086, #17646 ) ;
#9916 = CARTESIAN_POINT ( 'NONE',  ( 0.1114640335818673916, -0.5707303086454891261, 0.2491850945404860684 ) ) ;
#9917 = LINE ( 'NONE', #9723, #106 ) ;
#9918 = CARTESIAN_POINT ( 'NONE',  ( -0.1659602879904968076, 0.5155992160893295706, 0.1238948718127820675 ) ) ;
#9919 = AXIS2_PLACEMENT_3D ( 'NONE', #11076, #23636, #36155 ) ;
#9920 = CARTESIAN_POINT ( 'NONE',  ( 0.7207144797668179059, -1.477263269554723202, 0.5687618070419677707 ) ) ;
#9921 = ORIENTED_EDGE ( 'NONE', *, *, #33885, .T. ) ;
#9922 = TOROIDAL_SURFACE ( 'NONE', #23104, 0.5250000000000000222, 0.01499999999999999944 ) ;
#9923 = CARTESIAN_POINT ( 'NONE',  ( 0.3164126684801325529, -1.761786144345217187, 0.5684815686975395188 ) ) ;
#9924 = CARTESIAN_POINT ( 'NONE',  ( 0.6757026422043570513, -1.393510729029532547, 0.7334196951842761880 ) ) ;
#9925 = EDGE_CURVE ( 'NONE', #17309, #36373, #36902, .T. ) ;
#9926 = CARTESIAN_POINT ( 'NONE',  ( 0.5654596793231598806, -1.618818539163461301, 0.5682417262808788783 ) ) ;
#9927 = CARTESIAN_POINT ( 'NONE',  ( 0.1349510429637978681, -0.5701812554335998762, 0.2338515878604368881 ) ) ;
#9928 = DIRECTION ( 'NONE',  ( 1.000000000000000000, 0.000000000000000000, 0.000000000000000000 ) ) ;
#9929 = LENGTH_MEASURE_WITH_UNIT ( LENGTH_MEASURE( 0.02539999999999999897 ), #21282 );
#9930 = CARTESIAN_POINT ( 'NONE',  ( 0.3207148961678939481, -1.182401600646133089, 0.3667417262808778111 ) ) ;
#9931 = CARTESIAN_POINT ( 'NONE',  ( -0.02000000000000000042, -1.646519645934556131, -0.1171471737359304072 ) ) ;
#9932 = LINE ( 'NONE', #6838, #15262 ) ;
#9933 = CARTESIAN_POINT ( 'NONE',  ( 0.4975638555224211612, -1.097967759515461550, 0.6244301767862630026 ) ) ;
#9934 = EDGE_CURVE ( 'NONE', #36123, #25560, #28605, .T. ) ;
#9935 = DATE_TIME_ROLE ( 'classification_date' ) ;
#9936 = DIRECTION ( 'NONE',  ( -8.881784197001246407E-16, 2.361472542561082612E-16, -1.000000000000000000 ) ) ;
#9937 = ADVANCED_FACE ( 'NONE', ( #21827 ), #25843, .T. ) ;
#9938 = AXIS2_PLACEMENT_3D ( 'NONE', #18065, #30616, #2443 ) ;
#9939 = CARTESIAN_POINT ( 'NONE',  ( 0.6054889487767985967, -1.479703267939684874, 0.5856070495615782745 ) ) ;
#9940 = AXIS2_PLACEMENT_3D ( 'NONE', #39886, #2253, #5296 ) ;
#9941 = EDGE_CURVE ( 'NONE', #2835, #1749, #24436, .T. ) ;
#9942 = CARTESIAN_POINT ( 'NONE',  ( -0.04047161733259035249, 0.06271464429810597041, 0.4973245071804685558 ) ) ;
#9943 = CONICAL_SURFACE ( 'NONE', #4033, 0.1600000000000005029, 1.047197551196598742 ) ;
#9944 = VERTEX_POINT ( 'NONE', #40324 ) ;
#9945 = DIRECTION ( 'NONE',  ( 0.000000000000000000, -0.5877852522925116618, -0.8090169943749194736 ) ) ;
#9946 = CIRCLE ( 'NONE', #27610, 0.02999999999999999195 ) ;
#9947 = CARTESIAN_POINT ( 'NONE',  ( 0.002938675265522861478, -0.5479465208063443171, 0.2683199588513891509 ) ) ;
#9948 = AXIS2_PLACEMENT_3D ( 'NONE', #34394, #37683, #12798 ) ;
#9949 = PLANE ( 'NONE',  #9475 ) ;
#9950 = ORIENTED_EDGE ( 'NONE', *, *, #14984, .F. ) ;
#9951 = CARTESIAN_POINT ( 'NONE',  ( 0.4094665197507286747, -1.132124008075320098, 0.5707417262808780478 ) ) ;
#9952 = CARTESIAN_POINT ( 'NONE',  ( 0.002782022538515906661, -0.9412645402768823333, 0.6116066270186392151 ) ) ;
#9954 = ORIENTED_EDGE ( 'NONE', *, *, #36038, .F. ) ;
#9953 = EDGE_LOOP ( 'NONE', ( #22124, #17761, #3971, #1684 ) ) ;
#9955 = CARTESIAN_POINT ( 'NONE',  ( -0.02000000000000000042, -2.626773565144302935, -0.2726934094652516127 ) ) ;
#9956 = ORIENTED_EDGE ( 'NONE', *, *, #12398, .F. ) ;
#9957 = CARTESIAN_POINT ( 'NONE',  ( -2.070754768975505034, -0.09959325338431362917, 0.09550516381870004234 ) ) ;
#9958 = EDGE_CURVE ( 'NONE', #33739, #23391, #21415, .T. ) ;
#9959 = DIRECTION ( 'NONE',  ( 1.000000000000000000, 0.000000000000000000, 0.000000000000000000 ) ) ;
#9960 = DIRECTION ( 'NONE',  ( 0.9378410757839558132, -0.3470650033817763158, 0.000000000000000000 ) ) ;
#9961 = B_SPLINE_CURVE_WITH_KNOTS ( 'NONE', 3,
 ( #33865, #30367, #24399, #27684 ),
 .UNSPECIFIED., .F., .F.,
 ( 4, 4 ),
 ( 0.000000000000000000, 0.0002238335178989935437 ),
 .UNSPECIFIED. ) ;
#9962 = FACE_OUTER_BOUND ( 'NONE', #9855, .T. ) ;
#9963 = ORIENTED_EDGE ( 'NONE', *, *, #19848, .T. ) ;
#9964 = CARTESIAN_POINT ( 'NONE',  ( 0.2486235419350810716, -1.344789659884683797, 1.171751475820631105 ) ) ;
#9965 = ORIENTED_EDGE ( 'NONE', *, *, #21741, .T. ) ;
#9966 = ORIENTED_EDGE ( 'NONE', *, *, #26247, .T. ) ;
#9967 = CARTESIAN_POINT ( 'NONE',  ( 0.09572618302809746127, -0.6249641250925348501, 0.2872090638444997901 ) ) ;
#9968 = B_SPLINE_CURVE_WITH_KNOTS ( 'NONE', 3,
 ( #11351, #5166, #8263, #36238, #8051, #39737, #8460, #15052, #20630, #17327 ),
 .UNSPECIFIED., .F., .F.,
 ( 4, 3, 3, 4 ),
 ( 0.000000000000000000, 4.304601007142825036E-05, 8.690714465717732273E-05, 0.0001096645486937237969 ),
 .UNSPECIFIED. ) ;
#9969 = CARTESIAN_POINT ( 'NONE',  ( 0.02524471160769579600, -0.6279797553945640765, 0.5994203574518347510 ) ) ;
#9970 = CARTESIAN_POINT ( 'NONE',  ( 0.4456035407152363348, -1.502374677390132529, 0.7781194087335665532 ) ) ;
#9972 = CARTESIAN_POINT ( 'NONE',  ( -0.1196127869351431838, -0.4993621520964605653, 0.3258261256381336235 ) ) ;
#9971 = CARTESIAN_POINT ( 'NONE',  ( 0.04598863217031589484, -0.8257334846043561383, 0.7092904895903023865 ) ) ;
#9973 = CARTESIAN_POINT ( 'NONE',  ( 0.01227139476065501611, -0.8747808039168644134, 0.4454182558007432347 ) ) ;
#9974 = CARTESIAN_POINT ( 'NONE',  ( 0.1718750000000003053, -0.9178826446108661052, 0.1457185332388701848 ) ) ;
#9975 = CIRCLE ( 'NONE', #36895, 0.01499999999999994914 ) ;
#9976 = UNCERTAINTY_MEASURE_WITH_UNIT (LENGTH_MEASURE( 1.000000000000000082E-05 ), #33549, 'distance_accuracy_value', 'NONE');
#9977 = LINE ( 'NONE', #153, #33773 ) ;
#9978 = CARTESIAN_POINT ( 'NONE',  ( 0.4409062655693435917, -1.690090444797295532, -0.4991292961807995421 ) ) ;
#9979 = CARTESIAN_POINT ( 'NONE',  ( -0.04085667396267339546, 0.2941474082995404471, -0.3688418229621439060 ) ) ;
#9980 = AXIS2_PLACEMENT_3D ( 'NONE', #20610, #11940, #36824 ) ;
#9981 = AXIS2_PLACEMENT_3D ( 'NONE', #7891, #23161, #13862 ) ;
#9982 = DIRECTION ( 'NONE',  ( 1.000000000000000000, -0.000000000000000000, -0.000000000000000000 ) ) ;
#9983 = CIRCLE ( 'NONE', #21801, 0.03000000000000000583 ) ;
#9984 = DIRECTION ( 'NONE',  ( 0.8660512985181136880, 0.4999551463232367876, 0.000000000000000000 ) ) ;
#9985 = CARTESIAN_POINT ( 'NONE',  ( 0.3136035985995381248, -0.8251737266935038617, 0.6634070228338775355 ) ) ;
#9986 = EDGE_CURVE ( 'NONE', #20774, #16986, #20499, .T. ) ;
#9987 = CARTESIAN_POINT ( 'NONE',  ( 0.4839838468137014904, -1.192129550890687062, 0.4021087476649028991 ) ) ;
#9988 = CARTESIAN_POINT ( 'NONE',  ( 0.04078634645975903056, -1.210087468311284553, 0.6658561005973028246 ) ) ;
#9989 = EDGE_CURVE ( 'NONE', #39766, #31435, #25940, .T. ) ;
#9991 = AXIS2_PLACEMENT_3D ( 'NONE', #8962, #37150, #21535 ) ;
#9990 = CARTESIAN_POINT ( 'NONE',  ( 0.03672447062657550193, 0.4430265621404723686, -0.1868507191434661263 ) ) ;
#9992 = LINE ( 'NONE', #31406, #5477 ) ;
#9993 = CARTESIAN_POINT ( 'NONE',  ( 0.2939503495491210816, -1.005253864439647371, 0.7192296934484712079 ) ) ;
#9994 = FACE_OUTER_BOUND ( 'NONE', #6656, .T. ) ;
#9995 = CARTESIAN_POINT ( 'NONE',  ( 0.1759300380180282841, -1.231083256582695906, -0.6184399470714002645 ) ) ;
#9996 = VERTEX_POINT ( 'NONE', #13577 ) ;
#9997 = DIRECTION ( 'NONE',  ( 0.000000000000000000, 0.000000000000000000, -1.000000000000000000 ) ) ;
#9998 = CARTESIAN_POINT ( 'NONE',  ( 0.3879614285305876820, -1.650392248945780960, -0.3945637954816432202 ) ) ;
#9999 = CIRCLE ( 'NONE', #18546, 0.1000000000000000194 ) ;
#10000 = CARTESIAN_POINT ( 'NONE',  ( 0.06444297064315794576, -0.8352831487901670737, 0.1457185332388703236 ) ) ;
#10001 = CARTESIAN_POINT ( 'NONE',  ( 0.08609945990018005868, -1.325383490889678662, 0.4606874596949692147 ) ) ;
#10002 = ORIENTED_EDGE ( 'NONE', *, *, #1714, .F. ) ;
#10003 = CARTESIAN_POINT ( 'NONE',  ( -0.1699622337672979377, 0.4951791062278196320, 0.3187362200132128343 ) ) ;
#10004 = AXIS2_PLACEMENT_3D ( 'NONE', #25993, #39131, #39322 ) ;
#10005 = CIRCLE ( 'NONE', #39568, 0.6114999999999938263 ) ;
#10006 = ADVANCED_FACE ( 'NONE', ( #26529 ), #12988, .T. ) ;
#10007 = CARTESIAN_POINT ( 'NONE',  ( 0.1818182084070924798, -0.5169919523671798745, 0.2198248585042891778 ) ) ;
#10008 = CARTESIAN_POINT ( 'NONE',  ( -0.1443922129835726875, -0.5166151207188712791, 0.3750000000000001110 ) ) ;
#10009 = ADVANCED_FACE ( 'NONE', ( #20560, #33093 ), #28103, .T. ) ;
#10010 = CARTESIAN_POINT ( 'NONE',  ( 0.05999999999999990757, 0.000000000000000000, 0.000000000000000000 ) ) ;
#10011 = AXIS2_PLACEMENT_3D ( 'NONE', #6451, #19022, #30950 ) ;
#10012 = CARTESIAN_POINT ( 'NONE',  ( 0.4433349170228174652, -1.204176679204282729, 0.6897527930916858008 ) ) ;
#10013 = LINE ( 'NONE', #6916, #19369 ) ;
#10014 = CARTESIAN_POINT ( 'NONE',  ( 0.4862843069642890925, -1.079060212656593798, 0.6007065101366493298 ) ) ;
#10015 = ORIENTED_EDGE ( 'NONE', *, *, #28089, .T. ) ;
#10016 = EDGE_CURVE ( 'NONE', #19872, #357, #24614, .T. ) ;
#10017 = DATE_AND_TIME ( #37997, #6950 ) ;
#10018 = CARTESIAN_POINT ( 'NONE',  ( 0.007861457232516730342, -0.8999816549950413469, 0.5065308129498107270 ) ) ;
#10019 = ORIENTED_EDGE ( 'NONE', *, *, #15014, .T. ) ;
#10020 = ADVANCED_FACE ( 'NONE', ( #1653 ), #17260, .T. ) ;
#10021 = CARTESIAN_POINT ( 'NONE',  ( 0.3845294810406492680, -1.605350533059137108, 0.5636378812280004036 ) ) ;
#10023 = CARTESIAN_POINT ( 'NONE',  ( 0.1940093581540119627, -0.6292132035201315476, 0.3231077534996323886 ) ) ;
#10022 = CARTESIAN_POINT ( 'NONE',  ( 0.06448134467046603979, -0.8354324776869207492, 0.1387861693055511825 ) ) ;
#10024 = CARTESIAN_POINT ( 'NONE',  ( 0.000000000000000000, 0.7171888913565960255, -0.2950238883388468514 ) ) ;
#10025 = VERTEX_POINT ( 'NONE', #37151 ) ;
#10026 = ORIENTED_EDGE ( 'NONE', *, *, #10262, .T. ) ;
#10027 = DIRECTION ( 'NONE',  ( 0.000000000000000000, 0.000000000000000000, 1.000000000000000000 ) ) ;
#10028 = CARTESIAN_POINT ( 'NONE',  ( 0.5500379755161437512, -1.473456634498119699, 0.7231298284428128165 ) ) ;
#10029 = ORIENTED_EDGE ( 'NONE', *, *, #6965, .T. ) ;
#10030 = CARTESIAN_POINT ( 'NONE',  ( 0.3868395167223153130, -1.896608414150803501, -0.5100822255063985899 ) ) ;
#10031 = DIRECTION ( 'NONE',  ( 1.000000000000000000, -0.000000000000000000, -0.000000000000000000 ) ) ;
#10032 = LINE ( 'NONE', #25272, #22355 ) ;
#10033 = CARTESIAN_POINT ( 'NONE',  ( -1.019575837292303166, -0.04310840302197994911, 0.09999999999999879818 ) ) ;
#10034 = CARTESIAN_POINT ( 'NONE',  ( 0.08556124454896821274, -1.317821213116421308, 0.4727606578195797660 ) ) ;
#10035 = VECTOR ( 'NONE', #4364, 39.37007874015748143 ) ;
#10036 = CARTESIAN_POINT ( 'NONE',  ( 0.02746053214171286644, -1.399542977676857758, -0.3784122419456570907 ) ) ;
#10037 = CARTESIAN_POINT ( 'NONE',  ( 0.3757471142192216340, -1.766731021160330206, -0.5680748514784758063 ) ) ;
#10038 = CARTESIAN_POINT ( 'NONE',  ( 0.7255563027409094312, -1.477976514587821422, 0.7347025679090390948 ) ) ;
#10039 = AXIS2_PLACEMENT_3D ( 'NONE', #13329, #25902, #38420 ) ;
#10040 = VECTOR ( 'NONE', #3815, 39.37007874015748143 ) ;
#10041 = LINE ( 'NONE', #32655, #4979 ) ;
#10042 = CARTESIAN_POINT ( 'NONE',  ( 0.1157337385916143990, -1.413492129114879203, 0.5950113313978990792 ) ) ;
#10043 = PERSON_AND_ORGANIZATION_ROLE ( 'classification_officer' ) ;
#10044 = AXIS2_PLACEMENT_3D ( 'NONE', #39265, #5095, #23648 ) ;
#10045 = ADVANCED_FACE ( 'NONE', ( #8963 ), #8760, .F. ) ;
#10046 = CARTESIAN_POINT ( 'NONE',  ( 0.4159916692016358830, -1.069406866067976081, -0.5155029497116575543 ) ) ;
#10047 = DIRECTION ( 'NONE',  ( -1.000000000000000000, -0.000000000000000000, -0.000000000000000000 ) ) ;
#10048 = CARTESIAN_POINT ( 'NONE',  ( 0.7185393139234729221, -1.479621239843056157, 0.4933132820244564565 ) ) ;
#10049 = EDGE_CURVE ( 'NONE', #29582, #31816, #30968, .T. ) ;
#10050 = CARTESIAN_POINT ( 'NONE',  ( 0.4952488905928924545, -1.196841907270136174, 0.4182417262808778013 ) ) ;
#10051 = DIRECTION ( 'NONE',  ( -0.000000000000000000, 0.9215515678030125057, 0.3882559824134196313 ) ) ;
#10052 = CIRCLE ( 'NONE', #36320, 0.2149999999999999967 ) ;
#10053 = CARTESIAN_POINT ( 'NONE',  ( 0.02199361096923483153, -0.8343928545013460374, 0.5934276300867008525 ) ) ;
#10054 = CARTESIAN_POINT ( 'NONE',  ( 1.543663729362214677E-05, -0.6714880032592078773, -0.1033492426826144589 ) ) ;
#10055 = CARTESIAN_POINT ( 'NONE',  ( 0.4231587444657393116, -1.645334281830443945, -0.4089428064156527820 ) ) ;
#10056 = CARTESIAN_POINT ( 'NONE',  ( 0.2764337282391428618, -1.207704344519209938, -0.5166151207188711680 ) ) ;
#10057 = EDGE_LOOP ( 'NONE', ( #1843, #34604, #12025, #12430 ) ) ;
#10058 = ORIENTED_EDGE ( 'NONE', *, *, #13758, .T. ) ;
#10059 = FACE_OUTER_BOUND ( 'NONE', #21577, .T. ) ;
#10060 = EDGE_LOOP ( 'NONE', ( #16963, #31671, #36326, #11503, #35872, #33283 ) ) ;
#10061 = CARTESIAN_POINT ( 'NONE',  ( -0.02869942827333604035, -0.06034320897027634772, 0.4947801815387837809 ) ) ;
#10062 = DIRECTION ( 'NONE',  ( -0.8660512985181119117, -0.4999551463232398962, 0.000000000000000000 ) ) ;
#10063 = CIRCLE ( 'NONE', #33049, 0.03000000000000003011 ) ;
#10064 = CARTESIAN_POINT ( 'NONE',  ( 0.3297457498401996645, -1.032296429229499823, 0.7921737166615708814 ) ) ;
#10066 = ORIENTED_EDGE ( 'NONE', *, *, #495, .T. ) ;
#10065 = CARTESIAN_POINT ( 'NONE',  ( -0.2399999999999999079, -4.289222312108804225, -0.7308809693675260011 ) ) ;
#10067 = EDGE_LOOP ( 'NONE', ( #17297, #27015, #16823 ) ) ;
#10068 = DIRECTION ( 'NONE',  ( -0.9903960388894593736, -0.05258684961124808488, -0.1278683283695876416 ) ) ;
#10069 = AXIS2_PLACEMENT_3D ( 'NONE', #15622, #12333, #39898 ) ;
#10070 = EDGE_LOOP ( 'NONE', ( #15833, #19893, #9400, #39559 ) ) ;
#10071 = AXIS2_PLACEMENT_3D ( 'NONE', #15579, #28523, #9386 ) ;
#10072 = CARTESIAN_POINT ( 'NONE',  ( 0.2962541062570004380, -1.656293626468827274, 0.5607359955346605807 ) ) ;
#10074 = CARTESIAN_POINT ( 'NONE',  ( -0.03868649100028027227, -0.4417196792138980421, 0.1788567627196056276 ) ) ;
#10073 = CARTESIAN_POINT ( 'NONE',  ( 0.6560486628413821908, -1.555476615240107829, 0.4279073640907943843 ) ) ;
#10075 = DIRECTION ( 'NONE',  ( 1.000000000000000000, -0.000000000000000000, -0.000000000000000000 ) ) ;
#10076 = CARTESIAN_POINT ( 'NONE',  ( 0.01185910703655305813, -0.5726836470825711345, -0.08659834197632501618 ) ) ;
#10077 = CARTESIAN_POINT ( 'NONE',  ( 0.04088380661261944299, -1.519926711703535327, -0.3733014666261871839 ) ) ;
#10079 = ORIENTED_EDGE ( 'NONE', *, *, #23983, .T. ) ;
#10078 = VERTEX_POINT ( 'NONE', #27898 ) ;
#10080 = DIRECTION ( 'NONE',  ( 0.000000000000000000, -0.7185945389471800615, -0.6954292836768448671 ) ) ;
#10081 = CARTESIAN_POINT ( 'NONE',  ( 0.1862146387795068081, -0.9153544180079368209, 0.1468049697877028548 ) ) ;
#10082 = AXIS2_PLACEMENT_3D ( 'NONE', #22457, #22262, #34983 ) ;
#10083 = CARTESIAN_POINT ( 'NONE',  ( -0.02953079040095533611, -0.4684706630666171101, 0.2484463060367359533 ) ) ;
#10084 = CARTESIAN_POINT ( 'NONE',  ( 0.6080545645982834424, -1.479187156349330623, 0.6099109919555032455 ) ) ;
#10085 = CIRCLE ( 'NONE', #271, 0.03000000000000002318 ) ;
#10086 = CARTESIAN_POINT ( 'NONE',  ( 0.2434517139947088293, -1.036255305955214867, 0.7293849779716305992 ) ) ;
#10087 = FACE_OUTER_BOUND ( 'NONE', #9656, .T. ) ;
#10088 = DIRECTION ( 'NONE',  ( -6.162975822039154730E-33, 0.000000000000000000, -1.000000000000000000 ) ) ;
#10089 = CARTESIAN_POINT ( 'NONE',  ( -0.1603938765018590729, 0.4636889572247935298, 0.3382895567580809226 ) ) ;
#10090 = CARTESIAN_POINT ( 'NONE',  ( 0.1499999999999993561, -3.685538980774209949E-17, -0.1750000000000000167 ) ) ;
#10091 =( BOUNDED_SURFACE ( )  B_SPLINE_SURFACE ( 3, 2, ( 
 ( #39861, #11680, #39646 ),
 ( #8787, #36574, #17837 ),
 ( #27521, #1634, #14349 ),
 ( #39444, #30398, #23838 ),
 ( #2230, #24435, #21363 ),
 ( #5700, #14768, #27331 ) ),
 .UNSPECIFIED., .F., .F., .F. ) 
 B_SPLINE_SURFACE_WITH_KNOTS ( ( 4, 2, 4 ),
 ( 3, 3 ),
 ( 6.179952383167375274E-18, 0.0007344380730649742277, 0.001468876146129942384 ),
 ( 0.000000000000000000, 1.000000000000000000 ),
 .UNSPECIFIED. ) 
 GEOMETRIC_REPRESENTATION_ITEM ( )  RATIONAL_B_SPLINE_SURFACE ( (
 ( 1.000000000000000000, 0.8219793159978235897, 1.000000000000000000),
 ( 1.000000000000000000, 0.8695169202949041276, 1.000000000000000000),
 ( 1.000000000000000000, 0.9157158777252236703, 1.000000000000000000),
 ( 1.000000000000000000, 0.9814457743411639790, 1.000000000000000000),
 ( 1.000000000000000000, 1.000262163779328528, 1.000000000000000000),
 ( 1.000000000000000000, 1.000000000000000000, 1.000000000000000000) ) ) 
 REPRESENTATION_ITEM ( '' )  SURFACE ( )  );
#10092 = CARTESIAN_POINT ( 'NONE',  ( -0.01548846960688927792, 0.5198120922917062181, -0.07362328916747552798 ) ) ;
#10093 = DIRECTION ( 'NONE',  ( 0.000000000000000000, 0.000000000000000000, -1.000000000000000000 ) ) ;
#10094 = DIRECTION ( 'NONE',  ( -0.7889715560959240648, -0.4554584589247170356, 0.4124093547259785053 ) ) ;
#10095 = AXIS2_PLACEMENT_3D ( 'NONE', #9851, #5944, #38039 ) ;
#10096 = CARTESIAN_POINT ( 'NONE',  ( 0.02953079040094797741, -0.3810518745594024259, 0.3687679460475924431 ) ) ;
#10097 = CARTESIAN_POINT ( 'NONE',  ( 0.3149693831142335032, -1.765269515322325899, 0.6420921437412323574 ) ) ;
#10098 = CARTESIAN_POINT ( 'NONE',  ( 0.1115667700604296847, -1.368744839739478580, 0.6778201501234852877 ) ) ;
#10099 = PERSON_AND_ORGANIZATION_ROLE ( 'classification_officer' ) ;
#10100 = CIRCLE ( 'NONE', #6150, 0.01000000000000002970 ) ;
#10101 = VECTOR ( 'NONE', #843, 39.37007874015748143 ) ;
#10102 = DIRECTION ( 'NONE',  ( -9.860761315262614725E-32, -0.9849933812516262766, 0.1725921171157263345 ) ) ;
#10103 = CARTESIAN_POINT ( 'NONE',  ( 0.3777603768608356338, -1.691903399793905027, -0.6926901660271995720 ) ) ;
#10104 = CARTESIAN_POINT ( 'NONE',  ( -0.04762035657659158955, 0.4700462218748341914, 0.1075639008184042372 ) ) ;
#10105 = DIRECTION ( 'NONE',  ( 0.000000000000000000, 0.7071067811865474617, 0.7071067811865474617 ) ) ;
#10106 = CIRCLE ( 'NONE', #8098, 0.01500000000000005322 ) ;
#10107 = CIRCLE ( 'NONE', #18653, 0.1400000000000003464 ) ;
#10108 = CARTESIAN_POINT ( 'NONE',  ( 5.439739711127286542E-16, -0.2981948553318921613, 0.06819284191469295042 ) ) ;
#10109 = VERTEX_POINT ( 'NONE', #12263 ) ;
#10110 = CARTESIAN_POINT ( 'NONE',  ( -0.2136509456379319383, -0.4946207598421927254, 0.3749999999999995559 ) ) ;
#10111 = CARTESIAN_POINT ( 'NONE',  ( 0.2621369394866731595, -1.686413516690222547, 0.5356639672823564347 ) ) ;
#10112 = CARTESIAN_POINT ( 'NONE',  ( 0.4883354474493797337, -1.330538578445629838, 0.8129148094954937731 ) ) ;
#10114 = EDGE_LOOP ( 'NONE', ( #15584, #28586, #16191, #10373, #2822, #29524, #10174, #29207, #34993 ) ) ;
#10113 = CARTESIAN_POINT ( 'NONE',  ( 0.5474085822752589037, -1.175693918439151942, 0.6018262437559286360 ) ) ;
#10116 = EDGE_LOOP ( 'NONE', ( #15547, #31172, #21426, #309, #25095 ) ) ;
#10115 = VERTEX_POINT ( 'NONE', #23653 ) ;
#10117 = DIRECTION ( 'NONE',  ( 0.000000000000000000, 0.000000000000000000, -1.000000000000000000 ) ) ;
#10118 = ORIENTED_EDGE ( 'NONE', *, *, #29774, .F. ) ;
#10119 = DIRECTION ( 'NONE',  ( 0.000000000000000000, -3.885780586188049371E-16, -1.000000000000000000 ) ) ;
#10120 = CARTESIAN_POINT ( 'NONE',  ( 0.6379677522609080720, -1.610970530618076380, -0.5598555352862202295 ) ) ;
#10121 = AXIS2_PLACEMENT_3D ( 'NONE', #12904, #29351, #23185 ) ;
#10122 = DIRECTION ( 'NONE',  ( 0.000000000000000000, 0.000000000000000000, -1.000000000000000000 ) ) ;
#10123 = ORIENTED_EDGE ( 'NONE', *, *, #13972, .T. ) ;
#10124 = CARTESIAN_POINT ( 'NONE',  ( 0.1716662052826025409, -0.8629998118152951703, 0.5713517472061939717 ) ) ;
#10125 = AXIS2_PLACEMENT_3D ( 'NONE', #5830, #18606, #31165 ) ;
#10126 = CARTESIAN_POINT ( 'NONE',  ( 0.08990536851188150880, -0.5646295468556827846, 0.1446695161202934954 ) ) ;
#10127 = AXIS2_PLACEMENT_3D ( 'NONE', #7731, #39600, #11435 ) ;
#10128 = CARTESIAN_POINT ( 'NONE',  ( 0.1101907795074059532, -0.5552708166754189989, 0.1999101508315398457 ) ) ;
#10129 = CARTESIAN_POINT ( 'NONE',  ( 0.6273212425429852690, -1.617116560689232152, -0.5218031926553677868 ) ) ;
#10130 = CARTESIAN_POINT ( 'NONE',  ( -0.06980746140711623082, 0.000000000000000000, 0.000000000000000000 ) ) ;
#10131 = APPROVAL_PERSON_ORGANIZATION ( #31749, #6886, #7050 ) ;
#10132 = FACE_OUTER_BOUND ( 'NONE', #12095, .T. ) ;
#10133 = EDGE_CURVE ( 'NONE', #24018, #38684, #18526, .T. ) ;
#10134 = CARTESIAN_POINT ( 'NONE',  ( 0.01548846960706735942, 0.4638115001431208362, 0.2459753896937896811 ) ) ;
#10135 = CARTESIAN_POINT ( 'NONE',  ( 0.7414302106162510286, -1.507121135501449771, 0.6614796144117841559 ) ) ;
#10136 = ADVANCED_FACE ( 'NONE', ( #30022 ), #36175, .T. ) ;
#10137 = AXIS2_PLACEMENT_3D ( 'NONE', #30994, #27924, #8781 ) ;
#10138 = CARTESIAN_POINT ( 'NONE',  ( 0.4631642984387073780, -1.593038035242256401, -0.6007335213492860371 ) ) ;
#10139 = CARTESIAN_POINT ( 'NONE',  ( 0.4435146130966207134, -1.231926360794060260, 0.8199172986756667614 ) ) ;
#10140 = TOROIDAL_SURFACE ( 'NONE', #23961, 0.08830708661417323302, 0.01499999999999999944 ) ;
#10141 = CARTESIAN_POINT ( 'NONE',  ( -1.882535413755627890E-05, -0.9357343916592213429, 0.06558131283649058785 ) ) ;
#10142 = DIRECTION ( 'NONE',  ( 1.000000000000000000, 2.341930812374887555E-31, -1.664003471950578127E-31 ) ) ;
#10143 = CARTESIAN_POINT ( 'NONE',  ( 0.4528109813659910721, -1.108023691146801548, -0.3699862881067115250 ) ) ;
#10144 = CARTESIAN_POINT ( 'NONE',  ( 1.365923996832131609E-16, -0.9481888444201345134, 0.1139263443108001761 ) ) ;
#10145 = CARTESIAN_POINT ( 'NONE',  ( 0.1897950977212392309, -0.7957416484119633759, 0.2611131357175326961 ) ) ;
#10146 = PERSON_AND_ORGANIZATION_ROLE ( 'creator' ) ;
#10147 = DIRECTION ( 'NONE',  ( 0.4999551463232372317, -0.8660512985181135770, 0.000000000000000000 ) ) ;
#10148 = EDGE_CURVE ( 'NONE', #1887, #1249, #4062, .T. ) ;
#10149 = APPLIED_DATE_AND_TIME_ASSIGNMENT ( #20844, #8056, ( #9542 ) ) ;
#10150 = AXIS2_PLACEMENT_3D ( 'NONE', #14105, #21098, #33430 ) ;
#10151 = AXIS2_PLACEMENT_3D ( 'NONE', #34256, #15133, #27497 ) ;
#10152 = LINE ( 'NONE', #22722, #20831 ) ;
#10153 = CARTESIAN_POINT ( 'NONE',  ( -0.03170752374382829891, -0.05433200130546726042, 0.4888275802721887553 ) ) ;
#10154 = VECTOR ( 'NONE', #28914, 39.37007874015748854 ) ;
#10155 = AXIS2_PLACEMENT_3D ( 'NONE', #17696, #30463, #1697 ) ;
#10156 = ORIENTED_EDGE ( 'NONE', *, *, #5244, .T. ) ;
#10157 = CARTESIAN_POINT ( 'NONE',  ( 0.4328515195334204368, -1.579414682775934109, 0.5917285476992683035 ) ) ;
#10158 = AXIS2_PLACEMENT_3D ( 'NONE', #29829, #38482, #32894 ) ;
#10159 = CARTESIAN_POINT ( 'NONE',  ( 0.01065772415598345742, -0.5389421826269154003, 0.2091342918453681088 ) ) ;
#10160 = DIRECTION ( 'NONE',  ( 0.000000000000000000, -0.8438867430782098777, -0.5365213554527457074 ) ) ;
#10161 = EDGE_LOOP ( 'NONE', ( #36264, #10185, #9904, #37774 ) ) ;
#10162 = DIRECTION ( 'NONE',  ( 1.000000000000000000, 6.779273404243070203E-32, 4.314083075427408311E-32 ) ) ;
#10163 = CIRCLE ( 'NONE', #28555, 1.991674066779348218 ) ;
#10164 = CARTESIAN_POINT ( 'NONE',  ( 0.6566606523871314494, -1.361328185136354119, 0.7219929986176217840 ) ) ;
#10166 = VERTEX_POINT ( 'NONE', #6063 ) ;
#10165 = ORIENTED_EDGE ( 'NONE', *, *, #19009, .T. ) ;
#10167 = CYLINDRICAL_SURFACE ( 'NONE', #35617, 0.01500000000000000291 ) ;
#10168 = EDGE_CURVE ( 'NONE', #22389, #16113, #11287, .T. ) ;
#10169 = VERTEX_POINT ( 'NONE', #13067 ) ;
#10170 = CARTESIAN_POINT ( 'NONE',  ( 0.3595150996541451871, -1.929818105082974800, -0.5025626374741613001 ) ) ;
#10171 = CARTESIAN_POINT ( 'NONE',  ( 0.2817715218429098223, -1.549959437726055933, -0.3415684628476097218 ) ) ;
#10172 = B_SPLINE_CURVE_WITH_KNOTS ( 'NONE', 3,
 ( #1086, #35594, #16287, #13173, #4111, #28825 ),
 .UNSPECIFIED., .F., .F.,
 ( 4, 2, 4 ),
 ( 2.453269466693398698E-18, 0.0006420322884310510243, 0.001284064576862099447 ),
 .UNSPECIFIED. ) ;
#10173 = CARTESIAN_POINT ( 'NONE',  ( 0.05268932808079675872, -0.2828369400135328227, -0.3737413977152367894 ) ) ;
#10174 = ORIENTED_EDGE ( 'NONE', *, *, #17544, .T. ) ;
#10175 = CARTESIAN_POINT ( 'NONE',  ( -2.086568639411206917E-17, -0.4716478265891163035, 0.3521378080009727185 ) ) ;
#10176 = ADVANCED_FACE ( 'NONE', ( #16553 ), #6877, .F. ) ;
#10177 = CARTESIAN_POINT ( 'NONE',  ( 0.1670460928285160684, -0.7847983796158649605, 0.5835955661026850372 ) ) ;
#10178 = ADVANCED_FACE ( 'NONE', ( #19246 ), #36287, .F. ) ;
#10179 = CARTESIAN_POINT ( 'NONE',  ( 0.01324987932754901482, -0.4603397457172120344, 0.2948093344987445241 ) ) ;
#10180 = CARTESIAN_POINT ( 'NONE',  ( 0.08793790621863624424, -0.5736368938888692925, 0.2699646086827657832 ) ) ;
#10182 = CARTESIAN_POINT ( 'NONE',  ( -0.1124400704934240963, -0.5139941482048617782, 0.3450122074418745521 ) ) ;
#10181 = CARTESIAN_POINT ( 'NONE',  ( 0.06517940379945762197, -0.9109053406753262472, 0.7832400949722142514 ) ) ;
#10183 = CARTESIAN_POINT ( 'NONE',  ( 0.1026215434209815508, -1.318872523977856259, 0.7205090641466329604 ) ) ;
#10184 = CARTESIAN_POINT ( 'NONE',  ( 0.4548150350199454128, -1.105354657904179305, 0.5758811255889696445 ) ) ;
#10185 = ORIENTED_EDGE ( 'NONE', *, *, #5475, .T. ) ;
#10186 = ORIENTED_EDGE ( 'NONE', *, *, #17003, .F. ) ;
#10187 = AXIS2_PLACEMENT_3D ( 'NONE', #21208, #12353, #5555 ) ;
#10188 = EDGE_CURVE ( 'NONE', #35163, #34957, #4679, .T. ) ;
#10189 = EDGE_CURVE ( 'NONE', #33895, #37954, #40213, .T. ) ;
#10190 = CARTESIAN_POINT ( 'NONE',  ( 0.3818955917259486132, -1.608577936064920832, 0.5280597390133632274 ) ) ;
#10191 = CARTESIAN_POINT ( 'NONE',  ( 0.1153473914419797103, -0.4465972332940850720, 0.1475347861288875961 ) ) ;
#10192 = CIRCLE ( 'NONE', #11513, 0.09088067974298034979 ) ;
#10193 = EDGE_CURVE ( 'NONE', #25764, #20672, #8668, .T. ) ;
#10194 = CARTESIAN_POINT ( 'NONE',  ( -0.05634307799789452925, 0.2614070397638449950, 0.3772863199289416825 ) ) ;
#10195 = CIRCLE ( 'NONE', #40399, 2.001558204291732146 ) ;
#10196 = APPLIED_APPROVAL_ASSIGNMENT ( #30299, ( #25296 ) ) ;
#10197 = DIRECTION ( 'NONE',  ( 0.000000000000000000, 0.000000000000000000, -1.000000000000000000 ) ) ;
#10198 = PLANE ( 'NONE',  #14825 ) ;
#10199 = AXIS2_PLACEMENT_3D ( 'NONE', #5579, #40131, #21452 ) ;
#10200 = CARTESIAN_POINT ( 'NONE',  ( 0.6326847266287998206, -1.322366380368365180, 0.7606069447649664861 ) ) ;
#10201 = DIRECTION ( 'NONE',  ( 0.3468893892380809363, -0.3199132558029670337, 0.8816593788961679667 ) ) ;
#10202 = ADVANCED_FACE ( 'NONE', ( #38299 ), #643, .T. ) ;
#10203 = CARTESIAN_POINT ( 'NONE',  ( 0.06367953181181854050, -1.330828220450373855, 0.6041689818902572506 ) ) ;
#10204 = APPLIED_PERSON_AND_ORGANIZATION_ASSIGNMENT ( #32102, #19753, ( #2940 ) ) ;
#10205 = CARTESIAN_POINT ( 'NONE',  ( 0.05561310505366643536, 0.4442420632723487195, -0.1228816621031056378 ) ) ;
#10206 = CARTESIAN_POINT ( 'NONE',  ( 0.5313741818379943416, -1.669536910112647377, -0.5811632390357616140 ) ) ;
#10207 = ORIENTED_EDGE ( 'NONE', *, *, #25563, .T. ) ;
#10208 = CARTESIAN_POINT ( 'NONE',  ( 0.2218534108553797402, -0.9537299479064303975, 0.6731843348530399673 ) ) ;
#10209 = CARTESIAN_POINT ( 'NONE',  ( 0.03664605387828149402, -0.3149102792626756742, 0.3635688186731572125 ) ) ;
#10210 = CARTESIAN_POINT ( 'NONE',  ( -0.1107910466892924328, -0.04310840302198022667, 0.3599999999999991540 ) ) ;
#10211 = ORIENTED_EDGE ( 'NONE', *, *, #23752, .F. ) ;
#10212 = CARTESIAN_POINT ( 'NONE',  ( 0.4115766028365042128, -1.733048369835246794, 0.5182417262812423209 ) ) ;
#10213 = CARTESIAN_POINT ( 'NONE',  ( 0.2535025136047072691, -0.9395968292722070014, 0.7008665722193688774 ) ) ;
#10214 = CYLINDRICAL_SURFACE ( 'NONE', #34260, 0.5756329413417605734 ) ;
#10215 = CARTESIAN_POINT ( 'NONE',  ( 0.1581650021276240492, -1.285700486175305635, 0.4182417262808778013 ) ) ;
#10216 = AXIS2_PLACEMENT_3D ( 'NONE', #36449, #11147, #33354 ) ;
#10217 = CARTESIAN_POINT ( 'NONE',  ( 0.08853488529544603636, -0.8965169086451082459, 0.5508734361391500745 ) ) ;
#10218 = ORIENTED_EDGE ( 'NONE', *, *, #17180, .F. ) ;
#10219 = CARTESIAN_POINT ( 'NONE',  ( -0.1508021419689005160, 0.4665171419162804645, 0.3606502365330792603 ) ) ;
#10220 = CARTESIAN_POINT ( 'NONE',  ( -0.2399999999999999079, -3.286568920421631290, -0.5766864829451954222 ) ) ;
#10221 = APPLIED_APPROVAL_ASSIGNMENT ( #2114, ( #9542 ) ) ;
#10222 = CARTESIAN_POINT ( 'NONE',  ( -2.070754768975505034, -0.09959325338431362917, 0.09999999999999933942 ) ) ;
#10223 = DIRECTION ( 'NONE',  ( 0.8660512985181133550, 0.4999551463232373982, 0.000000000000000000 ) ) ;
#10224 = CARTESIAN_POINT ( 'NONE',  ( 0.4885442780260524920, -1.272859572036962650, 0.6135294268981799082 ) ) ;
#10226 = LINE ( 'NONE', #7108, #39142 ) ;
#10225 = DIRECTION ( 'NONE',  ( 1.000000000000000000, 5.544814160424620659E-16, -8.132394101956109642E-16 ) ) ;
#10227 = CARTESIAN_POINT ( 'NONE',  ( 0.4508097189255980131, -1.059596525805123202, 0.6314750327306427602 ) ) ;
#10228 = EDGE_LOOP ( 'NONE', ( #6587, #33583, #10876, #35490 ) ) ;
#10229 = CONTEXT_DEPENDENT_SHAPE_REPRESENTATION ( #32670, #33116 ) ;
#10230 = CIRCLE ( 'NONE', #33215, 0.2526340763130724976 ) ;
#10231 = DIRECTION ( 'NONE',  ( -0.8153658488301590568, -0.4895179469056346044, -0.3091127823606886760 ) ) ;
#10232 = ORIENTED_EDGE ( 'NONE', *, *, #38128, .T. ) ;
#10233 = EDGE_CURVE ( 'NONE', #22378, #27741, #25160, .T. ) ;
#10234 = CARTESIAN_POINT ( 'NONE',  ( 0.04942251982096398932, -0.5642247362408411293, 0.2638688747701836146 ) ) ;
#10236 = CARTESIAN_POINT ( 'NONE',  ( 0.3409152363046567547, -1.516880185093696154, -0.5318766032426672785 ) ) ;
#10235 = CARTESIAN_POINT ( 'NONE',  ( 0.08519720172272383929, -0.8101245899050438792, 0.1318208758437162953 ) ) ;
#10237 = CARTESIAN_POINT ( 'NONE',  ( 0.1845478187330835684, -1.892088228647428094, -0.3405287551785696754 ) ) ;
#10238 = ORIENTED_EDGE ( 'NONE', *, *, #7670, .F. ) ;
#10239 = EDGE_CURVE ( 'NONE', #2531, #16637, #30360, .T. ) ;
#10240 = VERTEX_POINT ( 'NONE', #32539 ) ;
#10241 = CARTESIAN_POINT ( 'NONE',  ( 0.3258695488805244955, -1.294614862064145333, 0.5703292412207198181 ) ) ;
#10242 = EDGE_CURVE ( 'NONE', #2236, #18399, #23517, .T. ) ;
#10243 = CARTESIAN_POINT ( 'NONE',  ( 0.1169372607101707567, -0.5676260265568476848, 0.2368506474140012752 ) ) ;
#10244 = EDGE_LOOP ( 'NONE', ( #16576, #8904, #39416, #32512 ) ) ;
#10245 = CARTESIAN_POINT ( 'NONE',  ( 0.01548846960707524721, 0.000000000000000000, 0.000000000000000000 ) ) ;
#10246 = FACE_OUTER_BOUND ( 'NONE', #21201, .T. ) ;
#10247 = CARTESIAN_POINT ( 'NONE',  ( 0.4119477494091341452, -1.689530741032903238, -0.6036133972602488740 ) ) ;
#10248 = EDGE_CURVE ( 'NONE', #12740, #11030, #29690, .T. ) ;
#10249 = CARTESIAN_POINT ( 'NONE',  ( 0.2739720158966007513, -1.679698321540450845, 0.5182417262812423209 ) ) ;
#10250 = CARTESIAN_POINT ( 'NONE',  ( 0.1999999999999788058, -2.097675824466502803, -0.2588528740066096678 ) ) ;
#10251 = CARTESIAN_POINT ( 'NONE',  ( 0.08642651716623081515, -0.7265462466526347862, 0.1036714726766719968 ) ) ;
#10252 = AXIS2_PLACEMENT_3D ( 'NONE', #26683, #30154, #39404 ) ;
#10253 = CIRCLE ( 'NONE', #18139, 0.1033070866141732325 ) ;
#10254 = CARTESIAN_POINT ( 'NONE',  ( -0.05464101615137786222, -2.196071624283071788, -0.8624000883860228894 ) ) ;
#10255 = CARTESIAN_POINT ( 'NONE',  ( 0.1750363347825162064, -1.731740520214466450, -0.6813996879367362203 ) ) ;
#10256 = ADVANCED_FACE ( 'NONE', ( #29048 ), #23101, .T. ) ;
#10257 = CARTESIAN_POINT ( 'NONE',  ( 0.3193593568291898666, -1.759991732705063150, 0.5682417262808788783 ) ) ;
#10258 = EDGE_CURVE ( 'NONE', #14931, #37238, #13294, .T. ) ;
#10259 = CARTESIAN_POINT ( 'NONE',  ( 0.06146611576415164646, -1.320267390396500318, 0.5069306018158911131 ) ) ;
#10260 = COORDINATED_UNIVERSAL_TIME_OFFSET ( 0, 0, .AHEAD. ) ;
#10261 = APPROVAL_PERSON_ORGANIZATION ( #5364, #24749, #40137 ) ;
#10262 = EDGE_CURVE ( 'NONE', #32272, #15843, #19607, .T. ) ;
#10263 = B_SPLINE_CURVE_WITH_KNOTS ( 'NONE', 3,
 ( #16257, #3700, #31674, #37853, #13356, #6557, #31472, #3279, #28385, #15834, #22035, #16649, #9667, #31882, #32080, #22643, #19135, #34958 ),
 .UNSPECIFIED., .F., .F.,
 ( 4, 2, 2, 2, 2, 2, 2, 2, 4 ),
 ( 0.001064266670126195764, 0.001883953749284820664, 0.002703640828443445564, 0.003523327907602070465, 0.004343014986760694932, 0.005162702065919320266, 0.005982389145077945600, 0.006802076224236569199, 0.007621763303395194533 ),
 .UNSPECIFIED. ) ;
#10264 = DIRECTION ( 'NONE',  ( 0.4999551463232373427, -0.8660512985181134660, 0.000000000000000000 ) ) ;
#10265 = ADVANCED_FACE ( 'NONE', ( #14230 ), #26433, .T. ) ;
#10266 = CARTESIAN_POINT ( 'NONE',  ( -0.2399999999999999079, -2.878813263491020180, -0.3823467908819087602 ) ) ;
#10267 = CARTESIAN_POINT ( 'NONE',  ( 0.1850176395162889120, -0.7468748968588784232, -0.01500765167341262980 ) ) ;
#10268 = CARTESIAN_POINT ( 'NONE',  ( 0.4627917923195704608, -1.215609717498142173, 0.4882610493429819787 ) ) ;
#10269 = VECTOR ( 'NONE', #38572, 39.37007874015748143 ) ;
#10270 = DIRECTION ( 'NONE',  ( 1.000000000000000000, 2.341930812374887555E-31, -1.664003471950578127E-31 ) ) ;
#10271 = CARTESIAN_POINT ( 'NONE',  ( 0.003124719664520368614, -0.5686731593868924461, 0.1457185332388688526 ) ) ;
#10272 = CARTESIAN_POINT ( 'NONE',  ( -5.779841274449564311E-05, -0.7442380360777858250, -0.09691552782533552346 ) ) ;
#10273 = DIRECTION ( 'NONE',  ( -6.162975822039149256E-32, 0.5237184928541297468, -0.8518913899333639961 ) ) ;
#10274 = CARTESIAN_POINT ( 'NONE',  ( 0.5137193753217319525, -1.640798741474252420, -0.6166062277181030282 ) ) ;
#10275 = DIRECTION ( 'NONE',  ( 0.8660512985181134660, 0.4999551463232372317, 0.000000000000000000 ) ) ;
#10276 = VERTEX_POINT ( 'NONE', #23701 ) ;
#10277 = ORIENTED_EDGE ( 'NONE', *, *, #4610, .F. ) ;
#10278 = DIRECTION ( 'NONE',  ( -4.930380657631323784E-32, -0.7472307839325097456, -0.6645646360916347417 ) ) ;
#10279 = EDGE_LOOP ( 'NONE', ( #21927, #11927 ) ) ;
#10280 = DIRECTION ( 'NONE',  ( 0.000000000000000000, -3.885780586188049371E-16, -1.000000000000000000 ) ) ;
#10281 = DIRECTION ( 'NONE',  ( 0.01455087615875041117, 0.9998941303973198913, 0.000000000000000000 ) ) ;
#10282 = CARTESIAN_POINT ( 'NONE',  ( 0.5314776938657069794, -1.347789272887517820, 0.7454713222889900459 ) ) ;
#10284 = ORIENTED_EDGE ( 'NONE', *, *, #9925, .T. ) ;
#10283 = DIRECTION ( 'NONE',  ( -1.000000000000000000, -1.446659165673941893E-15, 8.266623803851096388E-16 ) ) ;
#10285 = CARTESIAN_POINT ( 'NONE',  ( 0.3778447279644155388, -0.9516834458091659732, 0.7020028943473471950 ) ) ;
#10286 = AXIS2_PLACEMENT_3D ( 'NONE', #30624, #38627, #16841 ) ;
#10287 = CARTESIAN_POINT ( 'NONE',  ( 0.3491199008570403661, -1.710663813406571254, -0.5475265892256320210 ) ) ;
#10288 = ORIENTED_EDGE ( 'NONE', *, *, #20334, .F. ) ;
#10289 = CARTESIAN_POINT ( 'NONE',  ( 0.5654596793231598806, -1.618818539163461301, 0.5682417262808788783 ) ) ;
#10290 = EDGE_LOOP ( 'NONE', ( #18306, #33123, #3377, #35046, #21256, #33479, #39705, #16452, #35869, #5049, #24108, #16945, #21167, #31076, #7250, #24284 ) ) ;
#10291 = CARTESIAN_POINT ( 'NONE',  ( 0.3260790593237656299, -1.638809186220848257, 0.5607896681960787832 ) ) ;
#10293 = CARTESIAN_POINT ( 'NONE',  ( -0.03159140494780162539, -0.4819881711443532168, 0.09921162977303668584 ) ) ;
#10292 = CARTESIAN_POINT ( 'NONE',  ( 0.6147754885679747039, -1.587842851228911556, 0.4306178729423159601 ) ) ;
#10294 = DIRECTION ( 'NONE',  ( 0.000000000000000000, 0.000000000000000000, -1.000000000000000000 ) ) ;
#10295 = ORGANIZATION ( 'NAUO-ORG9', 'UNSPECIFIED', 'UNSPECIFIED' ) ;
#10296 = EDGE_CURVE ( 'NONE', #15679, #31508, #4546, .T. ) ;
#10297 = CARTESIAN_POINT ( 'NONE',  ( 0.1106902893256054288, -1.391740630825941905, -0.3302364130144593291 ) ) ;
#10298 = ORIENTED_EDGE ( 'NONE', *, *, #28045, .T. ) ;
#10299 = ADVANCED_FACE ( 'NONE', ( #16918 ), #16716, .T. ) ;
#10300 = CARTESIAN_POINT ( 'NONE',  ( 0.3211164138312800898, -1.297326394713050890, 0.5856983068966360451 ) ) ;
#10301 = AXIS2_PLACEMENT_3D ( 'NONE', #25589, #6841, #16330 ) ;
#10302 = CARTESIAN_POINT ( 'NONE',  ( 0.2342238878248118772, -0.8684236987200721902, 0.4577198892158801935 ) ) ;
#10303 = DIRECTION ( 'NONE',  ( 1.000000000000000000, 0.000000000000000000, 0.000000000000000000 ) ) ;
#10304 = FACE_OUTER_BOUND ( 'NONE', #10661, .T. ) ;
#10305 = CARTESIAN_POINT ( 'NONE',  ( 0.1220082445362224849, -0.8490970766526738656, 0.4167849038607836509 ) ) ;
#10306 = DIRECTION ( 'NONE',  ( -1.000000000000000000, -0.000000000000000000, -0.000000000000000000 ) ) ;
#10307 = CARTESIAN_POINT ( 'NONE',  ( 0.4904112910084882371, -1.188461936721588064, 0.4182417262808778013 ) ) ;
#10308 = CARTESIAN_POINT ( 'NONE',  ( -0.1638575715552355871, 0.5090525736529738499, 0.3414257732885147556 ) ) ;
#10309 = CARTESIAN_POINT ( 'NONE',  ( 0.1901695884098246192, -0.5023773489605839471, 0.1477569985384105666 ) ) ;
#10310 = CARTESIAN_POINT ( 'NONE',  ( 0.1499999999999994671, 0.5203207976467930651, -0.08861466064782039243 ) ) ;
#10311 = FACE_OUTER_BOUND ( 'NONE', #30779, .T. ) ;
#10312 = PERSON_AND_ORGANIZATION ( #28500, #32463 ) ;
#10313 = CIRCLE ( 'NONE', #33285, 0.09249999999977555343 ) ;
#10314 = EDGE_CURVE ( 'NONE', #27272, #7871, #17230, .T. ) ;
#10315 = CARTESIAN_POINT ( 'NONE',  ( 0.02242828275838585836, -0.3548975010106722450, 0.3695194593235500702 ) ) ;
#10316 = CARTESIAN_POINT ( 'NONE',  ( 0.1782715084618822221, -0.4916008192336085991, 0.1361683654214305150 ) ) ;
#10317 = CARTESIAN_POINT ( 'NONE',  ( 0.1976446668592635181, -2.032347859264719059, -0.6786056056212084187 ) ) ;
#10318 = ORIENTED_EDGE ( 'NONE', *, *, #3164, .F. ) ;
#10319 = CARTESIAN_POINT ( 'NONE',  ( 0.4840003331797737562, -1.673488358279072941, 0.5079737477917150024 ) ) ;
#10320 = CARTESIAN_POINT ( 'NONE',  ( 0.3707960435722095216, -1.730448033722604251, -0.6824770964179540655 ) ) ;
#10321 = FACE_OUTER_BOUND ( 'NONE', #11694, .T. ) ;
#10322 = DIRECTION ( 'NONE',  ( 1.000000000000000000, -1.195566832711449733E-12, 1.235392033522785979E-12 ) ) ;
#10323 = CIRCLE ( 'NONE', #23470, 0.009999999999999960310 ) ;
#10324 = FACE_OUTER_BOUND ( 'NONE', #31664, .T. ) ;
#10325 = EDGE_LOOP ( 'NONE', ( #27988, #19017, #1430, #13447 ) ) ;
#10326 = CARTESIAN_POINT ( 'NONE',  ( 0.2705736468062067690, -1.683571660621278943, 0.6651229586412615857 ) ) ;
#10327 = CARTESIAN_POINT ( 'NONE',  ( 0.5984989131615597868, -1.474188139544028608, 0.6628805706823384103 ) ) ;
#10329 = ORIENTED_EDGE ( 'NONE', *, *, #10456, .F. ) ;
#10328 = CARTESIAN_POINT ( 'NONE',  ( 0.5860257985473389386, -1.592810714289445650, 0.4182417262808776903 ) ) ;
#10331 = VERTEX_POINT ( 'NONE', #20214 ) ;
#10330 = EDGE_LOOP ( 'NONE', ( #3241, #12531, #7323, #13306 ) ) ;
#10332 = CARTESIAN_POINT ( 'NONE',  ( -0.08000000000000000167, -2.183180860297908144, -0.4937760292030871079 ) ) ;
#10333 = ORIENTED_EDGE ( 'NONE', *, *, #2937, .F. ) ;
#10334 = DIRECTION ( 'NONE',  ( 0.8660512985181133550, 0.4999551463232373427, 9.313118160219073865E-16 ) ) ;
#10335 = CARTESIAN_POINT ( 'NONE',  ( 0.6293241097234876236, -1.615960343088709505, -0.5667764449061211129 ) ) ;
#10336 = ITEM_DEFINED_TRANSFORMATION ( 'NONE', 'NONE', #39050,  #27819 ) ;
#10337 = EDGE_CURVE ( 'NONE', #23348, #6307, #28233, .T. ) ;
#10338 = CARTESIAN_POINT ( 'NONE',  ( 0.002922335949518027436, -0.5275076572294762345, 0.04185307883324664718 ) ) ;
#10339 = VERTEX_POINT ( 'NONE', #7431 ) ;
#10340 = TOROIDAL_SURFACE ( 'NONE', #33313, 0.9237847906030132172, 0.01499999999999999944 ) ;
#10341 = CARTESIAN_POINT ( 'NONE',  ( 0.1015825433511447218, -0.8064352114398918303, 0.3490809539757221969 ) ) ;
#10342 = APPLICATION_CONTEXT ( 'configuration controlled 3d designs of mechanical parts and assemblies' ) ;
#10343 = CARTESIAN_POINT ( 'NONE',  ( 0.08990669076543263138, -0.5646496350939130826, 0.1479540721674596493 ) ) ;
#10344 =( BOUNDED_SURFACE ( )  B_SPLINE_SURFACE ( 3, 2, ( 
 ( #32064, #3872, #26506 ),
 ( #10453, #35959, #25914 ),
 ( #20140, #26719, #39248 ),
 ( #19531, #23019, #32456 ) ),
 .UNSPECIFIED., .F., .F., .T. ) 
 B_SPLINE_SURFACE_WITH_KNOTS ( ( 4, 4 ),
 ( 3, 3 ),
 ( 0.000000000000000000, 0.0002767335164478071353 ),
 ( 0.000000000000000000, 1.000000000000000000 ),
 .UNSPECIFIED. ) 
 GEOMETRIC_REPRESENTATION_ITEM ( )  RATIONAL_B_SPLINE_SURFACE ( (
 ( 1.000000000000000000, 0.7071328584466077816, 1.000000000000000000),
 ( 1.000000000000000000, 0.7071158410878489731, 1.000000000000000000),
 ( 1.000000000000000000, 0.7071067847848822030, 1.000000000000000000),
 ( 1.000000000000000000, 0.7071067811865467956, 1.000000000000000000) ) ) 
 REPRESENTATION_ITEM ( '' )  SURFACE ( )  );
#10345 = CARTESIAN_POINT ( 'NONE',  ( 0.2720353181507955131, -1.018083045546113841, 0.7834435089220197490 ) ) ;
#10346 = ORIENTED_EDGE ( 'NONE', *, *, #19973, .F. ) ;
#10347 = CARTESIAN_POINT ( 'NONE',  ( 0.05665256868255191119, -1.234311085492082016, 0.6576315090042377243 ) ) ;
#10348 = CARTESIAN_POINT ( 'NONE',  ( 0.6064149006458688929, -1.480831751486391568, 0.5848188689676782070 ) ) ;
#10349 = CARTESIAN_POINT ( 'NONE',  ( -0.1574377185082707353, 0.4885537809602777948, 0.09999999999999989453 ) ) ;
#10350 = CARTESIAN_POINT ( 'NONE',  ( 0.3558981752617644823, -1.739539538141937847, 0.5952128432464615093 ) ) ;
#10351 = CARTESIAN_POINT ( 'NONE',  ( 0.3316968599837757381, -1.522201780612220112, -0.7090643400862902679 ) ) ;
#10352 = CARTESIAN_POINT ( 'NONE',  ( 0.5156646344045052732, -1.614467889434319625, -0.5600385693181707536 ) ) ;
#10353 = CARTESIAN_POINT ( 'NONE',  ( 0.1434142660641894162, -0.6144585306666423552, 0.3449574928712252908 ) ) ;
#10354 = CARTESIAN_POINT ( 'NONE',  ( -1.069831502984013885E-05, -0.8266740528552610767, -0.07503813273732132250 ) ) ;
#10355 = CARTESIAN_POINT ( 'NONE',  ( 0.008166896316263525663, -0.6975401206106399687, -0.01226723980950392666 ) ) ;
#10356 = CARTESIAN_POINT ( 'NONE',  ( 0.4795819664771984736, -1.106247336020415917, -0.4111404562665418871 ) ) ;
#10357 = CARTESIAN_POINT ( 'NONE',  ( 0.1172021019593823543, -1.233981478044366087, 0.8520562743190572830 ) ) ;
#10358 = CARTESIAN_POINT ( 'NONE',  ( 0.3223305689799217388, -0.9241512680936796453, 0.6167986945225242268 ) ) ;
#10359 = DATE_AND_TIME ( #37713, #10868 ) ;
#10360 = EDGE_CURVE ( 'NONE', #38179, #799, #38910, .T. ) ;
#10361 = CARTESIAN_POINT ( 'NONE',  ( -0.3000000000000000999, -2.294529520598973082, -0.6534431116140350104 ) ) ;
#10362 = CARTESIAN_POINT ( 'NONE',  ( -0.02418142828330846830, 0.06026811487149354857, -0.1249999999999999029 ) ) ;
#10363 = ORIENTED_EDGE ( 'NONE', *, *, #13715, .T. ) ;
#10364 = CARTESIAN_POINT ( 'NONE',  ( 0.1424029337235096226, -1.400533250147911746, -0.3552704771134632677 ) ) ;
#10365 = CARTESIAN_POINT ( 'NONE',  ( 0.002296835029420861689, -0.5198933010532014176, 0.1443450864220853225 ) ) ;
#10366 = CARTESIAN_POINT ( 'NONE',  ( 0.1331762155611039000, -1.278701992196867199, 0.4313405395425053412 ) ) ;
#10367 = ORIENTED_EDGE ( 'NONE', *, *, #34368, .T. ) ;
#10368 = CONICAL_SURFACE ( 'NONE', #22223, 0.1400000000000007627, 1.047197551196601406 ) ;
#10369 = CARTESIAN_POINT ( 'NONE',  ( 0.6804297327399058126, -1.407484794882680745, 0.5682417262808783232 ) ) ;
#10371 = ORIENTED_EDGE ( 'NONE', *, *, #11488, .F. ) ;
#10370 = ORIENTED_EDGE ( 'NONE', *, *, #33878, .T. ) ;
#10372 = CARTESIAN_POINT ( 'NONE',  ( 0.5022839945508311699, -1.192782407697791980, 0.4224083929475445642 ) ) ;
#10373 = ORIENTED_EDGE ( 'NONE', *, *, #26993, .T. ) ;
#10374 = DIRECTION ( 'NONE',  ( 1.000000000000000000, -0.000000000000000000, -0.000000000000000000 ) ) ;
#10375 = CARTESIAN_POINT ( 'NONE',  ( 0.2901625129748762189, -1.544549902221894255, -0.3389314648480827308 ) ) ;
#10376 = CARTESIAN_POINT ( 'NONE',  ( -0.04574984450155356736, 0.4792536329485947433, -0.08732079948164463146 ) ) ;
#10377 = ORIENTED_EDGE ( 'NONE', *, *, #7142, .T. ) ;
#10378 = CARTESIAN_POINT ( 'NONE',  ( 2.760432932221084055E-19, -0.4262518876079539609, 0.1943948295682533245 ) ) ;
#10379 = CARTESIAN_POINT ( 'NONE',  ( 0.1335488240444889507, -0.7306454402582662766, 0.4913411250300099842 ) ) ;
#10380 = DIRECTION ( 'NONE',  ( 0.000000000000000000, 0.000000000000000000, -1.000000000000000000 ) ) ;
#10381 = CARTESIAN_POINT ( 'NONE',  ( 0.4697899360850255612, -1.558003200582610326, 0.5742671668342153035 ) ) ;
#10383 = CARTESIAN_POINT ( 'NONE',  ( 0.3634331063870702705, -1.729372196318228028, 0.4280548696313287715 ) ) ;
#10382 = FACE_OUTER_BOUND ( 'NONE', #8594, .T. ) ;
#10384 = CARTESIAN_POINT ( 'NONE',  ( 0.2369787301659028733, -1.147573247486365133, 0.6457685179108213491 ) ) ;
#10385 = ORIENTED_EDGE ( 'NONE', *, *, #12398, .T. ) ;
#10386 = CARTESIAN_POINT ( 'NONE',  ( 0.6343156381093978391, -1.595758837318228318, -0.5875140676452393906 ) ) ;
#10387 = CARTESIAN_POINT ( 'NONE',  ( 0.1945367592390488398, -0.5021430848050445483, 0.3156752544587705933 ) ) ;
#10388 = CARTESIAN_POINT ( 'NONE',  ( 0.05999999999999990757, -0.3458405862425447119, -0.1052451372150005060 ) ) ;
#10389 = CARTESIAN_POINT ( 'NONE',  ( -0.02953079040095560326, -0.4684706630666131133, -0.2484463060367418652 ) ) ;
#10390 = CYLINDRICAL_SURFACE ( 'NONE', #22071, 0.6114999999999938263 ) ;
#10391 = CIRCLE ( 'NONE', #16972, 0.1749999999999999889 ) ;
#10392 = CARTESIAN_POINT ( 'NONE',  ( 0.4929832608774247782, -1.104425667152665991, 0.8058332650092189242 ) ) ;
#10393 = CARTESIAN_POINT ( 'NONE',  ( 0.4561342652787643281, -1.116728573584468975, 0.5428924009958523422 ) ) ;
#10394 = CARTESIAN_POINT ( 'NONE',  ( 0.008743562632478048963, -0.8600815613495956802, 0.3724168526861249551 ) ) ;
#10395 = DIRECTION ( 'NONE',  ( 1.188678714063518424E-15, -1.000000000000000000, 0.000000000000000000 ) ) ;
#10396 = CARTESIAN_POINT ( 'NONE',  ( 0.5454085514665598655, -1.664197832243224262, -0.5577771241037264849 ) ) ;
#10397 = CARTESIAN_POINT ( 'NONE',  ( 0.3483176199711587318, -1.078699710109881194, 0.7396318397321306470 ) ) ;
#10398 = CARTESIAN_POINT ( 'NONE',  ( 0.03868649100028107024, -0.03360400204099643628, 0.4753701585314249467 ) ) ;
#10399 = EDGE_CURVE ( 'NONE', #16250, #32357, #7376, .T. ) ;
#10400 = CARTESIAN_POINT ( 'NONE',  ( -0.01548846960707416301, -0.2450655194479855747, -0.4674710490749294234 ) ) ;
#10401 = ADVANCED_FACE ( 'NONE', ( #29873 ), #4778, .T. ) ;
#10402 = VERTEX_POINT ( 'NONE', #40332 ) ;
#10403 = DIRECTION ( 'NONE',  ( -1.000000000000000000, -2.280301054154495132E-31, 1.664003471950577689E-31 ) ) ;
#10404 = CARTESIAN_POINT ( 'NONE',  ( 0.09079604095656999829, -0.5753325755772371597, 0.2071909514994974000 ) ) ;
#10405 = EDGE_CURVE ( 'NONE', #30911, #14004, #8451, .T. ) ;
#10406 = DIRECTION ( 'NONE',  ( -1.000000000000000000, 0.000000000000000000, 0.000000000000000000 ) ) ;
#10407 = DIRECTION ( 'NONE',  ( 0.000000000000000000, -1.000000000000000000, 3.330669073875470607E-16 ) ) ;
#10408 = ADVANCED_FACE ( 'NONE', ( #30475, #24308 ), #17524, .T. ) ;
#10409 = CARTESIAN_POINT ( 'NONE',  ( 0.2164536357353635254, -1.200268718222536224, 0.7409067871576232589 ) ) ;
#10410 = ORIENTED_EDGE ( 'NONE', *, *, #26256, .T. ) ;
#10411 = CARTESIAN_POINT ( 'NONE',  ( -0.03159140494780058456, -0.2432984029592178132, -0.4277399113045173284 ) ) ;
#10412 = CARTESIAN_POINT ( 'NONE',  ( 0.3946348076106268588, -1.611793502148812340, -0.3621938603178055383 ) ) ;
#10413 = DIRECTION ( 'NONE',  ( 0.000000000000000000, 0.7095423125567595912, -0.7046628319214841563 ) ) ;
#10414 = CARTESIAN_POINT ( 'NONE',  ( 0.1909286924077258640, -1.257064795538239244, -0.7462941026102620778 ) ) ;
#10415 = CARTESIAN_POINT ( 'NONE',  ( 0.4636748301137948447, -1.234986657158876122, 0.6895902313637624070 ) ) ;
#10417 = CARTESIAN_POINT ( 'NONE',  ( 0.3174184176267917934, -1.762933076790991205, 0.5319023928053214778 ) ) ;
#10416 = FACE_OUTER_BOUND ( 'NONE', #24481, .T. ) ;
#10418 = CARTESIAN_POINT ( 'NONE',  ( 0.5768838759879602041, -1.536724830852129520, -0.5579058299699864998 ) ) ;
#10419 = ORIENTED_EDGE ( 'NONE', *, *, #1875, .F. ) ;
#10420 = CARTESIAN_POINT ( 'NONE',  ( -0.1533385355407297923, 0.4750492940987078860, 0.3599999999999995981 ) ) ;
#10421 = ORIENTED_EDGE ( 'NONE', *, *, #30870, .F. ) ;
#10422 = CARTESIAN_POINT ( 'NONE',  ( 0.3875215993302730810, -1.517830918838856569, 0.8094752223628088883 ) ) ;
#10423 = ADVANCED_FACE ( 'NONE', ( #2304 ), #14845, .T. ) ;
#10425 = CARTESIAN_POINT ( 'NONE',  ( 0.1961281144780854524, -0.6676453483071772554, 0.3322964415046538722 ) ) ;
#10424 = CARTESIAN_POINT ( 'NONE',  ( 0.08604873559162301566, -0.7971672130737051942, 0.05183853996302047878 ) ) ;
#10426 = CARTESIAN_POINT ( 'NONE',  ( 0.1817694849310280136, -1.261899108304536110, 0.5084384546551340422 ) ) ;
#10427 = APPLIED_PERSON_AND_ORGANIZATION_ASSIGNMENT ( #30540, #8712, ( #1014 ) ) ;
#10428 = ORIENTED_EDGE ( 'NONE', *, *, #1226, .F. ) ;
#10429 = ORIENTED_EDGE ( 'NONE', *, *, #20141, .F. ) ;
#10430 = CARTESIAN_POINT ( 'NONE',  ( 0.3325245471243513107, -1.290768314560045038, 0.5729784808290850906 ) ) ;
#10431 = CARTESIAN_POINT ( 'NONE',  ( 0.5346825410386824018, -1.439718025093458920, 0.7637196853476909686 ) ) ;
#10432 = ORIENTED_EDGE ( 'NONE', *, *, #32108, .T. ) ;
#10433 = FACE_OUTER_BOUND ( 'NONE', #7015, .T. ) ;
#10434 = CARTESIAN_POINT ( 'NONE',  ( 0.05078310099560627566, -0.4632425114130950261, 0.09919524461158438222 ) ) ;
#10435 = CARTESIAN_POINT ( 'NONE',  ( 0.1045181657808564313, -1.266534658925821732, -0.5155029497116575543 ) ) ;
#10436 = ORIENTED_EDGE ( 'NONE', *, *, #29594, .F. ) ;
#10437 = LINE ( 'NONE', #16610, #8065 ) ;
#10438 = CARTESIAN_POINT ( 'NONE',  ( 0.3845449968151027353, -1.722577193482669022, 0.6193603067054115341 ) ) ;
#10439 = B_SPLINE_CURVE_WITH_KNOTS ( 'NONE', 3,
 ( #24782, #27257, #39786, #24176 ),
 .UNSPECIFIED., .F., .F.,
 ( 4, 4 ),
 ( 1.748223473168675632E-18, 0.0009765734425980529369 ),
 .UNSPECIFIED. ) ;
#10440 = CARTESIAN_POINT ( 'NONE',  ( 0.6100913662829361428, -1.289225211610094401, 0.8693105457786516332 ) ) ;
#10441 = CARTESIAN_POINT ( 'NONE',  ( 0.3927073942151048658, -1.776709627579699413, -0.7060183551223596643 ) ) ;
#10442 = CARTESIAN_POINT ( 'NONE',  ( 0.01548846960707497486, -0.2306506793133962230, 0.4716198300880369287 ) ) ;
#10443 = CARTESIAN_POINT ( 'NONE',  ( -0.08000000000000000167, -2.180132361182266720, -0.6941833704005058170 ) ) ;
#10444 = CALENDAR_DATE ( 2026, 13, 10 ) ;
#10445 = CARTESIAN_POINT ( 'NONE',  ( 0.05279905671744913181, 0.2420693533014125209, 0.4010177630757486011 ) ) ;
#10446 = CARTESIAN_POINT ( 'NONE',  ( 0.1839464713631710491, -0.5494516881424977850, 0.02732684068011371689 ) ) ;
#10447 = DIRECTION ( 'NONE',  ( 0.000000000000000000, 0.000000000000000000, 1.000000000000000000 ) ) ;
#10448 = DIRECTION ( 'NONE',  ( 8.881784197001246407E-16, -2.361472542561082612E-16, 1.000000000000000000 ) ) ;
#10449 = EDGE_CURVE ( 'NONE', #7197, #24171, #36832, .T. ) ;
#10450 = CARTESIAN_POINT ( 'NONE',  ( 0.02242113575389428556, -0.7151737931810984161, 0.5646644402375310401 ) ) ;
#10451 = CARTESIAN_POINT ( 'NONE',  ( 0.5895895133292542445, -1.562273338605467021, -0.5541701122963066384 ) ) ;
#10452 = EDGE_CURVE ( 'NONE', #19821, #16708, #38894, .T. ) ;
#10453 = CARTESIAN_POINT ( 'NONE',  ( -2.125292368820994835E-14, -2.101103427206035601, -0.2895067271637098982 ) ) ;
#10454 = CARTESIAN_POINT ( 'NONE',  ( -0.02000000000000000042, -2.183180860297908144, -0.4937760292030871079 ) ) ;
#10455 = CARTESIAN_POINT ( 'NONE',  ( -0.2343922129835737667, -0.5166151207188713901, 0.3750000000000000555 ) ) ;
#10456 = EDGE_CURVE ( 'NONE', #10562, #16113, #29062, .T. ) ;
#10457 = ORIENTED_EDGE ( 'NONE', *, *, #20738, .T. ) ;
#10458 = ORIENTED_EDGE ( 'NONE', *, *, #7180, .T. ) ;
#10459 = CARTESIAN_POINT ( 'NONE',  ( 0.4970758107849645446, -1.079867600816170059, 0.3667417262808778666 ) ) ;
#10460 = ORIENTED_EDGE ( 'NONE', *, *, #10193, .F. ) ;
#10461 = CARTESIAN_POINT ( 'NONE',  ( 0.3728661538533184494, -1.740126085018506963, 0.4331033444688550116 ) ) ;
#10462 = DIRECTION ( 'NONE',  ( -0.2147743920926263317, -0.9766636885342071528, 2.066666135092459448E-16 ) ) ;
#10463 = CARTESIAN_POINT ( 'NONE',  ( 0.4707424504419197020, -1.251593692541077107, 0.7595398601079852430 ) ) ;
#10465 = VERTEX_POINT ( 'NONE', #15240 ) ;
#10464 = CARTESIAN_POINT ( 'NONE',  ( 0.5935794547855036685, -1.611332463636045764, 0.4487275098415936525 ) ) ;
#10466 = CARTESIAN_POINT ( 'NONE',  ( 0.2256328605772283669, -0.7491591359250245885, 0.4461645245400559512 ) ) ;
#10467 = CARTESIAN_POINT ( 'NONE',  ( 0.3553775023099885466, -1.749316302220775832, -0.5487481164399209410 ) ) ;
#10468 = ORIENTED_EDGE ( 'NONE', *, *, #24369, .T. ) ;
#10469 = FACE_OUTER_BOUND ( 'NONE', #11692, .T. ) ;
#10470 = ORIENTED_EDGE ( 'NONE', *, *, #20567, .F. ) ;
#10471 = CARTESIAN_POINT ( 'NONE',  ( 0.3289079490030120123, -1.639352849464426498, 0.6015274726064920863 ) ) ;
#10472 = EDGE_CURVE ( 'NONE', #2281, #35264, #1747, .T. ) ;
#10474 = CARTESIAN_POINT ( 'NONE',  ( -0.04155248107635971938, -0.2623121065566123566, 0.3903559784317158776 ) ) ;
#10473 = CYLINDRICAL_SURFACE ( 'NONE', #33151, 0.1749999999999999889 ) ;
#10475 = CARTESIAN_POINT ( 'NONE',  ( 0.1438681892407857876, -1.284094082863941111, 0.3157417262808777658 ) ) ;
#10476 = CARTESIAN_POINT ( 'NONE',  ( 0.005127655334880022210, -1.809120478639261176, -0.3273012655191571696 ) ) ;
#10477 = EDGE_LOOP ( 'NONE', ( #30200, #27624, #38284, #14382 ) ) ;
#10478 = DIMENSIONAL_EXPONENTS ( 1.000000000000000000, 0.000000000000000000, 0.000000000000000000, 0.000000000000000000, 0.000000000000000000, 0.000000000000000000, 0.000000000000000000 ) ;
#10479 = CARTESIAN_POINT ( 'NONE',  ( 0.5447018010467034044, -1.168331122704159286, 0.5148643787740219135 ) ) ;
#10480 = CARTESIAN_POINT ( 'NONE',  ( 0.1866070744275658277, -0.9155653071574156865, 0.1780381001982239975 ) ) ;
#10481 = B_SPLINE_CURVE_WITH_KNOTS ( 'NONE', 3,
 ( #23754, #27034, #20880, #23967, #26844, #36274, #14681, #36696, #30728, #8096, #32989, #29926, #30121, #8310, #2143, #21067, #17763, #1952 ),
 .UNSPECIFIED., .F., .F.,
 ( 4, 2, 2, 2, 2, 2, 2, 2, 4 ),
 ( -0.003133633995111093605, -0.002350221109836652788, -0.001566808224562211971, -0.0007833953392877711537, 1.754598666966339371E-08, 0.0007834304312611109142, 0.001566843316535551298, 0.002350256201809991681, 0.003133669087084432932 ),
 .UNSPECIFIED. ) ;
#10482 = CARTESIAN_POINT ( 'NONE',  ( -0.3000000000000000999, -1.891808285041389093, -0.4498908273618595910 ) ) ;
#10483 = DIRECTION ( 'NONE',  ( 0.4999551463232373427, -0.8660512985181134660, 0.000000000000000000 ) ) ;
#10484 = CARTESIAN_POINT ( 'NONE',  ( 0.1573455698924841606, -0.8938959663910659437, 0.5707458213001018743 ) ) ;
#10485 = CARTESIAN_POINT ( 'NONE',  ( 0.1058066437981236146, -1.050304887260346876, 0.8576506362211480106 ) ) ;
#10486 = CARTESIAN_POINT ( 'NONE',  ( 0.4905684254636979436, -1.178471512614451822, 0.4182417262808778013 ) ) ;
#10487 = CARTESIAN_POINT ( 'NONE',  ( -0.1743922129835737966, -0.5166151207188712791, 0.08499999999999977018 ) ) ;
#10488 = DIRECTION ( 'NONE',  ( 0.000000000000000000, 0.9510565162951636342, 0.3090169943749164205 ) ) ;
#10489 = DIRECTION ( 'NONE',  ( -1.000000000000000000, -2.280301054154495132E-31, 1.664003471950577689E-31 ) ) ;
#10490 = DIRECTION ( 'NONE',  ( -0.01254811300245605755, -0.8659344938869285579, -0.4999999971568663826 ) ) ;
#10491 =( NAMED_UNIT ( * ) SI_UNIT ( $, .STERADIAN. ) SOLID_ANGLE_UNIT ( ) );
#10492 = B_SPLINE_CURVE_WITH_KNOTS ( 'NONE', 3,
 ( #8777, #15149, #12079, #2814 ),
 .UNSPECIFIED., .F., .F.,
 ( 4, 4 ),
 ( 0.000000000000000000, 0.001825717054875163579 ),
 .UNSPECIFIED. ) ;
#10493 = CARTESIAN_POINT ( 'NONE',  ( 0.01387309669645373639, -1.022410628767960405, 0.5763875663499552493 ) ) ;
#10494 = CARTESIAN_POINT ( 'NONE',  ( 0.1759300380180284507, -1.231083256582695684, -0.4125659523519146221 ) ) ;
#10495 = CARTESIAN_POINT ( 'NONE',  ( 0.1084311124255188524, -1.402644867855400657, 0.6343705678861770725 ) ) ;
#10496 = ORIENTED_EDGE ( 'NONE', *, *, #17547, .F. ) ;
#10497 = CARTESIAN_POINT ( 'NONE',  ( 0.4719957491900099722, -1.679875000564180709, 0.4688966813032011682 ) ) ;
#10498 = CARTESIAN_POINT ( 'NONE',  ( 0.2002642730199227783, -1.651659577068177676, -0.6582679755329989835 ) ) ;
#10499 = EDGE_CURVE ( 'NONE', #23694, #26277, #21220, .T. ) ;
#10500 = CARTESIAN_POINT ( 'NONE',  ( -0.01548846960707538425, 0.09319974324248773978, -0.5318964258758787089 ) ) ;
#10501 = CARTESIAN_POINT ( 'NONE',  ( 0.1761268469877938225, -1.381065068506146298, -0.3150366247064029235 ) ) ;
#10502 = ORIENTED_EDGE ( 'NONE', *, *, #6998, .T. ) ;
#10503 = CARTESIAN_POINT ( 'NONE',  ( -0.1443922129835728263, -0.5166151207188712791, 0.08499999999999961753 ) ) ;
#10504 = EDGE_LOOP ( 'NONE', ( #1757, #31120, #6319, #7864 ) ) ;
#10505 = EDGE_CURVE ( 'NONE', #25709, #20955, #22507, .T. ) ;
#10506 = DIRECTION ( 'NONE',  ( -1.000000000000000000, 0.000000000000000000, 0.000000000000000000 ) ) ;
#10507 = CARTESIAN_POINT ( 'NONE',  ( 0.6007894471599048991, -1.477974513124123312, 0.6406838331186633928 ) ) ;
#10509 = ORIENTED_EDGE ( 'NONE', *, *, #18086, .T. ) ;
#10508 = DIRECTION ( 'NONE',  ( -1.000000000000000000, -0.000000000000000000, -0.000000000000000000 ) ) ;
#10511 = ORIENTED_EDGE ( 'NONE', *, *, #5434, .F. ) ;
#10510 = ORIENTED_EDGE ( 'NONE', *, *, #39691, .T. ) ;
#10512 = DIRECTION ( 'NONE',  ( -0.4999999999999957812, -0.3085698060533151876, -0.8091876635195469625 ) ) ;
#10513 = VERTEX_POINT ( 'NONE', #33755 ) ;
#10514 = ORIENTED_EDGE ( 'NONE', *, *, #37719, .F. ) ;
#10515 = DIRECTION ( 'NONE',  ( 0.9378410757839510392, -0.3470650033817896385, 0.000000000000000000 ) ) ;
#10516 = DIRECTION ( 'NONE',  ( 1.000000000000000000, 0.000000000000000000, 0.000000000000000000 ) ) ;
#10517 = CARTESIAN_POINT ( 'NONE',  ( -0.2399999999999999079, -2.945416957892569521, -0.4639726661791638840 ) ) ;
#10518 = EDGE_CURVE ( 'NONE', #4981, #29632, #34973, .T. ) ;
#10519 = DATE_AND_TIME ( #39119, #12278 ) ;
#10520 = APPLIED_DATE_AND_TIME_ASSIGNMENT ( #11937, #24502, ( #38548 ) ) ;
#10521 = CARTESIAN_POINT ( 'NONE',  ( 0.002762111618723705336, -0.9534082139883239826, -0.1178596299512794793 ) ) ;
#10523 = EDGE_LOOP ( 'NONE', ( #15605, #28554, #34995, #18685 ) ) ;
#10522 = ORIENTED_EDGE ( 'NONE', *, *, #10982, .T. ) ;
#10524 = EDGE_CURVE ( 'NONE', #34849, #10078, #37601, .T. ) ;
#10525 = CARTESIAN_POINT ( 'NONE',  ( 0.1845623500247081106, -0.8903488908324218576, 0.5922637714853882240 ) ) ;
#10526 = CARTESIAN_POINT ( 'NONE',  ( 0.06924657340766243729, -0.5400045880099085815, 0.1370866209488758869 ) ) ;
#10527 = CARTESIAN_POINT ( 'NONE',  ( 0.1100840907954307585, -0.5526133480759019001, 0.1897287169192503620 ) ) ;
#10528 = ORIENTED_EDGE ( 'NONE', *, *, #19783, .T. ) ;
#10529 = CARTESIAN_POINT ( 'NONE',  ( 0.03468330715085447130, -1.089634729100930954, 0.6338593068032741806 ) ) ;
#10530 = CARTESIAN_POINT ( 'NONE',  ( 0.4935456730871101150, -1.587903313234494629, -0.4610633267758252329 ) ) ;
#10531 = CARTESIAN_POINT ( 'NONE',  ( -0.03309059653085701797, 0.08822156176788366333, 0.5132714489379847089 ) ) ;
#10532 = CIRCLE ( 'NONE', #21053, 0.03749999999977545601 ) ;
#10533 = CARTESIAN_POINT ( 'NONE',  ( 0.3379905402051226471, -1.761107921090772299, 0.5690149188013547965 ) ) ;
#10534 = CARTESIAN_POINT ( 'NONE',  ( 0.3332516724025844645, -1.614750829017314926, -0.6926149471072686747 ) ) ;
#10535 = FACE_OUTER_BOUND ( 'NONE', #10555, .T. ) ;
#10536 = CARTESIAN_POINT ( 'NONE',  ( 0.05999999999999990757, -0.1354409211049039941, -0.1857769145426272639 ) ) ;
#10537 = VECTOR ( 'NONE', #10716, 39.37007874015748854 ) ;
#10538 = DIRECTION ( 'NONE',  ( -0.000000000000000000, 0.8090169943749540016, 0.5877852522924639223 ) ) ;
#10539 = CARTESIAN_POINT ( 'NONE',  ( -0.0003095478128742020006, -0.9052138808146785731, 0.02354638163038534626 ) ) ;
#10540 = CARTESIAN_POINT ( 'NONE',  ( 0.5171109296076384920, -1.359203088151551331, 0.7981695906224013370 ) ) ;
#10541 = CARTESIAN_POINT ( 'NONE',  ( 0.4970758107849645446, -1.079867600816170059, 0.3667417262808778666 ) ) ;
#10542 = LINE ( 'NONE', #19203, #4224 ) ;
#10543 = CARTESIAN_POINT ( 'NONE',  ( 0.1172025164431036715, -1.392648223243311723, 0.6963985612953286219 ) ) ;
#10544 = CARTESIAN_POINT ( 'NONE',  ( 0.3630793090018165636, -0.9924503543686107321, 0.6290125294248597454 ) ) ;
#10545 = APPROVAL_DATE_TIME ( #23330, #22974 ) ;
#10546 = EDGE_CURVE ( 'NONE', #13556, #27730, #5157, .T. ) ;
#10547 = B_SPLINE_CURVE_WITH_KNOTS ( 'NONE', 3,
 ( #36112, #10613, #1381, #17608, #4621, #14503, #4831, #17402, #39001, #7732 ),
 .UNSPECIFIED., .F., .F.,
 ( 4, 2, 2, 2, 4 ),
 ( 0.000000000000000000, 0.0005419198834577468185, 0.001083839766915493637, 0.001625759650373240564, 0.002167679533830987274 ),
 .UNSPECIFIED. ) ;
#10548 = FACE_OUTER_BOUND ( 'NONE', #11726, .T. ) ;
#10549 = DIRECTION ( 'NONE',  ( -0.1766035691529960483, -0.1934850654821817784, 0.9650775662079078554 ) ) ;
#10550 = VERTEX_POINT ( 'NONE', #5348 ) ;
#10551 = CARTESIAN_POINT ( 'NONE',  ( 0.2059273467974224725, -1.283046334493782137, -0.3824824602286829855 ) ) ;
#10552 = CARTESIAN_POINT ( 'NONE',  ( 0.002514036842440564665, -0.5353143163907467805, 0.2306785804606524271 ) ) ;
#10553 = TOROIDAL_SURFACE ( 'NONE', #3969, 0.05330708661417323663, 0.01000000000000000021 ) ;
#10554 = CARTESIAN_POINT ( 'NONE',  ( 0.6473787150721044270, -1.455279521797666176, -0.6250000000000000000 ) ) ;
#10555 = EDGE_LOOP ( 'NONE', ( #19403, #12144, #19236, #7723 ) ) ;
#10556 = CARTESIAN_POINT ( 'NONE',  ( 0.5318889985472864401, -1.659866604704374637, -0.4542321257220686137 ) ) ;
#10557 = CARTESIAN_POINT ( 'NONE',  ( 0.1895831464430141888, -0.5047047246472139426, 0.1503823323309240734 ) ) ;
#10559 = ORIENTED_EDGE ( 'NONE', *, *, #33818, .T. ) ;
#10558 = ORIENTED_EDGE ( 'NONE', *, *, #38815, .T. ) ;
#10560 = DIRECTION ( 'NONE',  ( 0.000000000000000000, 0.000000000000000000, 1.000000000000000000 ) ) ;
#10561 = AXIS2_PLACEMENT_3D ( 'NONE', #10222, #9799, #16201 ) ;
#10562 = VERTEX_POINT ( 'NONE', #27408 ) ;
#10563 = CARTESIAN_POINT ( 'NONE',  ( 0.3587246564956185768, -1.771947280444475137, -0.5205743448439883458 ) ) ;
#10564 = CARTESIAN_POINT ( 'NONE',  ( 0.3819720823480106109, -1.699928762836120377, -0.3361580370732986101 ) ) ;
#10565 = AXIS2_PLACEMENT_3D ( 'NONE', #3333, #25378, #31345 ) ;
#10566 = CARTESIAN_POINT ( 'NONE',  ( -0.04229883635637986250, 0.4470233673486225245, -0.1406638142521441093 ) ) ;
#10567 = ORIENTED_EDGE ( 'NONE', *, *, #662, .F. ) ;
#10568 = CARTESIAN_POINT ( 'NONE',  ( 0.5457411013609096972, -1.645686818912574179, 0.8576316932085735756 ) ) ;
#10569 = CARTESIAN_POINT ( 'NONE',  ( 0.1145849041649253802, -0.6984622373509431492, 0.4166132103181554580 ) ) ;
#10570 = CARTESIAN_POINT ( 'NONE',  ( 0.06413938869033396217, -0.7427754723600979991, 0.7547169867245954178 ) ) ;
#10571 = CARTESIAN_POINT ( 'NONE',  ( 0.08541776836348415058, -0.5463775883488639629, 0.1813289453475219748 ) ) ;
#10573 = CARTESIAN_POINT ( 'NONE',  ( -0.1743922129835733803, -0.5166151207188712791, 0.3749999999999999445 ) ) ;
#10572 = DIRECTION ( 'NONE',  ( 1.787262988391355310E-31, 0.4685245517978617324, -0.8834504764629497187 ) ) ;
#10574 = CARTESIAN_POINT ( 'NONE',  ( 0.1986024623659905786, -1.088350075686307816, 0.6415510412962815989 ) ) ;
#10575 = EDGE_LOOP ( 'NONE', ( #9603, #8229, #40192, #15636 ) ) ;
#10576 = ORIENTED_EDGE ( 'NONE', *, *, #36088, .T. ) ;
#10577 = EDGE_CURVE ( 'NONE', #4305, #35302, #15910, .T. ) ;
#10578 = FACE_OUTER_BOUND ( 'NONE', #24970, .T. ) ;
#10579 = CARTESIAN_POINT ( 'NONE',  ( 0.1899112346947867958, -0.5366114675534041645, 0.1755787374122024513 ) ) ;
#10580 = DIRECTION ( 'NONE',  ( 0.9998941247116546194, -0.01455087607601020412, 0.0001066420868422379362 ) ) ;
#10581 = CARTESIAN_POINT ( 'NONE',  ( -0.05279185365593355023, -0.4315575715699441206, -0.1821760513485178312 ) ) ;
#10582 = CIRCLE ( 'NONE', #11234, 0.09999999999999999167 ) ;
#10583 = LINE ( 'NONE', #26438, #33229 ) ;
#10584 = B_SPLINE_CURVE_WITH_KNOTS ( 'NONE', 3,
 ( #15122, #28487, #34663, #30963, #27680, #25204, #34457, #37747, #5849, #31182 ),
 .UNSPECIFIED., .F., .F.,
 ( 4, 2, 2, 2, 4 ),
 ( -0.003133633995111221975, -0.002350225496333395447, -0.001566816997555568487, -0.0007834084987777415257, 8.586881206085195117E-17 ),
 .UNSPECIFIED. ) ;
#10585 = AXIS2_PLACEMENT_3D ( 'NONE', #30828, #11704, #33489 ) ;
#10586 = CARTESIAN_POINT ( 'NONE',  ( -2.070754768975505034, -0.09959325338431362917, 0.09813923389047245205 ) ) ;
#10587 = CARTESIAN_POINT ( 'NONE',  ( 0.4865355734717750624, -1.097175741254786452, 0.7494200075675998551 ) ) ;
#10588 = AXIS2_PLACEMENT_3D ( 'NONE', #5241, #34242, #12252 ) ;
#10589 = CARTESIAN_POINT ( 'NONE',  ( 0.4933430811445716491, -1.186754567874577226, 0.4151382928142203221 ) ) ;
#10590 = CARTESIAN_POINT ( 'NONE',  ( -0.002362956560267360107, -0.8470628361959046115, 0.1913124104053905150 ) ) ;
#10591 = VECTOR ( 'NONE', #17644, 39.37007874015748143 ) ;
#10592 = CIRCLE ( 'NONE', #1433, 0.6115209409081865388 ) ;
#10593 = CARTESIAN_POINT ( 'NONE',  ( 0.04575106512774645279, 0.4390484599015499478, -0.2110503898921174404 ) ) ;
#10594 = CARTESIAN_POINT ( 'NONE',  ( 0.3247155104185332486, -1.295292661530707878, 0.4306002955320518133 ) ) ;
#10595 = CARTESIAN_POINT ( 'NONE',  ( 0.4065905862282702676, -1.156565771161806921, 0.7145884245918578959 ) ) ;
#10596 = DIRECTION ( 'NONE',  ( -1.387778780781449423E-15, 6.590151126658376924E-16, -1.000000000000000000 ) ) ;
#10597 = CARTESIAN_POINT ( 'NONE',  ( -0.05076541221973714102, -0.2374623881706939277, -0.4099867295868578343 ) ) ;
#10598 = ORIENTED_EDGE ( 'NONE', *, *, #24589, .T. ) ;
#10599 = LINE ( 'NONE', #16374, #10154 ) ;
#10600 = CARTESIAN_POINT ( 'NONE',  ( 0.03113248654051816583, 0.1919340784543128453, -0.1767348310837237868 ) ) ;
#10601 = DIRECTION ( 'NONE',  ( 1.000000000000000000, 2.276539994720212446E-15, -1.138269997360106223E-15 ) ) ;
#10602 = CARTESIAN_POINT ( 'NONE',  ( 0.4209449764515663106, -1.127703425338436372, 0.4919882752232563328 ) ) ;
#10603 = CIRCLE ( 'NONE', #15870, 0.01000000000000002970 ) ;
#10604 = CARTESIAN_POINT ( 'NONE',  ( 0.05856722883986545392, -0.8414967731140865492, 0.2843716283219245855 ) ) ;
#10605 = ORIENTED_EDGE ( 'NONE', *, *, #40072, .T. ) ;
#10606 = CARTESIAN_POINT ( 'NONE',  ( -0.03868649100028244414, -0.3066017772948799180, -0.3648306000529315529 ) ) ;
#10607 = CARTESIAN_POINT ( 'NONE',  ( 0.02238826743733661473, 0.06997574608431179899, 0.5076331681966321785 ) ) ;
#10608 = CARTESIAN_POINT ( 'NONE',  ( 0.02881408050861775094, -0.4889293851945573643, -0.09562755728437868918 ) ) ;
#10609 = LINE ( 'NONE', #28923, #9473 ) ;
#10610 = CARTESIAN_POINT ( 'NONE',  ( 0.4340920373745369432, -1.192938021670690407, 0.7091433560946051040 ) ) ;
#10611 = TOROIDAL_SURFACE ( 'NONE', #33598, 0.2200000000000000011, 0.02999999999999999889 ) ;
#10613 = CARTESIAN_POINT ( 'NONE',  ( 0.5346239700487379620, -1.154911596989372846, 0.5682481700188124485 ) ) ;
#10612 = DIRECTION ( 'NONE',  ( 5.551115123125774690E-17, 0.000000000000000000, -1.000000000000000000 ) ) ;
#10614 = CARTESIAN_POINT ( 'NONE',  ( 0.2370370725713593918, -0.9423068241879761775, 0.4501375130042485906 ) ) ;
#10615 = ORIENTED_EDGE ( 'NONE', *, *, #37405, .F. ) ;
#10616 = LINE ( 'NONE', #7736, #38185 ) ;
#10617 = ORIENTED_EDGE ( 'NONE', *, *, #18426, .T. ) ;
#10618 = CIRCLE ( 'NONE', #21145, 0.04749999999977550652 ) ;
#10619 = CIRCLE ( 'NONE', #3499, 0.01499999999999999251 ) ;
#10620 = CARTESIAN_POINT ( 'NONE',  ( 0.2438426133570002763, -1.175331807871637269, 0.8706532464808368621 ) ) ;
#10622 = CARTESIAN_POINT ( 'NONE',  ( 0.2018363294977822686, -0.7308029772144113423, 0.3390199763628233831 ) ) ;
#10621 = CARTESIAN_POINT ( 'NONE',  ( 0.06797573035266660235, -0.5960914377309097789, 0.02939662547896050929 ) ) ;
#10623 = CARTESIAN_POINT ( 'NONE',  ( 0.2402595592073158148, -1.589192177423347285, -0.3527948934348379972 ) ) ;
#10624 = ORIENTED_EDGE ( 'NONE', *, *, #33012, .F. ) ;
#10625 = AXIS2_PLACEMENT_3D ( 'NONE', #22366, #6496, #19274 ) ;
#10626 = ORIENTED_EDGE ( 'NONE', *, *, #23796, .T. ) ;
#10627 = DIRECTION ( 'NONE',  ( -0.000000000000000000, -0.6595282642760672553, -0.7516797646744243222 ) ) ;
#10628 = EDGE_CURVE ( 'NONE', #26041, #21164, #38059, .T. ) ;
#10629 = ADVANCED_FACE ( 'NONE', ( #9872 ), #13159, .T. ) ;
#10630 = CARTESIAN_POINT ( 'NONE',  ( 0.1197446008095364028, -0.5662179169742945772, 0.2308386541185581120 ) ) ;
#10631 = ORIENTED_EDGE ( 'NONE', *, *, #21600, .T. ) ;
#10632 = CARTESIAN_POINT ( 'NONE',  ( 0.5586419605352853646, -1.622123839695630787, -0.4759077358386838985 ) ) ;
#10633 = B_SPLINE_CURVE_WITH_KNOTS ( 'NONE', 3,
 ( #13782, #10706, #1680, #30223, #17494, #14197, #26348, #23280, #39292, #30046 ),
 .UNSPECIFIED., .F., .F.,
 ( 4, 2, 2, 2, 4 ),
 ( 3.469446951953614189E-18, 0.0005277335017653989350, 0.001055467003530794401, 0.001583200505296189758, 0.002110934007061585332 ),
 .UNSPECIFIED. ) ;
#10634 = CARTESIAN_POINT ( 'NONE',  ( 0.03478489236951123886, -0.5086709597375885794, 0.08927530733452980483 ) ) ;
#10635 = CARTESIAN_POINT ( 'NONE',  ( 0.2087112741175610464, -1.246538662281911236, 0.4623142537311495381 ) ) ;
#10636 = EDGE_CURVE ( 'NONE', #32720, #1199, #12556, .T. ) ;
#10637 = CARTESIAN_POINT ( 'NONE',  ( -0.1603938765018536328, 0.4636889572247743230, 0.1178658435936996290 ) ) ;
#10638 = CARTESIAN_POINT ( 'NONE',  ( -0.1399999999999997358, 0.000000000000000000, 0.000000000000000000 ) ) ;
#10639 = ADVANCED_FACE ( 'NONE', ( #12363 ), #15849, .F. ) ;
#10640 = CARTESIAN_POINT ( 'NONE',  ( 0.5573545814012507149, -1.203739305690170402, 0.8778060520269345135 ) ) ;
#10641 = CARTESIAN_POINT ( 'NONE',  ( 9.860761315262654615E-34, -0.4700000000000001954, 0.04000000000000001471 ) ) ;
#10642 = DIRECTION ( 'NONE',  ( 0.000000000000000000, 0.5781348229923760629, -0.8159412518334723252 ) ) ;
#10643 = CALENDAR_DATE ( 2026, 13, 10 ) ;
#10644 = AXIS2_PLACEMENT_3D ( 'NONE', #29001, #10306, #29418 ) ;
#10645 = DIRECTION ( 'NONE',  ( -0.1166888840060208155, -0.08018547039157027101, -0.9899262571967228919 ) ) ;
#10646 = CARTESIAN_POINT ( 'NONE',  ( 0.02881408050861337250, 0.3393437137871819775, 0.3647498010034102567 ) ) ;
#10647 = CARTESIAN_POINT ( 'NONE',  ( 0.1849961625554341071, -0.7276430976136223361, -0.02180148029977278454 ) ) ;
#10648 = CARTESIAN_POINT ( 'NONE',  ( 0.4168377001686644490, -1.242140235433856432, 0.4952185744155029323 ) ) ;
#10649 = CARTESIAN_POINT ( 'NONE',  ( 0.1077840105943417282, -1.313547665849942314, 0.4360032343016825851 ) ) ;
#10650 = AXIS2_PLACEMENT_3D ( 'NONE', #32140, #29262, #29462 ) ;
#10651 = AXIS2_PLACEMENT_3D ( 'NONE', #1461, #10489, #13974 ) ;
#10652 = EDGE_CURVE ( 'NONE', #15491, #5909, #20528, .T. ) ;
#10653 = APPLIED_PERSON_AND_ORGANIZATION_ASSIGNMENT ( #34637, #16135, ( #26657 ) ) ;
#10654 = CARTESIAN_POINT ( 'NONE',  ( 0.2890670123411187564, -1.729633309587475187, 0.5682417262808785452 ) ) ;
#10655 = CARTESIAN_POINT ( 'NONE',  ( 0.5781467389326836459, -1.533504052124724293, -0.5635290765616033370 ) ) ;
#10656 = AXIS2_PLACEMENT_3D ( 'NONE', #38546, #19826, #38132 ) ;
#10657 = DIRECTION ( 'NONE',  ( -1.000000000000000000, -0.000000000000000000, -0.000000000000000000 ) ) ;
#10658 = FACE_OUTER_BOUND ( 'NONE', #34950, .T. ) ;
#10659 = CARTESIAN_POINT ( 'NONE',  ( -0.04047076529493409680, -0.3430644450807453505, 0.3654777640200593813 ) ) ;
#10660 = ORIENTED_EDGE ( 'NONE', *, *, #24826, .T. ) ;
#10661 = EDGE_LOOP ( 'NONE', ( #7974, #5010, #18673, #15892, #21618, #4252, #23234 ) ) ;
#10662 = DIRECTION ( 'NONE',  ( 0.000000000000000000, 0.000000000000000000, -1.000000000000000000 ) ) ;
#10663 = ORIENTED_EDGE ( 'NONE', *, *, #19006, .F. ) ;
#10664 = CARTESIAN_POINT ( 'NONE',  ( -0.1163200376094534610, -0.5319009979872302285, 0.1426078552794932397 ) ) ;
#10665 = CYLINDRICAL_SURFACE ( 'NONE', #6819, 0.4614999999999880864 ) ;
#10666 = CARTESIAN_POINT ( 'NONE',  ( 0.4760599958747125937, -1.259643329453308924, 0.7570774943031273185 ) ) ;
#10668 = VERTEX_POINT ( 'NONE', #34765 ) ;
#10667 = CARTESIAN_POINT ( 'NONE',  ( -0.1566201954065875035, 0.4859225043295781199, 0.1133527062597455004 ) ) ;
#10669 = CARTESIAN_POINT ( 'NONE',  ( 0.3146548270004942971, -0.9167534899940792403, 0.6079632372063322743 ) ) ;
#10670 = DIRECTION ( 'NONE',  ( 0.000000000000000000, 0.000000000000000000, 1.000000000000000000 ) ) ;
#10671 = ORIENTED_EDGE ( 'NONE', *, *, #28489, .T. ) ;
#10672 = CARTESIAN_POINT ( 'NONE',  ( 0.3229289876128840775, -1.169687821100875658, 0.5631135379446852163 ) ) ;
#10673 = ORIENTED_EDGE ( 'NONE', *, *, #8244, .T. ) ;
#10674 = CARTESIAN_POINT ( 'NONE',  ( 0.3255049925932525512, -1.611144953433153448, 0.7534810049541833532 ) ) ;
#10676 = CARTESIAN_POINT ( 'NONE',  ( 0.03113248654051816583, 0.5878163732725504298, -0.2204268771689479045 ) ) ;
#10675 = DIRECTION ( 'NONE',  ( 1.000000000000000000, 2.280301054154495132E-31, -1.664003471950577689E-31 ) ) ;
#10677 = CARTESIAN_POINT ( 'NONE',  ( 0.01548846960707292615, -0.4638115001430591078, -0.2459753896938795814 ) ) ;
#10678 = CARTESIAN_POINT ( 'NONE',  ( 0.04075052232006950298, -1.520844532399347804, -0.3463593800647417065 ) ) ;
#10679 = ORIENTED_EDGE ( 'NONE', *, *, #23113, .T. ) ;
#10680 = EDGE_CURVE ( 'NONE', #23498, #1496, #28724, .T. ) ;
#10681 = CARTESIAN_POINT ( 'NONE',  ( 0.5446972779418673971, -1.168323287519652975, 0.4762509439642684250 ) ) ;
#10682 = DIRECTION ( 'NONE',  ( -1.355854680848614260E-31, 3.330669073875470114E-16, 1.000000000000000000 ) ) ;
#10683 = CARTESIAN_POINT ( 'NONE',  ( -0.1167294259372883281, -0.5331983348239499598, 0.3084771640796409864 ) ) ;
#10684 = ADVANCED_FACE ( 'NONE', ( #21634 ), #12018, .T. ) ;
#10685 = DIRECTION ( 'NONE',  ( -1.000000000000000000, -0.000000000000000000, -0.000000000000000000 ) ) ;
#10686 = AXIS2_PLACEMENT_3D ( 'NONE', #13780, #33502, #26343 ) ;
#10687 = CARTESIAN_POINT ( 'NONE',  ( 0.1170610741652670789, -0.8436375311889402484, 0.3825169963771947179 ) ) ;
#10688 = CARTESIAN_POINT ( 'NONE',  ( 0.01061034631529937829, -0.5352819679159596111, 0.1926328805739365713 ) ) ;
#10689 = AXIS2_PLACEMENT_3D ( 'NONE', #1250, #16864, #36371 ) ;
#10690 = ADVANCED_FACE ( 'NONE', ( #7136 ), #34729, .T. ) ;
#10691 = DIRECTION ( 'NONE',  ( 1.664003471950577032E-31, 3.330669073875470607E-16, 1.000000000000000000 ) ) ;
#10692 = EDGE_CURVE ( 'NONE', #12973, #27138, #32053, .T. ) ;
#10693 = EDGE_CURVE ( 'NONE', #35263, #23421, #30130, .T. ) ;
#10694 = CARTESIAN_POINT ( 'NONE',  ( 0.1999999999999789724, -2.183180860297921466, -0.4937760292030871079 ) ) ;
#10695 = CARTESIAN_POINT ( 'NONE',  ( -0.1126900943574664637, -0.5191528599708425951, 0.1528658435936960103 ) ) ;
#10696 = CARTESIAN_POINT ( 'NONE',  ( 0.6059510396320981762, -1.580958211694154292, 0.4182417262808776348 ) ) ;
#10697 = CONICAL_SURFACE ( 'NONE', #5417, 0.1762268159172233339, 0.7853981633974500554 ) ;
#10698 = CARTESIAN_POINT ( 'NONE',  ( -0.01548846960707531660, -0.09061086148575756005, -0.5171215251571035232 ) ) ;
#10699 = CARTESIAN_POINT ( 'NONE',  ( 0.2722331219925429036, -1.671874623808670135, 0.4849083929475441201 ) ) ;
#10700 = COORDINATED_UNIVERSAL_TIME_OFFSET ( 0, 0, .AHEAD. ) ;
#10701 = CARTESIAN_POINT ( 'NONE',  ( 0.06481251280142887039, -1.340178673227269801, 0.5794969380269323622 ) ) ;
#10702 = CARTESIAN_POINT ( 'NONE',  ( 0.4259907721281001036, -1.086727892038337417, -0.5155029497116575543 ) ) ;
#10703 = CARTESIAN_POINT ( 'NONE',  ( -0.1743922129835730472, -0.5166151207188712791, 0.08499999999999964528 ) ) ;
#10704 = EDGE_CURVE ( 'NONE', #1646, #32089, #37998, .T. ) ;
#10705 = CARTESIAN_POINT ( 'NONE',  ( -0.02953079040095693900, -0.09152108205202422186, -0.5223162075576424090 ) ) ;
#10706 = CARTESIAN_POINT ( 'NONE',  ( 0.3985218788515150212, -1.105145776744873798, 0.6030479543138400622 ) ) ;
#10707 = CIRCLE ( 'NONE', #13985, 0.1033070866141732880 ) ;
#10708 = CARTESIAN_POINT ( 'NONE',  ( 0.3102026568030923914, -1.754211112397273009, 0.6570273542612804496 ) ) ;
#10709 = DIRECTION ( 'NONE',  ( -7.771561172376107616E-16, 7.170354002788761615E-17, -1.000000000000000000 ) ) ;
#10710 = B_SPLINE_CURVE_WITH_KNOTS ( 'NONE', 3,
 ( #927, #9736, #7233, #26004, #32341, #28669, #35247, #4162, #31534, #38525, #25392, #22919, #3347, #29279, #1128, #34818, #15906, #28451 ),
 .UNSPECIFIED., .F., .F.,
 ( 4, 2, 2, 2, 2, 2, 2, 2, 4 ),
 ( 0.0003425652276237726654, 0.001007165397454292104, 0.001671765567284811543, 0.002336365737115330982, 0.003000965906945850421, 0.003665566076776368993, 0.004330166246606887565, 0.004994766416437405702, 0.005659366586267923840 ),
 .UNSPECIFIED. ) ;
#10711 = AXIS2_PLACEMENT_3D ( 'NONE', #3680, #10051, #28575 ) ;
#10712 = ORIENTED_EDGE ( 'NONE', *, *, #37391, .F. ) ;
#10713 = CIRCLE ( 'NONE', #33703, 1.986674066779353875 ) ;
#10714 = CARTESIAN_POINT ( 'NONE',  ( 0.1772270119712388292, -0.4894770652708761438, 0.1265226523157877703 ) ) ;
#10715 = ORIENTED_EDGE ( 'NONE', *, *, #36036, .F. ) ;
#10716 = DIRECTION ( 'NONE',  ( 4.930380657631322689E-32, 0.7472307839325097456, 0.6645646360916346307 ) ) ;
#10717 = CIRCLE ( 'NONE', #17839, 0.06250000000000001388 ) ;
#10718 = CARTESIAN_POINT ( 'NONE',  ( 0.1601225296750040661, -0.6765572740170349153, 0.4594829422558849852 ) ) ;
#10719 = VERTEX_POINT ( 'NONE', #18914 ) ;
#10720 = CIRCLE ( 'NONE', #21246, 0.2000000000000000111 ) ;
#10722 = ORIENTED_EDGE ( 'NONE', *, *, #30058, .F. ) ;
#10721 = ORIENTED_EDGE ( 'NONE', *, *, #12441, .F. ) ;
#10723 = CARTESIAN_POINT ( 'NONE',  ( 0.1220110744298638639, -0.4984167407757109647, 0.3414028199781711792 ) ) ;
#10724 = CONICAL_SURFACE ( 'NONE', #14646, 0.1400000000000013733, 1.047197551196602294 ) ;
#10725 = CARTESIAN_POINT ( 'NONE',  ( 0.1226099275768244429, -1.148810827165510862, 0.9082586858799801544 ) ) ;
#10727 = CARTESIAN_POINT ( 'NONE',  ( 0.1676546834103173622, -1.385519403818823436, 0.5281503411795812619 ) ) ;
#10726 = CARTESIAN_POINT ( 'NONE',  ( 0.02953079040094790803, 0.4684706630666300442, 0.2484463060367509413 ) ) ;
#10728 = CARTESIAN_POINT ( 'NONE',  ( 0.3595715536228106801, -1.625401886829162423, -0.3696110269036073093 ) ) ;
#10729 = COORDINATED_UNIVERSAL_TIME_OFFSET ( 0, 0, .AHEAD. ) ;
#10730 = CARTESIAN_POINT ( 'NONE',  ( 0.001778485958989725092, -0.5275076572294763455, -0.01138449076159588590 ) ) ;
#10732 = ORIENTED_EDGE ( 'NONE', *, *, #30268, .T. ) ;
#10731 = ORIENTED_EDGE ( 'NONE', *, *, #16039, .F. ) ;
#10733 = CARTESIAN_POINT ( 'NONE',  ( 0.1318732271430533010, -0.8550887030632243757, 0.4701083376385029045 ) ) ;
#10734 = EDGE_CURVE ( 'NONE', #14679, #36975, #38216, .T. ) ;
#10735 = CARTESIAN_POINT ( 'NONE',  ( 0.07151319716137326254, -0.5632038019116255567, 0.2489596798534031985 ) ) ;
#10736 = CARTESIAN_POINT ( 'NONE',  ( 0.3901811030578707373, -1.256540976566071333, 0.8456182275435326634 ) ) ;
#10737 = CARTESIAN_POINT ( 'NONE',  ( -0.02000000000000000042, -2.691615088641019504, -0.5143267481657003426 ) ) ;
#10738 = CARTESIAN_POINT ( 'NONE',  ( 0.3865586847035667462, -1.614704152518654512, 0.5182417262812423209 ) ) ;
#10739 = CARTESIAN_POINT ( 'NONE',  ( 0.6504330680646749352, -1.464154268620814880, 0.4118863462905618111 ) ) ;
#10740 = VECTOR ( 'NONE', #16978, 39.37007874015748854 ) ;
#10741 = EDGE_CURVE ( 'NONE', #2376, #10925, #34317, .T. ) ;
#10742 = CARTESIAN_POINT ( 'NONE',  ( 0.3373037064751163716, -1.749770764905459242, 0.5760335165290267900 ) ) ;
#10743 = CARTESIAN_POINT ( 'NONE',  ( 0.3995269031511867741, -1.597602329235723095, -0.3111376553386354105 ) ) ;
#10744 = ADVANCED_FACE ( 'NONE', ( #16025 ), #25489, .T. ) ;
#10745 = CARTESIAN_POINT ( 'NONE',  ( 0.06829362261317843685, -1.326848020601397504, 0.5207672198342441217 ) ) ;
#10746 = AXIS2_PLACEMENT_3D ( 'NONE', #19532, #13734, #34176 ) ;
#10747 = DIRECTION ( 'NONE',  ( 0.000000000000000000, 0.000000000000000000, -1.000000000000000000 ) ) ;
#10748 = DIRECTION ( 'NONE',  ( 0.000000000000000000, 0.000000000000000000, 1.000000000000000000 ) ) ;
#10749 = CARTESIAN_POINT ( 'NONE',  ( 0.01146630784979661005, -0.8949520681090487040, -0.009824401211993303087 ) ) ;
#10750 = CARTESIAN_POINT ( 'NONE',  ( 0.4693814222616094489, -1.280284924017013770, 0.8165702439546136393 ) ) ;
#10752 = EDGE_CURVE ( 'NONE', #356, #12111, #21859, .T. ) ;
#10751 = SHAPE_REPRESENTATION_RELATIONSHIP ( 'NONE' , 'NONE' ,  #31708, #24078 ) ;
#10753 = DIRECTION ( 'NONE',  ( 0.8660512985181130219, 0.4999551463232378978, -1.983296656985678775E-15 ) ) ;
#10754 = DIRECTION ( 'NONE',  ( 1.000000000000000000, 0.000000000000000000, 0.000000000000000000 ) ) ;
#10755 = CARTESIAN_POINT ( 'NONE',  ( 0.07582666994630285484, -1.068917391567854036, 0.8049195030047635591 ) ) ;
#10756 = CIRCLE ( 'NONE', #33736, 0.2149999999999999967 ) ;
#10757 = CARTESIAN_POINT ( 'NONE',  ( 0.4928237909781065240, -1.082648202709539431, 0.5731206881285608734 ) ) ;
#10758 = COORDINATED_UNIVERSAL_TIME_OFFSET ( 0, 0, .AHEAD. ) ;
#10759 = CARTESIAN_POINT ( 'NONE',  ( 0.3508337187165347926, -0.8535322721259723799, 0.7608596062780633718 ) ) ;
#10760 = ADVANCED_FACE ( 'NONE', ( #37606 ), #32345, .F. ) ;
#10761 = VECTOR ( 'NONE', #23708, 39.37007874015748143 ) ;
#10762 = EDGE_CURVE ( 'NONE', #6555, #23895, #9348, .T. ) ;
#10763 = EDGE_CURVE ( 'NONE', #14, #32251, #223, .T. ) ;
#10764 = CARTESIAN_POINT ( 'NONE',  ( 0.3768783096114511344, -1.720370743462839025, 0.4222122349756194382 ) ) ;
#10765 = CARTESIAN_POINT ( 'NONE',  ( 0.3061479062650170335, -1.759180248854478101, 0.5686207101516911333 ) ) ;
#10766 = ADVANCED_FACE ( 'NONE', ( #26709 ), #4462, .F. ) ;
#10767 = ORIENTED_EDGE ( 'NONE', *, *, #9716, .F. ) ;
#10768 = DIRECTION ( 'NONE',  ( 0.000000000000000000, 0.000000000000000000, 1.000000000000000000 ) ) ;
#10769 = CARTESIAN_POINT ( 'NONE',  ( 0.003257547668126477714, -0.5625981998575959597, 0.2841698052623323201 ) ) ;
#10770 = CARTESIAN_POINT ( 'NONE',  ( 0.01548846960707524721, -0.4770632572900511681, -0.2530032579707427454 ) ) ;
#10771 = ORIENTED_EDGE ( 'NONE', *, *, #5874, .T. ) ;
#10772 = CARTESIAN_POINT ( 'NONE',  ( 0.06319106323617752763, -1.336233308022867217, 0.5682657828639668951 ) ) ;
#10773 = CARTESIAN_POINT ( 'NONE',  ( 0.4107733320947055122, -0.9780847931859447675, 0.7674390821536307694 ) ) ;
#10775 = ORIENTED_EDGE ( 'NONE', *, *, #3223, .F. ) ;
#10774 = ORIENTED_EDGE ( 'NONE', *, *, #33119, .F. ) ;
#10776 = CARTESIAN_POINT ( 'NONE',  ( -1.310828011476809540E-05, -2.055032695347356331, -0.7138301564589908388 ) ) ;
#10777 = CIRCLE ( 'NONE', #39017, 0.09999999999999996392 ) ;
#10778 = VERTEX_POINT ( 'NONE', #13919 ) ;
#10779 = AXIS2_PLACEMENT_3D ( 'NONE', #5894, #33682, #8576 ) ;
#10780 = CARTESIAN_POINT ( 'NONE',  ( 0.03650577977170433447, -0.08362514765351604373, -0.5048437183011801332 ) ) ;
#10781 = PRODUCT_DEFINITION_SHAPE ( 'NONE', 'NONE',  #40651 ) ;
#10782 = LINE ( 'NONE', #23553, #20677 ) ;
#10783 = CARTESIAN_POINT ( 'NONE',  ( -0.05634490452572885749, 0.4348542811545068609, -0.1466173361067412140 ) ) ;
#10784 = ORIENTED_EDGE ( 'NONE', *, *, #2442, .F. ) ;
#10785 = CARTESIAN_POINT ( 'NONE',  ( 0.009263959265383548899, -0.5910811120922173645, 0.02017480025628250878 ) ) ;
#10786 = CARTESIAN_POINT ( 'NONE',  ( 0.1529695162128977548, -0.7869584365478802246, 0.5431710472807829149 ) ) ;
#10787 = AXIS2_PLACEMENT_3D ( 'NONE', #12264, #34464, #37344 ) ;
#10788 = CARTESIAN_POINT ( 'NONE',  ( 0.1454824607866254671, -1.106208088005755208, 0.9808573752210623109 ) ) ;
#10789 = CARTESIAN_POINT ( 'NONE',  ( 0.08551960242419305580, -0.5485164467215365436, 0.1912689294972731158 ) ) ;
#10790 = CIRCLE ( 'NONE', #20601, 0.1400000000000013178 ) ;
#10792 = DIRECTION ( 'NONE',  ( 0.8660512985181132439, 0.4999551463232374537, 0.000000000000000000 ) ) ;
#10791 = CARTESIAN_POINT ( 'NONE',  ( 0.2661871413848379553, -1.687809284679251620, 0.5876828195007447464 ) ) ;
#10793 = CARTESIAN_POINT ( 'NONE',  ( 0.1684731838197772724, -0.9467412257359250072, 0.4230012374223513505 ) ) ;
#10794 = VERTEX_POINT ( 'NONE', #23217 ) ;
#10795 = EDGE_CURVE ( 'NONE', #28660, #24301, #15941, .T. ) ;
#10796 = CARTESIAN_POINT ( 'NONE',  ( 0.3460582752528997830, -1.629311570083116889, 0.5557434574143875761 ) ) ;
#10797 = CARTESIAN_POINT ( 'NONE',  ( 0.1190390134088109841, -0.4827176764154528787, 0.3011203263016439813 ) ) ;
#10798 = EDGE_CURVE ( 'NONE', #28193, #20390, #28675, .T. ) ;
#10799 = CARTESIAN_POINT ( 'NONE',  ( -0.3000000000000000999, -1.804235510932644004, -0.05018601889714981862 ) ) ;
#10800 = CARTESIAN_POINT ( 'NONE',  ( -0.05615703521555148736, -0.4336255412628354233, -0.1517287855096114135 ) ) ;
#10801 = AXIS2_PLACEMENT_3D ( 'NONE', #13463, #13053, #6863 ) ;
#10802 = CARTESIAN_POINT ( 'NONE',  ( 0.01548846960707511190, 0.09319974324248773978, -0.5318964258758787089 ) ) ;
#10803 = CIRCLE ( 'NONE', #21333, 0.1033070866141734129 ) ;
#10804 = DIRECTION ( 'NONE',  ( 0.8660512985181130219, 0.4999551463232377868, 0.000000000000000000 ) ) ;
#10805 = CARTESIAN_POINT ( 'NONE',  ( 0.5008076730341156635, -1.117067070538257489, 0.7495569431474730093 ) ) ;
#10806 = AXIS2_PLACEMENT_3D ( 'NONE', #18049, #6090, #5698 ) ;
#10807 = CONICAL_SURFACE ( 'NONE', #40371, 0.6443128707267505861, 1.047197551196601184 ) ;
#10808 = CARTESIAN_POINT ( 'NONE',  ( -2.070754768975509474, -0.09959325338431662678, 0.3606502365330794824 ) ) ;
#10809 = CARTESIAN_POINT ( 'NONE',  ( 0.02715706672027885099, -0.9320027591207687978, 0.6014473777329288895 ) ) ;
#10810 = EDGE_CURVE ( 'NONE', #30304, #19775, #21932, .T. ) ;
#10811 = LINE ( 'NONE', #30331, #10740 ) ;
#10812 = CARTESIAN_POINT ( 'NONE',  ( 0.4807327490442517282, -1.659256856822121540, -0.6108297979790577870 ) ) ;
#10813 = CARTESIAN_POINT ( 'NONE',  ( 0.2636704545280705303, -1.001036816892615811, 0.7140474771236937634 ) ) ;
#10814 = FACE_OUTER_BOUND ( 'NONE', #33189, .T. ) ;
#10815 = CIRCLE ( 'NONE', #15424, 0.01499999999999997169 ) ;
#10816 = CARTESIAN_POINT ( 'NONE',  ( 0.5741497723391727481, -1.420869068547097269, 0.6057417262805909752 ) ) ;
#10817 =( BOUNDED_SURFACE ( )  B_SPLINE_SURFACE ( 3, 2, ( 
 ( #22795, #3830, #35497 ),
 ( #3644, #6710, #31616 ),
 ( #25462, #16594, #32211 ),
 ( #15990, #19675, #25873 ),
 ( #16206, #4240, #38187 ),
 ( #10417, #13698, #29138 ) ),
 .UNSPECIFIED., .F., .F., .F. ) 
 B_SPLINE_SURFACE_WITH_KNOTS ( ( 4, 2, 4 ),
 ( 3, 3 ),
 ( 3.903127820947815962E-18, 0.0005634672180686404065, 0.001126934436137276910 ),
 ( 0.000000000000000000, 1.000000000000000000 ),
 .UNSPECIFIED. ) 
 GEOMETRIC_REPRESENTATION_ITEM ( )  RATIONAL_B_SPLINE_SURFACE ( (
 ( 1.000000000000000000, 0.9544113358811391334, 1.000000000000000000),
 ( 1.000000000000000000, 0.9558699249329746239, 1.000000000000000000),
 ( 1.000000000000000000, 0.9497853595015035566, 1.000000000000000000),
 ( 1.000000000000000000, 0.9203877932839388265, 1.000000000000000000),
 ( 1.000000000000000000, 0.8974056080853995976, 1.000000000000000000),
 ( 1.000000000000000000, 0.8602827799847387880, 1.000000000000000000) ) ) 
 REPRESENTATION_ITEM ( '' )  SURFACE ( )  );
#10818 = CIRCLE ( 'NONE', #8745, 0.01499999999999994046 ) ;
#10819 = EDGE_LOOP ( 'NONE', ( #6934, #40583, #10211 ) ) ;
#10820 = DIRECTION ( 'NONE',  ( 0.000000000000000000, 0.000000000000000000, -1.000000000000000000 ) ) ;
#10821 = FACE_OUTER_BOUND ( 'NONE', #32913, .T. ) ;
#10822 = CARTESIAN_POINT ( 'NONE',  ( 0.3650945375302141471, -1.739603212589635461, -0.4849876925477283884 ) ) ;
#10823 = DIRECTION ( 'NONE',  ( 1.188678714063518227E-15, -1.000000000000000000, -3.263080277421930985E-16 ) ) ;
#10824 = CARTESIAN_POINT ( 'NONE',  ( 0.03202889392918464168, -0.8409986250695942189, 0.1806008807001980021 ) ) ;
#10825 = EDGE_LOOP ( 'NONE', ( #14058, #26726 ) ) ;
#10826 = CARTESIAN_POINT ( 'NONE',  ( -0.03868264068766667785, -0.2522289290439768683, -0.4043438810462546273 ) ) ;
#10827 = CYLINDRICAL_SURFACE ( 'NONE', #25011, 0.01500000000000001506 ) ;
#10828 = CARTESIAN_POINT ( 'NONE',  ( 0.4152335211599790799, -1.084324332244355205, 0.5182417262812423209 ) ) ;
#10829 = CARTESIAN_POINT ( 'NONE',  ( -2.070754768975509474, -0.09959325338431662678, 0.3750000000000004996 ) ) ;
#10830 = AXIS2_PLACEMENT_3D ( 'NONE', #33744, #8634, #27785 ) ;
#10831 = CARTESIAN_POINT ( 'NONE',  ( 0.4450023961560361507, -1.208088614032591490, 0.7033065338990315274 ) ) ;
#10833 = CARTESIAN_POINT ( 'NONE',  ( 0.01548846960707524721, 0.000000000000000000, 0.000000000000000000 ) ) ;
#10832 = CARTESIAN_POINT ( 'NONE',  ( 0.4124787977826392948, -1.129720521516186960, 0.5352010793853081427 ) ) ;
#10834 = CARTESIAN_POINT ( 'NONE',  ( 0.5795887036850762009, -1.527265703570089617, -0.4600246038137717486 ) ) ;
#10835 = VERTEX_POINT ( 'NONE', #5071 ) ;
#10836 = CIRCLE ( 'NONE', #4271, 0.04749999999977543713 ) ;
#10837 = CARTESIAN_POINT ( 'NONE',  ( 0.5046384106032315575, -1.676392394905552585, -0.5155029497116575543 ) ) ;
#10838 = VERTEX_POINT ( 'NONE', #16835 ) ;
#10839 = AXIS2_PLACEMENT_3D ( 'NONE', #21355, #34487, #31411 ) ;
#10840 = CARTESIAN_POINT ( 'NONE',  ( 0.3925301276612754298, -1.756377271995033684, -0.4843757382520948451 ) ) ;
#10841 = CONICAL_SURFACE ( 'NONE', #18707, 0.1600000000000004752, 1.047197551196598519 ) ;
#10842 = CARTESIAN_POINT ( 'NONE',  ( 0.05093431041759328981, -0.5776221905076182050, 0.2999712174261540132 ) ) ;
#10844 = CARTESIAN_POINT ( 'NONE',  ( 0.4679018147548930084, -1.094320404139347058, -0.6313355493825374420 ) ) ;
#10843 = CARTESIAN_POINT ( 'NONE',  ( 0.06891712773961738980, -0.5465723661966604974, 0.1009469152245711515 ) ) ;
#10845 = CARTESIAN_POINT ( 'NONE',  ( 0.1700813958898667599, -1.268695326050480299, 0.4882188859375907741 ) ) ;
#10846 = PRODUCT_DEFINITION_FORMATION_WITH_SPECIFIED_SOURCE ( 'ANY', '', #33451, .NOT_KNOWN. ) ;
#10847 = ORIENTED_EDGE ( 'NONE', *, *, #5721, .T. ) ;
#10848 = DIRECTION ( 'NONE',  ( 5.551115123125673617E-17, 3.263080277421931478E-16, -1.000000000000000000 ) ) ;
#10849 = CARTESIAN_POINT ( 'NONE',  ( 0.4441618370914984237, -1.292678418814498187, 0.8278337041136846208 ) ) ;
#10850 = ORIENTED_EDGE ( 'NONE', *, *, #10762, .F. ) ;
#10851 = AXIS2_PLACEMENT_3D ( 'NONE', #28111, #27500, #5681 ) ;
#10852 = FACE_OUTER_BOUND ( 'NONE', #6527, .T. ) ;
#10853 = LINE ( 'NONE', #30375, #28393 ) ;
#10854 = B_SPLINE_CURVE_WITH_KNOTS ( 'NONE', 3,
 ( #32042, #9825, #37815, #29159, #22996, #16826, #13532, #22397, #13115, #13319, #35518, #34720, #32437, #29372 ),
 .UNSPECIFIED., .F., .F.,
 ( 4, 2, 2, 2, 2, 2, 4 ),
 ( 0.002220865337158942510, 0.002866522892504111235, 0.003512180447849279526, 0.003835009225521858467, 0.004157838003194438276, 0.004480666780867017217, 0.004803495558539596158 ),
 .UNSPECIFIED. ) ;
#10855 = CARTESIAN_POINT ( 'NONE',  ( 0.1856343102545933432, -1.259872755799225086, 0.4406686558725164127 ) ) ;
#10856 = CARTESIAN_POINT ( 'NONE',  ( 0.07006815180908280982, -1.315301596572416631, 0.5080907171456734428 ) ) ;
#10857 = CARTESIAN_POINT ( 'NONE',  ( -0.2746410161513770931, -3.237612445311622622, -0.5419983935656527141 ) ) ;
#10858 = CARTESIAN_POINT ( 'NONE',  ( 0.4504805333218593333, -1.026900667268108469, 0.8467065612799143937 ) ) ;
#10859 = FACE_OUTER_BOUND ( 'NONE', #36716, .T. ) ;
#10860 = CARTESIAN_POINT ( 'NONE',  ( 0.07973371882703013391, -1.320969072382258913, 0.5669061587800955371 ) ) ;
#10861 = VECTOR ( 'NONE', #15942, 39.37007874015748143 ) ;
#10862 = CARTESIAN_POINT ( 'NONE',  ( 0.6186972872989504602, -1.565036408902899634, -0.5905337336510069202 ) ) ;
#10863 = VECTOR ( 'NONE', #26286, 39.37007874015748143 ) ;
#10864 = CARTESIAN_POINT ( 'NONE',  ( 0.01548846960707344483, 0.3688619771572954620, 0.3775276577326994176 ) ) ;
#10865 = DIRECTION ( 'NONE',  ( 0.000000000000000000, 3.414809992080316105E-15, -1.000000000000000000 ) ) ;
#10866 = CARTESIAN_POINT ( 'NONE',  ( 0.4262438152663738933, -1.592651821845863402, -0.6151431148613257793 ) ) ;
#10867 = CARTESIAN_POINT ( 'NONE',  ( -0.02000000000000000042, -1.910390638264138685, -0.7420407338378623985 ) ) ;
#10868 = LOCAL_TIME ( 0, 53, 7.000000000000000000, #725 ) ;
#10869 = CARTESIAN_POINT ( 'NONE',  ( 0.01548846960721255751, -0.07651041855108323131, 0.5222379212565277928 ) ) ;
#10870 = CARTESIAN_POINT ( 'NONE',  ( 0.6116753299763959539, -1.502912699639540550, -0.6106436555062486615 ) ) ;
#10871 = DIRECTION ( 'NONE',  ( -1.000000000000000000, 0.000000000000000000, 0.000000000000000000 ) ) ;
#10872 = LINE ( 'NONE', #29997, #25221 ) ;
#10873 = CARTESIAN_POINT ( 'NONE',  ( -0.04285561529641291473, -0.2295129201144956999, 0.4383679482630353785 ) ) ;
#10874 =( REPRESENTATION_RELATIONSHIP ('NONE','NONE', #27514, #35919 ) REPRESENTATION_RELATIONSHIP_WITH_TRANSFORMATION ( #12810 )SHAPE_REPRESENTATION_RELATIONSHIP( ) );
#10875 = TOROIDAL_SURFACE ( 'NONE', #27305, 0.04500000000000032446, 0.01499999999999999944 ) ;
#10876 = ORIENTED_EDGE ( 'NONE', *, *, #3904, .T. ) ;
#10877 = B_SPLINE_CURVE_WITH_KNOTS ( 'NONE', 3,
 ( #34926, #6731, #19308, #31850 ),
 .UNSPECIFIED., .F., .F.,
 ( 4, 4 ),
 ( 5.151976560715283563E-05, 0.0009056307464049973130 ),
 .UNSPECIFIED. ) ;
#10878 = VERTEX_POINT ( 'NONE', #10443 ) ;
#10879 = CARTESIAN_POINT ( 'NONE',  ( 0.4428400309745523233, -1.146281092196613338, -0.3830631589809550541 ) ) ;
#10880 = CARTESIAN_POINT ( 'NONE',  ( 0.3743765113291571689, -1.762474601098698024, -0.5779735398402915392 ) ) ;
#10881 = VERTEX_POINT ( 'NONE', #38623 ) ;
#10882 = CARTESIAN_POINT ( 'NONE',  ( 0.3754387176203204946, -1.765456752270669449, 0.5182417262812423209 ) ) ;
#10883 = CARTESIAN_POINT ( 'NONE',  ( 0.3445219659096331322, -1.630113034086819290, -0.4330379103484555681 ) ) ;
#10884 = CARTESIAN_POINT ( 'NONE',  ( 0.5546139119538038287, -1.386769227612277611, 0.6118514161299568599 ) ) ;
#10886 = ORIENTED_EDGE ( 'NONE', *, *, #39431, .F. ) ;
#10885 = CARTESIAN_POINT ( 'NONE',  ( -0.1574073192761738238, 0.4884966930314057487, 0.1147307106484463379 ) ) ;
#10887 = CARTESIAN_POINT ( 'NONE',  ( 0.4609105641225965111, -1.064890115380353386, 0.6919706562625183022 ) ) ;
#10888 = CARTESIAN_POINT ( 'NONE',  ( 0.01548846960707524721, 0.000000000000000000, 0.000000000000000000 ) ) ;
#10889 = EDGE_LOOP ( 'NONE', ( #40314, #984, #27024, #13140 ) ) ;
#10890 = DIRECTION ( 'NONE',  ( 0.000000000000000000, 0.000000000000000000, 1.000000000000000000 ) ) ;
#10891 = CARTESIAN_POINT ( 'NONE',  ( 0.3267929376468292069, -1.639096506223164829, 0.5708619501093183946 ) ) ;
#10893 = CARTESIAN_POINT ( 'NONE',  ( 0.1880883187714730009, -0.5243002637854453640, 0.1042455497702089173 ) ) ;
#10892 = CARTESIAN_POINT ( 'NONE',  ( 0.6579944548887032285, -1.543696042244296462, 0.4299453908671848068 ) ) ;
#10894 = CARTESIAN_POINT ( 'NONE',  ( 0.4090604450045443596, -1.131420581850358653, 0.3667417262808778666 ) ) ;
#10895 = CARTESIAN_POINT ( 'NONE',  ( 0.003504163894631640280, -1.844708889207917313, -0.3218820310881243540 ) ) ;
#10896 = ORIENTED_EDGE ( 'NONE', *, *, #12441, .T. ) ;
#10897 = CIRCLE ( 'NONE', #29307, 0.02500000000000004996 ) ;
#10898 = CARTESIAN_POINT ( 'NONE',  ( -0.2399999999999999079, -3.216935334666387813, -0.6321346234654038332 ) ) ;
#10899 = CARTESIAN_POINT ( 'NONE',  ( 9.222166083094558481E-05, -2.006822057499934697, -0.6711564558286039484 ) ) ;
#10900 = CARTESIAN_POINT ( 'NONE',  ( 0.03664605387828129279, 0.4430871221163660278, 0.1871485295462630150 ) ) ;
#10901 = EDGE_CURVE ( 'NONE', #3626, #40153, #12487, .T. ) ;
#10902 = CARTESIAN_POINT ( 'NONE',  ( 0.3754333920846802952, -1.248282022732751351, 0.6420704804048268377 ) ) ;
#10903 = APPLIED_APPROVAL_ASSIGNMENT ( #24749, ( #2357 ) ) ;
#10904 = CARTESIAN_POINT ( 'NONE',  ( 0.5891906343740130891, -1.485326646281273089, 0.6398249741016610592 ) ) ;
#10905 = APPLIED_PERSON_AND_ORGANIZATION_ASSIGNMENT ( #12910, #31828, ( #28638 ) ) ;
#10906 = CARTESIAN_POINT ( 'NONE',  ( 0.5306085078623116180, -1.660610003246502986, -0.5787814785457732203 ) ) ;
#10907 = CIRCLE ( 'NONE', #39151, 0.009999999999999998473 ) ;
#10908 = CARTESIAN_POINT ( 'NONE',  ( -0.02000000000000000042, -2.218388099582461415, -0.4932950115394270085 ) ) ;
#10909 = DIRECTION ( 'NONE',  ( 1.000000000000000000, -0.000000000000000000, -0.000000000000000000 ) ) ;
#10910 = LINE ( 'NONE', #23477, #21176 ) ;
#10911 = DIRECTION ( 'NONE',  ( 0.000000000000000000, 0.000000000000000000, -1.000000000000000000 ) ) ;
#10912 = CARTESIAN_POINT ( 'NONE',  ( 0.4368279861776801498, -1.677667223885810577, 0.4282417262809075087 ) ) ;
#10913 = CALENDAR_DATE ( 2026, 13, 10 ) ;
#10914 = CARTESIAN_POINT ( 'NONE',  ( 0.02646712690499511758, -1.095781990028246833, 0.6523102692877094100 ) ) ;
#10915 = DIRECTION ( 'NONE',  ( 0.000000000000000000, 0.000000000000000000, -1.000000000000000000 ) ) ;
#10916 = DIRECTION ( 'NONE',  ( 0.000000000000000000, 0.5550234895931941415, 0.8318346746798871427 ) ) ;
#10917 = LINE ( 'NONE', #26558, #15886 ) ;
#10918 = CARTESIAN_POINT ( 'NONE',  ( -0.2746410161513770931, -3.220869926774937664, -0.5656276768926112863 ) ) ;
#10919 = CARTESIAN_POINT ( 'NONE',  ( 0.2213055653232768594, -1.375750682257318447, 1.025040830464602815 ) ) ;
#10920 = AXIS2_PLACEMENT_3D ( 'NONE', #25938, #22435, #32085 ) ;
#10921 = FACE_OUTER_BOUND ( 'NONE', #39060, .T. ) ;
#10922 = EDGE_CURVE ( 'NONE', #31364, #16583, #17892, .T. ) ;
#10923 = ORIENTED_EDGE ( 'NONE', *, *, #4471, .F. ) ;
#10924 = EDGE_CURVE ( 'NONE', #39872, #23612, #29734, .T. ) ;
#10925 = VERTEX_POINT ( 'NONE', #32846 ) ;
#10926 = CARTESIAN_POINT ( 'NONE',  ( 0.1791081599780166012, -0.4927798373357311079, 0.1046006427271031491 ) ) ;
#10927 = ORIENTED_EDGE ( 'NONE', *, *, #31320, .F. ) ;
#10928 = LOCAL_TIME ( 0, 53, 7.000000000000000000, #3144 ) ;
#10929 = LINE ( 'NONE', #36626, #15141 ) ;
#10930 = B_SPLINE_CURVE_WITH_KNOTS ( 'NONE', 3,
 ( #1149, #19828, #10780, #23138, #10994, #7867, #26416, #4779, #4187, #17354 ),
 .UNSPECIFIED., .F., .F.,
 ( 4, 2, 2, 2, 4 ),
 ( -0.003133633995111182076, -0.002350225496333364222, -0.001566816997555546803, -0.0007834084987777293826, 8.760353553682875827E-17 ),
 .UNSPECIFIED. ) ;
#10931 = EDGE_CURVE ( 'NONE', #26041, #35420, #17929, .T. ) ;
#10932 = CARTESIAN_POINT ( 'NONE',  ( 0.6022170153251571456, -1.483150505077808878, 0.5777505789966421723 ) ) ;
#10933 = ADVANCED_FACE ( 'NONE', ( #1222 ), #29987, .T. ) ;
#10935 = VERTEX_POINT ( 'NONE', #7551 ) ;
#10934 = CARTESIAN_POINT ( 'NONE',  ( -0.001802072477946061032, -0.8317662731473794979, 0.07689373464280477299 ) ) ;
#10936 = ADVANCED_FACE ( 'NONE', ( #20128 ), #23621, .T. ) ;
#10937 = AXIS2_PLACEMENT_3D ( 'NONE', #6173, #15040, #60 ) ;
#10938 = VERTEX_POINT ( 'NONE', #11062 ) ;
#10939 = CARTESIAN_POINT ( 'NONE',  ( 0.1411908422770818405, -0.5631842745024300267, 0.4719898812008860300 ) ) ;
#10940 =( BOUNDED_SURFACE ( )  B_SPLINE_SURFACE ( 3, 2, ( 
 ( #24720, #18947, #40537 ),
 ( #18522, #25109, #40327 ),
 ( #37650, #34152, #9467 ),
 ( #6568, #22247, #22441 ),
 ( #9253, #2899, #12359 ),
 ( #18741, #21630, #31482 ) ),
 .UNSPECIFIED., .F., .F., .F. ) 
 B_SPLINE_SURFACE_WITH_KNOTS ( ( 4, 2, 4 ),
 ( 3, 3 ),
 ( -3.523657060577889411E-18, 0.0007344380730649657709, 0.001468876146129935011 ),
 ( 0.000000000000000000, 1.000000000000000000 ),
 .UNSPECIFIED. ) 
 GEOMETRIC_REPRESENTATION_ITEM ( )  RATIONAL_B_SPLINE_SURFACE ( (
 ( 1.000000000000000000, 0.8219793159978276975, 1.000000000000000000),
 ( 1.000000000000000000, 0.8695169202949302178, 1.000000000000000000),
 ( 1.000000000000000000, 0.9157158777251862558, 1.000000000000000000),
 ( 1.000000000000000000, 0.9814457743412016155, 1.000000000000000000),
 ( 1.000000000000000000, 1.000262163779300995, 1.000000000000000000),
 ( 1.000000000000000000, 1.000000000000000000, 1.000000000000000000) ) ) 
 REPRESENTATION_ITEM ( '' )  SURFACE ( )  );
#10941 = ORIENTED_EDGE ( 'NONE', *, *, #23821, .F. ) ;
#10942 = CARTESIAN_POINT ( 'NONE',  ( 0.2363740895084206761, -1.537497096284702103, 0.8974013143058253705 ) ) ;
#10944 = FACE_OUTER_BOUND ( 'NONE', #21780, .T. ) ;
#10943 = CARTESIAN_POINT ( 'NONE',  ( 0.4835349102845575842, -1.678212234975946293, -0.3866364743305659157 ) ) ;
#10945 = CARTESIAN_POINT ( 'NONE',  ( 0.4409062655693438137, -1.690090444797295977, -0.7462941026102624109 ) ) ;
#10946 = APPROVAL_STATUS ( 'not_yet_approved' ) ;
#10947 = LINE ( 'NONE', #36023, #25113 ) ;
#10949 = EDGE_LOOP ( 'NONE', ( #21003, #12426, #24899 ) ) ;
#10948 = ORIENTED_EDGE ( 'NONE', *, *, #29215, .F. ) ;
#10950 = CARTESIAN_POINT ( 'NONE',  ( 0.09328054744289671074, -0.8198616939459991704, 0.2909628914676452016 ) ) ;
#10951 = CARTESIAN_POINT ( 'NONE',  ( 0.06913471046454594537, -1.118970164930346733, 0.7557088715074291585 ) ) ;
#10952 = CARTESIAN_POINT ( 'NONE',  ( 0.1445232641043270594, -0.7452533224692177161, 0.5265950822232948747 ) ) ;
#10953 = CARTESIAN_POINT ( 'NONE',  ( 0.5536391078438838154, -1.507869940163521827, 0.6342902233424858593 ) ) ;
#10954 = CARTESIAN_POINT ( 'NONE',  ( 0.06005323737745657531, -1.257861521318574205, 0.6484451051230492036 ) ) ;
#10955 = ADVANCED_FACE ( 'NONE', ( #39430 ), #12668, .F. ) ;
#10956 = CARTESIAN_POINT ( 'NONE',  ( 0.4341912152387207291, -1.592006445115355273, -0.4177668494440743285 ) ) ;
#10957 = CARTESIAN_POINT ( 'NONE',  ( 0.5446874837152237969, -1.168306321392260649, 0.4290006342139815465 ) ) ;
#10958 = CARTESIAN_POINT ( 'NONE',  ( 0.4104061326339791815, -1.719843444618068595, -0.4250636112545012613 ) ) ;
#10959 = CARTESIAN_POINT ( 'NONE',  ( 0.3722076170955361252, -1.592376083966843714, -0.7090645075809880460 ) ) ;
#10960 = CONICAL_SURFACE ( 'NONE', #16861, 0.1400000000000004297, 1.047197551196599630 ) ;
#10961 = CARTESIAN_POINT ( 'NONE',  ( 0.06747690200237689562, -1.330070943150472917, 0.5060650602545671006 ) ) ;
#10962 = DIRECTION ( 'NONE',  ( -1.000000000000000000, -0.000000000000000000, -0.000000000000000000 ) ) ;
#10963 = DIRECTION ( 'NONE',  ( -1.000000000000000000, 0.000000000000000000, 0.000000000000000000 ) ) ;
#10964 = CARTESIAN_POINT ( 'NONE',  ( -0.0001419198701252090346, -0.8132405810867952001, -0.06941372320109172322 ) ) ;
#10965 = CARTESIAN_POINT ( 'NONE',  ( 0.5655345595830957306, -1.445718534125680410, 0.7372501758031703156 ) ) ;
#10966 = LOCAL_TIME ( 0, 53, 7.000000000000000000, #4950 ) ;
#10967 = LENGTH_MEASURE_WITH_UNIT ( LENGTH_MEASURE( 0.02539999999999999897 ), #38919 );
#10968 = CARTESIAN_POINT ( 'NONE',  ( 0.006846968701975976630, -0.8130952999835362460, 0.04930517669358801952 ) ) ;
#10969 = B_SPLINE_CURVE_WITH_KNOTS ( 'NONE', 3,
 ( #38359, #37971, #22351, #22766, #32188, #34869 ),
 .UNSPECIFIED., .F., .F.,
 ( 4, 2, 4 ),
 ( 0.0001296384739227541844, 0.002096621291417103024, 0.004063604108911452080 ),
 .UNSPECIFIED. ) ;
#10970 = CARTESIAN_POINT ( 'NONE',  ( -0.1142670043590668788, -0.4723146173917492918, 0.3382895567580816443 ) ) ;
#10971 = AXIS2_PLACEMENT_3D ( 'NONE', #15792, #38205, #10027 ) ;
#10972 = CARTESIAN_POINT ( 'NONE',  ( 0.02760435326350026836, -0.9850525496912549972, 0.6581503728771671557 ) ) ;
#10973 = CARTESIAN_POINT ( 'NONE',  ( 0.2060221519102763132, -0.8840977030479291177, 0.3560353928791143985 ) ) ;
#10974 = CALENDAR_DATE ( 2026, 13, 10 ) ;
#10975 = CARTESIAN_POINT ( 'NONE',  ( 0.2064087850599171381, -0.5517209573913892662, 0.4235422224703019323 ) ) ;
#10976 = DIRECTION ( 'NONE',  ( 0.000000000000000000, 1.000000000000000000, -1.224646799147353207E-16 ) ) ;
#10977 = CARTESIAN_POINT ( 'NONE',  ( 0.3048327051194437698, -1.756855311985219936, 0.5690458522854572321 ) ) ;
#10978 = EDGE_CURVE ( 'NONE', #31057, #37937, #22537, .T. ) ;
#10979 = ORIENTED_EDGE ( 'NONE', *, *, #12200, .F. ) ;
#10980 = CARTESIAN_POINT ( 'NONE',  ( 0.3408288395586620556, -1.672135129142385379, -0.5725068027761680556 ) ) ;
#10981 = CARTESIAN_POINT ( 'NONE',  ( 0.1023069199889618808, -1.037162491060638736, 0.8507079986674529470 ) ) ;
#10982 = EDGE_CURVE ( 'NONE', #8354, #34456, #5119, .T. ) ;
#10983 = FACE_OUTER_BOUND ( 'NONE', #4528, .T. ) ;
#10985 = VERTEX_POINT ( 'NONE', #27915 ) ;
#10984 = CARTESIAN_POINT ( 'NONE',  ( 0.3844041218437064811, -1.810736139791024435, -0.4824699277892320337 ) ) ;
#10986 = CIRCLE ( 'NONE', #5709, 0.08000000000000000167 ) ;
#10987 = CARTESIAN_POINT ( 'NONE',  ( 0.5457082879296111244, -1.652683526200752206, -0.4845594716743291119 ) ) ;
#10988 = EDGE_CURVE ( 'NONE', #36587, #19668, #22799, .T. ) ;
#10989 = CARTESIAN_POINT ( 'NONE',  ( 0.6761418372287171241, -1.395094899906518471, 0.6557117145240808354 ) ) ;
#10991 = VERTEX_POINT ( 'NONE', #8366 ) ;
#10990 = ORIENTED_EDGE ( 'NONE', *, *, #34115, .F. ) ;
#10992 = CARTESIAN_POINT ( 'NONE',  ( 0.1141769515801121238, -1.332194933707445017, -0.6802792144121206919 ) ) ;
#10993 = ORIENTED_EDGE ( 'NONE', *, *, #6921, .T. ) ;
#10994 = CARTESIAN_POINT ( 'NONE',  ( 0.04582705327698207570, -0.06484491888962944095, -0.4826014279685457153 ) ) ;
#10995 = CARTESIAN_POINT ( 'NONE',  ( -0.01548846960712804005, -0.3688619771571925998, 0.3775276577326319161 ) ) ;
#10996 = CARTESIAN_POINT ( 'NONE',  ( -0.05138886601527934556, 0.4416142869301819540, -0.1669109982970012063 ) ) ;
#10997 = ORIENTED_EDGE ( 'NONE', *, *, #5104, .T. ) ;
#10998 = DIRECTION ( 'NONE',  ( 0.8660512985181136880, 0.4999551463232368431, 0.000000000000000000 ) ) ;
#10999 = CARTESIAN_POINT ( 'NONE',  ( 0.08878836246962278078, -0.6867776948031327766, 0.2056562767453794516 ) ) ;
#11000 = CARTESIAN_POINT ( 'NONE',  ( 0.2852911188406123122, -1.556753723687055224, 0.9829980583461535026 ) ) ;
#11001 = CARTESIAN_POINT ( 'NONE',  ( 0.09766204791072935487, -0.5457031429471165263, 0.1623845927645223841 ) ) ;
#11003 = CARTESIAN_POINT ( 'NONE',  ( 0.3116047323306956884, -1.649437158552430338, 0.5948350866965763650 ) ) ;
#11002 = CARTESIAN_POINT ( 'NONE',  ( 0.2650451966282841298, -1.687516040838051845, 0.5730406266932795978 ) ) ;
#11004 = ADVANCED_FACE ( 'NONE', ( #11855 ), #3461, .T. ) ;
#11005 = CARTESIAN_POINT ( 'NONE',  ( 0.04706940247297254631, -0.9403352153122209733, 0.1954608171380558534 ) ) ;
#11006 = ORIENTED_EDGE ( 'NONE', *, *, #21937, .T. ) ;
#11007 = DIRECTION ( 'NONE',  ( 1.000000000000000000, 2.341930812374887555E-31, -1.664003471950578127E-31 ) ) ;
#11008 = B_SPLINE_CURVE_WITH_KNOTS ( 'NONE', 3,
 ( #30115, #1946, #36691, #33808 ),
 .UNSPECIFIED., .F., .F.,
 ( 4, 4 ),
 ( 0.0006408076469776195555, 0.0007877951202762262500 ),
 .UNSPECIFIED. ) ;
#11009 = ADVANCED_FACE ( 'NONE', ( #27506 ), #17170, .T. ) ;
#11010 = CARTESIAN_POINT ( 'NONE',  ( 0.2178843723336029436, -0.5744936670103212295, 0.4629775832872777830 ) ) ;
#11011 = B_SPLINE_CURVE_WITH_KNOTS ( 'NONE', 3,
 ( #19794, #23105, #22911, #3947 ),
 .UNSPECIFIED., .F., .F.,
 ( 4, 4 ),
 ( 0.000000000000000000, 0.0004498717961012255943 ),
 .UNSPECIFIED. ) ;
#11012 = DIRECTION ( 'NONE',  ( -0.8400989100995858161, 0.000000000000000000, 0.5424332412836514461 ) ) ;
#11013 = CARTESIAN_POINT ( 'NONE',  ( -0.05491348488830681551, -0.4472107100395448231, -0.1187682108873645004 ) ) ;
#11014 = DIRECTION ( 'NONE',  ( 0.000000000000000000, 6.829619984160658243E-15, -1.000000000000000000 ) ) ;
#11015 = CARTESIAN_POINT ( 'NONE',  ( -0.2399999999999999079, -3.941790907013290823, -0.4709369376873030477 ) ) ;
#11016 = CARTESIAN_POINT ( 'NONE',  ( 0.1909052096321314784, -0.5854118129141068216, 0.1777712087850742972 ) ) ;
#11017 = DIRECTION ( 'NONE',  ( 1.000000000000000000, 0.000000000000000000, 7.847494366974321282E-16 ) ) ;
#11018 = CARTESIAN_POINT ( 'NONE',  ( 0.05999999999999990757, 0.4783370154475735103, 0.2940679337375869951 ) ) ;
#11019 = CARTESIAN_POINT ( 'NONE',  ( 0.3297273269827796782, -1.292423171921244895, 0.4805102893914065532 ) ) ;
#11020 = FACE_OUTER_BOUND ( 'NONE', #29635, .T. ) ;
#11021 = CARTESIAN_POINT ( 'NONE',  ( 0.02953079040095728247, 0.000000000000000000, 0.000000000000000000 ) ) ;
#11022 = AXIS2_PLACEMENT_3D ( 'NONE', #20202, #4346, #38899 ) ;
#11023 = CARTESIAN_POINT ( 'NONE',  ( -0.04047076529492847630, -0.2415772653364916533, -0.4392125161515710863 ) ) ;
#11024 = ORIENTED_EDGE ( 'NONE', *, *, #14163, .F. ) ;
#11025 = CARTESIAN_POINT ( 'NONE',  ( 0.4640588441595929203, -1.068323083224587577, 0.7162715700772641636 ) ) ;
#11026 = LINE ( 'NONE', #33011, #33122 ) ;
#11027 = EDGE_CURVE ( 'NONE', #30248, #23130, #6083, .T. ) ;
#11028 = CARTESIAN_POINT ( 'NONE',  ( 0.4139226612333222199, -1.128928040977267511, 0.5474757255584167259 ) ) ;
#11029 = CARTESIAN_POINT ( 'NONE',  ( 0.2774637254902345140, -1.318135075689816249, 0.6011524605781312092 ) ) ;
#11030 = VERTEX_POINT ( 'NONE', #16570 ) ;
#11031 = CARTESIAN_POINT ( 'NONE',  ( 0.03309057659885129149, 0.2303206601891112093, 0.4671007096900143818 ) ) ;
#11032 = CARTESIAN_POINT ( 'NONE',  ( -0.02953079040095652960, 0.2329676531120518090, 0.4763574306556300764 ) ) ;
#11033 = CARTESIAN_POINT ( 'NONE',  ( 0.3703394740834939913, -1.759797141953248323, -0.4296865123946668197 ) ) ;
#11034 = CARTESIAN_POINT ( 'NONE',  ( 2.189050353664013844E-15, -0.2949999999999994849, -0.06434668806854183798 ) ) ;
#11035 = CARTESIAN_POINT ( 'NONE',  ( 0.3647626819780801499, -1.106519030682488802, 0.7096260846467223882 ) ) ;
#11037 = CARTESIAN_POINT ( 'NONE',  ( 0.5670576198622274688, -1.627347961110953367, 0.5260709129414246066 ) ) ;
#11036 = CARTESIAN_POINT ( 'NONE',  ( 0.1999999999999789724, -2.183180860297921466, -0.4937760292030871079 ) ) ;
#11038 = CARTESIAN_POINT ( 'NONE',  ( 0.5816799176160351026, -1.521122139812363550, -0.5782616316121675926 ) ) ;
#11039 = ORIENTED_EDGE ( 'NONE', *, *, #8139, .F. ) ;
#11040 = B_SPLINE_CURVE_WITH_KNOTS ( 'NONE', 3,
 ( #3901, #38057, #34578, #13583 ),
 .UNSPECIFIED., .F., .F.,
 ( 4, 4 ),
 ( 0.000000000000000000, 0.0002767576745124534663 ),
 .UNSPECIFIED. ) ;
#11041 = CARTESIAN_POINT ( 'NONE',  ( 0.1759300380180284507, -1.231083256582695684, -0.4125659523519146221 ) ) ;
#11042 = ORIENTED_EDGE ( 'NONE', *, *, #6180, .F. ) ;
#11043 = DIRECTION ( 'NONE',  ( 1.000000000000000000, -0.000000000000000000, -0.000000000000000000 ) ) ;
#11044 = CARTESIAN_POINT ( 'NONE',  ( 0.4083779858257735040, -1.563267192213793511, 0.7363480300735880668 ) ) ;
#11046 = CARTESIAN_POINT ( 'NONE',  ( 0.03113248654051816583, 0.3931478764542372661, 0.2416960844521746365 ) ) ;
#11045 = CARTESIAN_POINT ( 'NONE',  ( 0.08836802265519826116, -0.6144346768691744121, 0.02127763492959088010 ) ) ;
#11047 = CARTESIAN_POINT ( 'NONE',  ( 0.5338352526116463270, -1.174566725300919989, -0.4248180574663139586 ) ) ;
#11048 = ADVANCED_FACE ( 'NONE', ( #30489 ), #7496, .T. ) ;
#11049 = ORIENTED_EDGE ( 'NONE', *, *, #23932, .F. ) ;
#11050 = EDGE_CURVE ( 'NONE', #10402, #14366, #19905, .T. ) ;
#11051 = CYLINDRICAL_SURFACE ( 'NONE', #12284, 0.1000000000000000194 ) ;
#11052 = CARTESIAN_POINT ( 'NONE',  ( 0.2359862434256725650, -0.8906993715589636151, 0.6977976417879780957 ) ) ;
#11053 = CIRCLE ( 'NONE', #36676, 0.08000000000000002942 ) ;
#11054 = ORIENTED_EDGE ( 'NONE', *, *, #25802, .T. ) ;
#11055 = DIRECTION ( 'NONE',  ( 1.000000000000000000, 7.857794173099924470E-32, 8.628166150854818811E-32 ) ) ;
#11056 = CARTESIAN_POINT ( 'NONE',  ( 0.04047043078436388108, -0.4923670751789738786, 0.09403524049742623125 ) ) ;
#11057 = CARTESIAN_POINT ( 'NONE',  ( 0.3848779947554198944, -1.747748222921210903, -0.4374302019815166642 ) ) ;
#11058 = CARTESIAN_POINT ( 'NONE',  ( 0.1806433941755341832, -1.251233634640312120, 0.4406669043849698597 ) ) ;
#11059 = CARTESIAN_POINT ( 'NONE',  ( 0.3925301276612723211, -1.756377271995031020, -0.4843757382520817445 ) ) ;
#11060 = CARTESIAN_POINT ( 'NONE',  ( 0.6638964227572436982, -1.375154404986101531, 0.8002223753517787586 ) ) ;
#11061 = CYLINDRICAL_SURFACE ( 'NONE', #11557, 0.1249999999999999584 ) ;
#11062 = CARTESIAN_POINT ( 'NONE',  ( 2.988985998443356465E-16, -0.05999999999999977573, 0.2000000000000000389 ) ) ;
#11063 = CARTESIAN_POINT ( 'NONE',  ( 0.5747947170275361506, -1.612684560496418174, -0.5055484516149173491 ) ) ;
#11064 = CARTESIAN_POINT ( 'NONE',  ( 0.02953079040095494406, 0.3810518745593893808, 0.3687679460475793425 ) ) ;
#11065 = DIRECTION ( 'NONE',  ( -1.387778780781449423E-15, 6.460451336368206514E-16, -1.000000000000000000 ) ) ;
#11066 = CARTESIAN_POINT ( 'NONE',  ( 0.01895494625228227870, 0.3623053290766983792, -0.3730957266516553017 ) ) ;
#11067 = CARTESIAN_POINT ( 'NONE',  ( 0.002083146443013456344, -0.4777046557262296100, 0.09357736723029726200 ) ) ;
#11068 = CARTESIAN_POINT ( 'NONE',  ( 0.5945517648669413902, -1.497934605890146154, -0.6409792228890591748 ) ) ;
#11069 = CARTESIAN_POINT ( 'NONE',  ( 0.4226000438817392180, -1.709616762427842218, 0.4282184315516496809 ) ) ;
#11070 = ADVANCED_FACE ( 'NONE', ( #38759 ), #33997, .T. ) ;
#11071 = CARTESIAN_POINT ( 'NONE',  ( 0.5975349495741208994, -1.597363011650178688, 0.4182417262808776903 ) ) ;
#11072 = CARTESIAN_POINT ( 'NONE',  ( -0.04308449196698653505, -0.3346410801914496691, 0.3638139224395113280 ) ) ;
#11073 = ORIENTED_EDGE ( 'NONE', *, *, #34328, .T. ) ;
#11074 = B_SPLINE_CURVE_WITH_KNOTS ( 'NONE', 3,
 ( #35702, #7719, #20285, #1574, #4607, #20086, #17183, #14097, #26670, #23174 ),
 .UNSPECIFIED., .F., .F.,
 ( 4, 2, 2, 2, 4 ),
 ( 1.080346398583096594E-17, 0.0007746574062662946875, 0.001549314812532578750, 0.002323972218798862812, 0.003098629625065147525 ),
 .UNSPECIFIED. ) ;
#11075 = ORIENTED_EDGE ( 'NONE', *, *, #10499, .T. ) ;
#11076 = CARTESIAN_POINT ( 'NONE',  ( 0.6540709664215760277, -1.593060928864740156, 0.5182417262812423209 ) ) ;
#11077 = CARTESIAN_POINT ( 'NONE',  ( 0.3208715077212234701, -1.182672892261233732, 0.4687417262808780127 ) ) ;
#11078 = EDGE_LOOP ( 'NONE', ( #3593, #18357 ) ) ;
#11079 = FACE_OUTER_BOUND ( 'NONE', #18899, .T. ) ;
#11080 = CARTESIAN_POINT ( 'NONE',  ( 0.6229690016365089233, -1.526593058827372174, -0.3991335894808961116 ) ) ;
#11081 = CARTESIAN_POINT ( 'NONE',  ( 0.5095464092883764673, -1.311269877878546763, 0.7328776202162170517 ) ) ;
#11083 = ORIENTED_EDGE ( 'NONE', *, *, #4642, .T. ) ;
#11082 = CARTESIAN_POINT ( 'NONE',  ( -0.1595531559346400341, 0.4954596757340542501, 0.1197284696570148632 ) ) ;
#11084 = CARTESIAN_POINT ( 'NONE',  ( 0.2122887247597850247, -0.8188226314918697346, 0.3927370908608381339 ) ) ;
#11085 = FACE_OUTER_BOUND ( 'NONE', #20498, .T. ) ;
#11086 = ORIENTED_EDGE ( 'NONE', *, *, #32300, .F. ) ;
#11087 = DIRECTION ( 'NONE',  ( 0.000000000000000000, 0.000000000000000000, -1.000000000000000000 ) ) ;
#11088 = ORIENTED_EDGE ( 'NONE', *, *, #14788, .F. ) ;
#11089 = CARTESIAN_POINT ( 'NONE',  ( 0.02322197787115687709, -0.5342335529176228670, 0.1743862541488195861 ) ) ;
#11091 = CARTESIAN_POINT ( 'NONE',  ( 0.1764183673576233957, -0.5463805283139606672, -0.03610222269428862291 ) ) ;
#11090 = CARTESIAN_POINT ( 'NONE',  ( 0.7077821646032427250, -1.503511044123807316, 0.5489718279396991196 ) ) ;
#11092 = CARTESIAN_POINT ( 'NONE',  ( 0.2319960710055803677, -1.232736008543062090, 0.4687417262808780127 ) ) ;
#11093 = CARTESIAN_POINT ( 'NONE',  ( 0.3699999999999783462, -2.120664306612686012, -0.5256090310107919272 ) ) ;
#11094 = EDGE_LOOP ( 'NONE', ( #32919, #30811, #32205, #33081 ) ) ;
#11095 = DIRECTION ( 'NONE',  ( 1.000000000000000000, -0.000000000000000000, -0.000000000000000000 ) ) ;
#11096 = CARTESIAN_POINT ( 'NONE',  ( 0.1598324831679015234, -1.276895193453223776, 0.4182417262808777458 ) ) ;
#11097 = CARTESIAN_POINT ( 'NONE',  ( 0.03868264068766623376, 0.4624969084406955200, 0.1149348357506039670 ) ) ;
#11098 = CARTESIAN_POINT ( 'NONE',  ( 0.3313744226343967036, -1.290158028341789276, 0.5896145059446814551 ) ) ;
#11099 = CARTESIAN_POINT ( 'NONE',  ( 0.09537675404226049480, -1.364128109777166475, -0.3613912495262363023 ) ) ;
#11100 = EDGE_CURVE ( 'NONE', #5197, #12681, #36026, .T. ) ;
#11101 = CARTESIAN_POINT ( 'NONE',  ( -0.1533385355407297923, 0.4750492940987078860, 0.3599999999999995981 ) ) ;
#11102 = B_SPLINE_CURVE_WITH_KNOTS ( 'NONE', 3,
 ( #21336, #8759, #24024, #14741 ),
 .UNSPECIFIED., .F., .F.,
 ( 4, 4 ),
 ( 0.005101096601136854980, 0.009027368544441125020 ),
 .UNSPECIFIED. ) ;
#11103 = CARTESIAN_POINT ( 'NONE',  ( 0.3965913301904470112, -1.111811593118468666, 0.6217369508112339238 ) ) ;
#11104 = CARTESIAN_POINT ( 'NONE',  ( -0.1167294258595701767, -0.5331983345537089081, 0.1478951491071181235 ) ) ;
#11105 = CARTESIAN_POINT ( 'NONE',  ( 0.01548846960707524721, 0.000000000000000000, 0.000000000000000000 ) ) ;
#11106 = LINE ( 'NONE', #33105, #25334 ) ;
#11107 = DIRECTION ( 'NONE',  ( -1.000000000000000000, -7.857794173099924470E-32, -8.628166150854818811E-32 ) ) ;
#11108 = APPROVAL_ROLE ( '' ) ;
#11109 = CARTESIAN_POINT ( 'NONE',  ( 0.4186431762316955019, -1.143068542649264163, 0.4275947501741096946 ) ) ;
#11110 = CARTESIAN_POINT ( 'NONE',  ( 0.1770675091758397157, -0.4892248890959581820, 0.1433326821102208493 ) ) ;
#11111 = APPLICATION_CONTEXT ( 'configuration controlled 3d designs of mechanical parts and assemblies' ) ;
#11112 = CARTESIAN_POINT ( 'NONE',  ( -0.2746410161513776482, -3.880844374714816247, -0.2860650318788287017 ) ) ;
#11113 = CARTESIAN_POINT ( 'NONE',  ( 0.01212774845371318924, -0.4356706518047467891, 0.08239804974011019634 ) ) ;
#11114 = CARTESIAN_POINT ( 'NONE',  ( 0.3986312341787107694, -2.053945766513980864, -0.5118724213368843756 ) ) ;
#11115 = CARTESIAN_POINT ( 'NONE',  ( 0.1352158960584371739, -1.069175309996540202, 0.9661058881916898544 ) ) ;
#11116 = CARTESIAN_POINT ( 'NONE',  ( 0.01548846960707528191, 0.2372406987223596164, -0.4850946823762614102 ) ) ;
#11117 = ORIENTED_EDGE ( 'NONE', *, *, #19080, .F. ) ;
#11118 = ORIENTED_EDGE ( 'NONE', *, *, #17176, .T. ) ;
#11119 = CARTESIAN_POINT ( 'NONE',  ( 0.07216878364870311924, 0.08000000000000023759, 0.1249999999999999029 ) ) ;
#11120 = EDGE_LOOP ( 'NONE', ( #12339, #15232, #7240, #14315 ) ) ;
#11121 = CARTESIAN_POINT ( 'NONE',  ( 0.4670757733960571034, -1.683842906665585337, -0.4131506686299025732 ) ) ;
#11123 = ORIENTED_EDGE ( 'NONE', *, *, #5874, .F. ) ;
#11122 = CARTESIAN_POINT ( 'NONE',  ( 0.1344413119357726061, -0.5591674697507452718, 0.1973459964408592893 ) ) ;
#11125 = ORIENTED_EDGE ( 'NONE', *, *, #20791, .F. ) ;
#11124 = CARTESIAN_POINT ( 'NONE',  ( 0.008064696880236928156, -0.7084159389384210304, -0.01121069830473241102 ) ) ;
#11126 = EDGE_LOOP ( 'NONE', ( #28397, #2615, #34707, #23424 ) ) ;
#11127 = CARTESIAN_POINT ( 'NONE',  ( 0.1175045378272833174, -0.4723384530406989912, 0.2724513898149077962 ) ) ;
#11128 = EDGE_LOOP ( 'NONE', ( #36596, #14043, #27018, #29708, #2278, #34838, #12622, #27395 ) ) ;
#11129 = CARTESIAN_POINT ( 'NONE',  ( 0.2573325307069851409, -1.608293788183657869, 0.8328901382586275659 ) ) ;
#11131 = CARTESIAN_POINT ( 'NONE',  ( 0.2101924623511064461, -1.233948830739026503, 0.5631135211526988593 ) ) ;
#11130 = DIRECTION ( 'NONE',  ( -1.000000000000000000, -0.000000000000000000, -0.000000000000000000 ) ) ;
#11132 = CARTESIAN_POINT ( 'NONE',  ( 0.1499999999999993561, 0.000000000000000000, 0.000000000000000000 ) ) ;
#11133 = APPROVAL_STATUS ( 'not_yet_approved' ) ;
#11134 = CARTESIAN_POINT ( 'NONE',  ( 0.2009282062366657129, -1.274386533297698909, -0.7137155460508515237 ) ) ;
#11136 = ORIENTED_EDGE ( 'NONE', *, *, #32611, .T. ) ;
#11135 = EDGE_LOOP ( 'NONE', ( #3480, #30869, #34920, #84, #28329 ) ) ;
#11137 = CARTESIAN_POINT ( 'NONE',  ( 0.2120815815383247649, -1.521234644788605150, -0.3529678530972831796 ) ) ;
#11138 = CARTESIAN_POINT ( 'NONE',  ( 0.08480723791494081121, -1.210854647815037932, 0.7609210295126361823 ) ) ;
#11139 = CARTESIAN_POINT ( 'NONE',  ( 0.1531589382160408741, -0.7640739595342987966, 0.5488755516528662781 ) ) ;
#11140 = CARTESIAN_POINT ( 'NONE',  ( 0.5530210029615032497, -1.511195326521239224, 0.5738729771428068283 ) ) ;
#11141 = DIRECTION ( 'NONE',  ( -1.000000000000000000, -0.000000000000000000, -0.000000000000000000 ) ) ;
#11142 = CARTESIAN_POINT ( 'NONE',  ( 0.6030593677082874970, -1.482073155342621851, 0.6044986214589193052 ) ) ;
#11143 = CARTESIAN_POINT ( 'NONE',  ( 0.1994740068363786423, -2.042640899752901085, -0.2765909798240093198 ) ) ;
#11144 = CARTESIAN_POINT ( 'NONE',  ( -0.3000000000000000999, -2.322955634169589612, -0.9336221289765171960 ) ) ;
#11145 = CARTESIAN_POINT ( 'NONE',  ( 0.6983789749627276056, -1.438823976843206509, 0.5652110266803307415 ) ) ;
#11146 = EDGE_CURVE ( 'NONE', #34108, #13144, #21842, .T. ) ;
#11147 = DIRECTION ( 'NONE',  ( 1.000000000000000000, 2.280301054154495132E-31, -1.664003471950577689E-31 ) ) ;
#11148 = EDGE_CURVE ( 'NONE', #34957, #3966, #21891, .T. ) ;
#11149 = FACE_BOUND ( 'NONE', #31119, .T. ) ;
#11150 = LINE ( 'NONE', #26389, #10761 ) ;
#11151 = CARTESIAN_POINT ( 'NONE',  ( 0.4075835738538290398, -1.123965384694001868, 0.6035659867371363507 ) ) ;
#11152 = CARTESIAN_POINT ( 'NONE',  ( 0.3279590963379148683, -1.123159558159656957, 0.5182417262812423209 ) ) ;
#11153 = ADVANCED_FACE ( 'NONE', ( #33111 ), #8703, .F. ) ;
#11154 = FACE_OUTER_BOUND ( 'NONE', #28594, .T. ) ;
#11155 = EDGE_CURVE ( 'NONE', #28743, #21660, #2175, .T. ) ;
#11156 = CARTESIAN_POINT ( 'NONE',  ( 0.004343411016521666126, -0.7362306918419727619, 0.3916307744012189618 ) ) ;
#11157 = CARTESIAN_POINT ( 'NONE',  ( 0.4928690250500026293, -1.082673021089655574, 0.5721439028494731405 ) ) ;
#11158 = APPROVAL_ROLE ( '' ) ;
#11159 = CARTESIAN_POINT ( 'NONE',  ( 0.2723301224276278298, -0.7044396210649886969, 0.6356112240561296867 ) ) ;
#11160 = DIRECTION ( 'NONE',  ( -1.000000000000000000, -0.000000000000000000, -0.000000000000000000 ) ) ;
#11161 = CARTESIAN_POINT ( 'NONE',  ( -2.070754768975509919, -0.09959325338431655739, 0.1000000000000005745 ) ) ;
#11162 =( BOUNDED_SURFACE ( )  B_SPLINE_SURFACE ( 3, 2, ( 
 ( #28400, #27588, #12158 ),
 ( #40114, #2690, #37251 ),
 ( #24916, #11945, #12553 ),
 ( #37443, #24508, #18126 ) ),
 .UNSPECIFIED., .F., .F., .F. ) 
 B_SPLINE_SURFACE_WITH_KNOTS ( ( 4, 4 ),
 ( 3, 3 ),
 ( 2.764715539838036307E-18, 0.001173839118112707421 ),
 ( 0.000000000000000000, 1.000000000000000000 ),
 .UNSPECIFIED. ) 
 GEOMETRIC_REPRESENTATION_ITEM ( )  RATIONAL_B_SPLINE_SURFACE ( (
 ( 1.000000000000000000, 0.9157534740979349497, 1.000000000000000000),
 ( 1.000000000000000000, 0.9253442540293808083, 1.000000000000000000),
 ( 1.000000000000000000, 0.9341318845569276386, 1.000000000000000000),
 ( 1.000000000000000000, 0.9411999499705258065, 1.000000000000000000) ) ) 
 REPRESENTATION_ITEM ( '' )  SURFACE ( )  );
#11163 = EDGE_CURVE ( 'NONE', #26173, #7249, #36545, .T. ) ;
#11164 = ORIENTED_EDGE ( 'NONE', *, *, #38802, .F. ) ;
#11165 = CARTESIAN_POINT ( 'NONE',  ( 0.3487950145890576503, -1.709514507286181262, -0.5484001082352915057 ) ) ;
#11166 = PRODUCT_DEFINITION ( 'UNKNOWN', '', #10846, #4325 ) ;
#11167 = CARTESIAN_POINT ( 'NONE',  ( 0.1740866738651369872, -1.306816224518804415, 0.9481330771635244625 ) ) ;
#11168 = CARTESIAN_POINT ( 'NONE',  ( 0.1099539500251690283, -1.292169261604334540, 0.4406931972238851691 ) ) ;
#11170 = VERTEX_POINT ( 'NONE', #38873 ) ;
#11169 = CARTESIAN_POINT ( 'NONE',  ( 0.3853448888748426393, -1.884999421977940015, -0.5123789408289101122 ) ) ;
#11171 = CARTESIAN_POINT ( 'NONE',  ( 0.1202595235781068889, 0.06028806207340008799, -0.04170439506869255686 ) ) ;
#11172 = CARTESIAN_POINT ( 'NONE',  ( 0.1906247196645202702, -0.5843772811062371009, 0.1457185332388696020 ) ) ;
#11174 = ORIENTED_EDGE ( 'NONE', *, *, #21854, .F. ) ;
#11173 = ORIENTED_EDGE ( 'NONE', *, *, #17292, .F. ) ;
#11175 = CARTESIAN_POINT ( 'NONE',  ( 0.003157895387556955251, -1.847058397352856485, -0.6456400114880085361 ) ) ;
#11176 = CARTESIAN_POINT ( 'NONE',  ( -0.02000000000000000042, -2.039246558356380135, -0.5681570558249129377 ) ) ;
#11177 = DIRECTION ( 'NONE',  ( 0.9591734532964090176, 0.2828184691483947022, -5.691349986800532102E-16 ) ) ;
#11178 = DATE_AND_TIME ( #39360, #34534 ) ;
#11179 = AXIS2_PLACEMENT_3D ( 'NONE', #25088, #18104, #18308 ) ;
#11180 = CARTESIAN_POINT ( 'NONE',  ( -0.03474824846560887331, 0.5087747035359508896, -0.08925086559848302570 ) ) ;
#11181 = ORIENTED_EDGE ( 'NONE', *, *, #34424, .T. ) ;
#11182 = CARTESIAN_POINT ( 'NONE',  ( 0.3572222731481287661, -1.622781385286526934, -0.3671481750039431446 ) ) ;
#11183 = CARTESIAN_POINT ( 'NONE',  ( 0.08952804818007449594, -0.6881766246006204568, 0.2235799437253089272 ) ) ;
#11184 = CARTESIAN_POINT ( 'NONE',  ( 0.2100130340724439826, -1.285393126011718623, 1.028891139539269250 ) ) ;
#11185 = CIRCLE ( 'NONE', #34174, 0.01000000000000001582 ) ;
#11186 = CARTESIAN_POINT ( 'NONE',  ( 0.4978489536914548208, -1.542573269935797686, 0.5796211865037168565 ) ) ;
#11188 = FACE_OUTER_BOUND ( 'NONE', #3039, .T. ) ;
#11187 = CARTESIAN_POINT ( 'NONE',  ( 0.1953104519840635767, -1.377916898911103472, 0.9490300120740665646 ) ) ;
#11189 = CARTESIAN_POINT ( 'NONE',  ( 0.2751433273660585099, -1.204544342693914860, 0.5922316713047012238 ) ) ;
#11190 = ORIENTED_EDGE ( 'NONE', *, *, #20978, .T. ) ;
#11191 = EDGE_LOOP ( 'NONE', ( #26132, #11073 ) ) ;
#11192 = CARTESIAN_POINT ( 'NONE',  ( -0.1643313925802001585, 0.5105373599712219601, 0.1162626052509345420 ) ) ;
#11193 = CARTESIAN_POINT ( 'NONE',  ( 0.2048162548087716639, -0.6103794925887051637, 0.3711584868840494544 ) ) ;
#11194 = CARTESIAN_POINT ( 'NONE',  ( -0.08000000000000000167, -2.379949255320110257, -0.6346823614705312533 ) ) ;
#11195 = ADVANCED_FACE ( 'NONE', ( #23274 ), #14589, .F. ) ;
#11196 = CARTESIAN_POINT ( 'NONE',  ( 0.4584717390208091770, -1.703043547193807017, -0.5155029497116575543 ) ) ;
#11197 = EDGE_CURVE ( 'NONE', #23884, #35323, #38274, .T. ) ;
#11198 = DIRECTION ( 'NONE',  ( -1.000000000000000000, -0.000000000000000000, -0.000000000000000000 ) ) ;
#11199 = CARTESIAN_POINT ( 'NONE',  ( 0.3948319565448157875, -1.761998452218138445, -0.7106721340409676291 ) ) ;
#11200 = EDGE_CURVE ( 'NONE', #25557, #23099, #9380, .T. ) ;
#11201 = DIRECTION ( 'NONE',  ( 1.000000000000000000, 6.779273404243070203E-32, 4.314083075427408311E-32 ) ) ;
#11202 = CARTESIAN_POINT ( 'NONE',  ( 0.3578995607061009054, -0.9255625346965836719, 0.6844156867609741957 ) ) ;
#11203 = DIRECTION ( 'NONE',  ( 0.000000000000000000, 0.000000000000000000, -1.000000000000000000 ) ) ;
#11204 = AXIS2_PLACEMENT_3D ( 'NONE', #27670, #15326, #1976 ) ;
#11205 = CARTESIAN_POINT ( 'NONE',  ( 0.03171861681797973065, 0.5171399723077767518, -0.08825220573713646322 ) ) ;
#11206 = ORIENTED_EDGE ( 'NONE', *, *, #33015, .F. ) ;
#11207 = SPHERICAL_SURFACE ( 'NONE', #18189, 0.01499999999999999944 ) ;
#11208 = CARTESIAN_POINT ( 'NONE',  ( 0.000000000000000000, -0.02999999999999995379, 0.000000000000000000 ) ) ;
#11209 = CARTESIAN_POINT ( 'NONE',  ( -0.05491348488830606611, -0.2919908616877284202, -0.3589493610278738922 ) ) ;
#11210 = EDGE_CURVE ( 'NONE', #17083, #33728, #33019, .T. ) ;
#11211 = ORIENTED_EDGE ( 'NONE', *, *, #32880, .F. ) ;
#11212 = CARTESIAN_POINT ( 'NONE',  ( 0.3510880644213571489, -0.9448783719387029434, 0.6508378404258201577 ) ) ;
#11213 = VECTOR ( 'NONE', #34709, 39.37007874015748143 ) ;
#11214 = CARTESIAN_POINT ( 'NONE',  ( 0.3979671137871990116, -1.137957823998669848, 0.4904217454224647499 ) ) ;
#11215 = CARTESIAN_POINT ( 'NONE',  ( 0.1897997141002692179, -1.273939956134424234, 0.7173303927998203600 ) ) ;
#11216 = VERTEX_POINT ( 'NONE', #11112 ) ;
#11217 = CARTESIAN_POINT ( 'NONE',  ( -0.03159140494780109804, 0.2432984029592196173, 0.4277399113045149415 ) ) ;
#11218 = CARTESIAN_POINT ( 'NONE',  ( 0.4165782488800118810, -1.609873178559232176, -0.3634132145561362326 ) ) ;
#11219 = CARTESIAN_POINT ( 'NONE',  ( 0.01899496522503167292, -0.5123200228845833371, -0.08888615261743730567 ) ) ;
#11220 = DIRECTION ( 'NONE',  ( -1.000000000000000000, -0.000000000000000000, -0.000000000000000000 ) ) ;
#11221 = CARTESIAN_POINT ( 'NONE',  ( 0.4684633558679283660, -1.238878407153067851, 0.5960060519205929719 ) ) ;
#11223 = DIRECTION ( 'NONE',  ( 1.000000000000000000, 0.000000000000000000, 8.537024980200777445E-16 ) ) ;
#11222 = DIRECTION ( 'NONE',  ( -1.000000000000000000, 0.000000000000000000, -7.847494366974319310E-16 ) ) ;
#11224 = CARTESIAN_POINT ( 'NONE',  ( 0.2296032268162506162, -0.9382281285954664485, 0.4302797228108481420 ) ) ;
#11225 = ORIENTED_EDGE ( 'NONE', *, *, #15033, .F. ) ;
#11226 = DIRECTION ( 'NONE',  ( 1.000000000000000000, 0.000000000000000000, 0.000000000000000000 ) ) ;
#11227 = ORIENTED_EDGE ( 'NONE', *, *, #33623, .T. ) ;
#11228 = DIRECTION ( 'NONE',  ( 0.000000000000000000, 0.000000000000000000, -1.000000000000000000 ) ) ;
#11229 = CARTESIAN_POINT ( 'NONE',  ( 0.1184242373551691735, -0.7868154500338676582, 0.6262615020233922580 ) ) ;
#11231 = DIRECTION ( 'NONE',  ( 1.000000000000000000, 6.779273404243070203E-32, -6.162975822039154730E-33 ) ) ;
#11230 = CARTESIAN_POINT ( 'NONE',  ( 0.06842540263846834392, -0.5687803859286276742, 0.05749882982346820465 ) ) ;
#11232 = CARTESIAN_POINT ( 'NONE',  ( 0.1826048122412617103, -1.261403426677984108, 0.5133468128926989005 ) ) ;
#11233 = ORIENTED_EDGE ( 'NONE', *, *, #24141, .T. ) ;
#11234 = AXIS2_PLACEMENT_3D ( 'NONE', #28228, #15887, #37689 ) ;
#11235 = EDGE_LOOP ( 'NONE', ( #20083, #32301, #12049, #19923 ) ) ;
#11236 = DIRECTION ( 'NONE',  ( 0.000000000000000000, 0.000000000000000000, -1.000000000000000000 ) ) ;
#11237 = CARTESIAN_POINT ( 'NONE',  ( 0.2939024926760947509, -1.010691472418420389, 0.7713339393085973938 ) ) ;
#11238 = ORIENTED_EDGE ( 'NONE', *, *, #1297, .T. ) ;
#11239 = DIRECTION ( 'NONE',  ( 0.8660512985181135770, 0.4999551463232371207, 0.000000000000000000 ) ) ;
#11240 = CARTESIAN_POINT ( 'NONE',  ( 0.04575185649130646820, -0.4792489163483505399, 0.08731931755211817803 ) ) ;
#11241 = EDGE_CURVE ( 'NONE', #2621, #8621, #21200, .T. ) ;
#11242 = CIRCLE ( 'NONE', #2032, 0.08249999999977555842 ) ;
#11243 = CARTESIAN_POINT ( 'NONE',  ( 0.3693472207122593387, -1.758516063299185195, -0.4275751132368607599 ) ) ;
#11244 = CIRCLE ( 'NONE', #3335, 0.04330708661417322775 ) ;
#11245 = CARTESIAN_POINT ( 'NONE',  ( 0.2343801618657880559, -1.231732140494844030, 0.5084283139525508366 ) ) ;
#11246 = CIRCLE ( 'NONE', #15863, 0.05000000000000000971 ) ;
#11247 = EDGE_CURVE ( 'NONE', #21046, #24008, #19239, .T. ) ;
#11248 = DIRECTION ( 'NONE',  ( 0.000000000000000000, 0.000000000000000000, -1.000000000000000000 ) ) ;
#11249 = CARTESIAN_POINT ( 'NONE',  ( 0.3933751395322767075, -1.752169251404669836, -0.4834917239368273223 ) ) ;
#11250 = CARTESIAN_POINT ( 'NONE',  ( 0.6859459673519229250, -1.411154268469613227, 0.7682993476293730195 ) ) ;
#11251 = CARTESIAN_POINT ( 'NONE',  ( 0.3627000673212703030, -1.755081015781649656, -0.5954581570135634161 ) ) ;
#11252 = CARTESIAN_POINT ( 'NONE',  ( 0.03158843595483436933, -0.2432919444504229867, -0.4277514783322127201 ) ) ;
#11253 = ADVANCED_FACE ( 'NONE', ( #30221 ), #39290, .F. ) ;
#11255 = VECTOR ( 'NONE', #20306, 39.37007874015748143 ) ;
#11254 = CARTESIAN_POINT ( 'NONE',  ( 0.6226077036546983079, -1.616690395946017489, -0.5571391715294409241 ) ) ;
#11256 = CARTESIAN_POINT ( 'NONE',  ( 0.03174060074380782165, 0.3664546090234515607, 0.3753288017716206459 ) ) ;
#11257 = DIRECTION ( 'NONE',  ( 0.000000000000000000, 0.000000000000000000, -1.000000000000000000 ) ) ;
#11258 = DIRECTION ( 'NONE',  ( 0.000000000000000000, 0.000000000000000000, 1.000000000000000000 ) ) ;
#11259 = CARTESIAN_POINT ( 'NONE',  ( 0.08344352785338075840, -1.320654673502084098, 0.4605903863189703684 ) ) ;
#11260 = ADVANCED_FACE ( 'NONE', ( #39688 ), #35671, .T. ) ;
#11261 = CARTESIAN_POINT ( 'NONE',  ( 0.04961935711675592720, -0.7636540146707464505, 0.7296111229395446651 ) ) ;
#11262 = CARTESIAN_POINT ( 'NONE',  ( 0.5786394055816501680, -1.530760785047180272, -0.4642196941395432264 ) ) ;
#11263 = EDGE_CURVE ( 'NONE', #16305, #20093, #24495, .T. ) ;
#11264 = CARTESIAN_POINT ( 'NONE',  ( 0.2617674847955998030, -1.607303447862003631, -0.3199733892743805708 ) ) ;
#11265 = AXIS2_PLACEMENT_3D ( 'NONE', #16062, #12975, #38054 ) ;
#11266 = DIRECTION ( 'NONE',  ( 0.000000000000000000, 0.000000000000000000, -1.000000000000000000 ) ) ;
#11267 = CARTESIAN_POINT ( 'NONE',  ( -0.05281452789367974132, -0.2421206024358327213, 0.4009379267244617684 ) ) ;
#11268 = ADVANCED_FACE ( 'NONE', ( #23484 ), #36194, .F. ) ;
#11269 = ORIENTED_EDGE ( 'NONE', *, *, #32755, .T. ) ;
#11270 = CARTESIAN_POINT ( 'NONE',  ( 0.01548846960707278911, -0.5198120922912308206, 0.07362328916738182516 ) ) ;
#11271 = AXIS2_PLACEMENT_3D ( 'NONE', #34000, #5805, #33195 ) ;
#11272 = CARTESIAN_POINT ( 'NONE',  ( 0.3207148961678939481, -1.182401600646133089, 0.3667417262808778111 ) ) ;
#11273 = DIRECTION ( 'NONE',  ( 0.4999551463232372317, -0.8660512985181135770, 0.000000000000000000 ) ) ;
#11274 = CARTESIAN_POINT ( 'NONE',  ( -1.694818351060767551E-32, 4.163336342344336410E-17, 0.1249999999999999584 ) ) ;
#11275 = CARTESIAN_POINT ( 'NONE',  ( 0.5335270692236984136, -1.350917419745129466, 0.6007964825855031110 ) ) ;
#11277 = EDGE_LOOP ( 'NONE', ( #23490, #19581, #15490, #32458, #39385, #7204, #14400 ) ) ;
#11276 = CARTESIAN_POINT ( 'NONE',  ( -0.05562144613422686373, 0.4441896308501013801, 0.1229845283801401928 ) ) ;
#11278 = CARTESIAN_POINT ( 'NONE',  ( 0.4926052497631904226, -1.101322287461897975, 0.6863075852112333619 ) ) ;
#11279 = CARTESIAN_POINT ( 'NONE',  ( 0.003604657698724842135, -1.841449275801259056, -0.3518445214664046028 ) ) ;
#11280 = ORIENTED_EDGE ( 'NONE', *, *, #34264, .F. ) ;
#11281 = DIRECTION ( 'NONE',  ( 1.000000000000000000, -0.000000000000000000, -0.000000000000000000 ) ) ;
#11282 = ORIENTED_EDGE ( 'NONE', *, *, #23744, .F. ) ;
#11283 = CARTESIAN_POINT ( 'NONE',  ( 0.3592589994864452962, -1.616760386158514251, 0.6673211502991388544 ) ) ;
#11285 = CARTESIAN_POINT ( 'NONE',  ( -0.01548846960712804005, -0.3688619771571925998, 0.3775276577326319161 ) ) ;
#11284 = CARTESIAN_POINT ( 'NONE',  ( 0.6826933326075008690, -1.509735114952027724, 0.4536807863530596396 ) ) ;
#11286 = CARTESIAN_POINT ( 'NONE',  ( 0.3211756810167746834, -1.183199798883805887, 0.5707417262808780478 ) ) ;
#11287 = LINE ( 'NONE', #23856, #19874 ) ;
#11288 = EDGE_LOOP ( 'NONE', ( #16373, #39390, #19933, #20712, #17449, #24700, #35668, #1397, #5848 ) ) ;
#11289 = ORIENTED_EDGE ( 'NONE', *, *, #30591, .F. ) ;
#11290 = CARTESIAN_POINT ( 'NONE',  ( 3.007606603700621411E-05, -2.025203935284336065, -0.6754650421693230156 ) ) ;
#11291 = DIRECTION ( 'NONE',  ( -1.000000000000000000, 0.000000000000000000, 0.000000000000000000 ) ) ;
#11292 = CARTESIAN_POINT ( 'NONE',  ( 0.1695210371906753222, -0.9850032004317544887, 0.6936202826021303780 ) ) ;
#11293 = LINE ( 'NONE', #14371, #30351 ) ;
#11294 = CIRCLE ( 'NONE', #26429, 0.005000000000000014849 ) ;
#11295 = EDGE_CURVE ( 'NONE', #35061, #33391, #2815, .T. ) ;
#11296 = CARTESIAN_POINT ( 'NONE',  ( -0.2399999999999999079, -2.416006048095809877, -1.059240699271965402 ) ) ;
#11297 = ADVANCED_FACE ( 'NONE', ( #27158 ), #26947, .T. ) ;
#11298 = ADVANCED_BREP_SHAPE_REPRESENTATION ( '', ( #4903, #27819 ), #23225 ) ;
#11299 = CARTESIAN_POINT ( 'NONE',  ( 2.988985998443356465E-16, -0.02999999999999982195, 0.2000000000000000389 ) ) ;
#11300 = AXIS2_PLACEMENT_3D ( 'NONE', #34194, #22093, #40575 ) ;
#11301 = CARTESIAN_POINT ( 'NONE',  ( -0.1127636766158876952, -0.5184084763139977792, 0.1453728055589495471 ) ) ;
#11302 = VECTOR ( 'NONE', #20370, 39.37007874015748143 ) ;
#11303 = CARTESIAN_POINT ( 'NONE',  ( 0.3465569301755319076, -1.167400393090313404, 0.4215427493204025877 ) ) ;
#11304 = CYLINDRICAL_SURFACE ( 'NONE', #6922, 0.1000000000000000194 ) ;
#11305 = DIRECTION ( 'NONE',  ( 0.000000000000000000, 6.829619984160658243E-15, -1.000000000000000000 ) ) ;
#11306 = APPROVAL_STATUS ( 'not_yet_approved' ) ;
#11307 = CIRCLE ( 'NONE', #25119, 0.05330708661417327826 ) ;
#11308 = CARTESIAN_POINT ( 'NONE',  ( 0.06380145895344221940, -1.331679772128220751, 0.6026722500081351797 ) ) ;
#11309 = CARTESIAN_POINT ( 'NONE',  ( 0.02869942827333354235, -0.4519168387192312175, 0.2102852866807465304 ) ) ;
#11310 = DIRECTION ( 'NONE',  ( -0.8660512985181132439, -0.4999551463232376758, 0.000000000000000000 ) ) ;
#11311 = CARTESIAN_POINT ( 'NONE',  ( 0.0002784714592843559058, -0.4877735126986449954, -0.003907027868444597034 ) ) ;
#11312 = CARTESIAN_POINT ( 'NONE',  ( -0.2267371898560522903, -0.4872893062166341327, 0.3599999999999997091 ) ) ;
#11313 = CARTESIAN_POINT ( 'NONE',  ( 0.07697101544015785834, -0.8504277950014116350, 0.8348144624976774342 ) ) ;
#11314 = CARTESIAN_POINT ( 'NONE',  ( -1.019575837292303166, -0.04310840302197994911, 0.09999999999999879818 ) ) ;
#11315 = EDGE_LOOP ( 'NONE', ( #13394, #3272, #14839, #22386 ) ) ;
#11316 = ORIENTED_EDGE ( 'NONE', *, *, #5489, .F. ) ;
#11317 = CARTESIAN_POINT ( 'NONE',  ( 0.1799893395252018524, -0.5084901828474633900, 0.2372766076402116897 ) ) ;
#11318 = VERTEX_POINT ( 'NONE', #17876 ) ;
#11319 = DIRECTION ( 'NONE',  ( 0.000000000000000000, 0.000000000000000000, -1.000000000000000000 ) ) ;
#11320 = AXIS2_PLACEMENT_3D ( 'NONE', #28405, #24726, #8867 ) ;
#11321 = DIRECTION ( 'NONE',  ( 0.000000000000000000, 0.000000000000000000, -1.000000000000000000 ) ) ;
#11323 = ORIENTED_EDGE ( 'NONE', *, *, #11717, .T. ) ;
#11322 = CARTESIAN_POINT ( 'NONE',  ( 0.0004130725403994839557, -0.6456490322605723531, -0.008477622837938958433 ) ) ;
#11324 = ORIENTED_EDGE ( 'NONE', *, *, #25393, .T. ) ;
#11325 = CARTESIAN_POINT ( 'NONE',  ( 0.1445495956827405892, -0.5724930378805425102, 0.4876118625187007560 ) ) ;
#11326 = AXIS2_PLACEMENT_3D ( 'NONE', #11561, #33537, #39934 ) ;
#11327 = ORIENTED_EDGE ( 'NONE', *, *, #34266, .T. ) ;
#11328 = CIRCLE ( 'NONE', #6704, 0.06434668806854085266 ) ;
#11329 = CARTESIAN_POINT ( 'NONE',  ( 0.01631055661851274138, -0.7363905679946652905, 0.6008399523819771826 ) ) ;
#11331 = CARTESIAN_POINT ( 'NONE',  ( 0.5406636675755426280, -1.597291370477161410, -0.4587226045079861314 ) ) ;
#11330 = CARTESIAN_POINT ( 'NONE',  ( -0.01548846960721259221, -0.5203207976464859774, -0.08861466064783186936 ) ) ;
#11332 = DIRECTION ( 'NONE',  ( 0.4999551463232371762, -0.8660512985181134660, 0.000000000000000000 ) ) ;
#11333 = CALENDAR_DATE ( 2026, 13, 10 ) ;
#11334 = CIRCLE ( 'NONE', #19879, 0.03000000000000001277 ) ;
#11335 = FACE_OUTER_BOUND ( 'NONE', #21918, .T. ) ;
#11337 = EDGE_LOOP ( 'NONE', ( #12211, #37687, #23352, #40094, #27980, #12138, #12738, #31279, #21265 ) ) ;
#11336 = ORIENTED_EDGE ( 'NONE', *, *, #5471, .T. ) ;
#11338 = DIRECTION ( 'NONE',  ( 0.000000000000000000, 1.000000000000000000, -1.224646799147353207E-16 ) ) ;
#11339 = CARTESIAN_POINT ( 'NONE',  ( 0.1187488235998804681, -1.413962359561577786, 0.5741705506523664404 ) ) ;
#11340 = B_SPLINE_SURFACE_WITH_KNOTS ( 'NONE', 3, 3, ( 
 ( #5847, #33632, #12048, #5445, #24606, #15334, #8956, #30567, #2393, #21528, #18408, #27891, #12255, #37334, #9147, #21710, #9346, #19446, #28277, #19235, #18843, #37524, #3985, #25423, #24993, #35274, #31383, #22145, #31779, #12635, #22535, #40623, #15938, #7069 ),
 ( #21926, #19640, #13254, #34660, #6268, #31984, #13060, #3796, #12439, #6661, #144, #6463, #34455, #358, #28096, #3187, #12862, #15728, #37953, #25201, #35062, #9967, #38343, #37744, #9566, #19033, #31564, #3382, #565, #22746, #28483, #9764, #22333, #32174 ),
 ( #34853, #28887, #3594, #16163, #28700, #25612, #38143, #16351, #10177, #6870, #25822, #748, #10379, #8086, #1759, #10569, #35458, #20447, #1545, #32981, #956, #35880, #16760, #35670, #22942, #29501, #33198, #13467, #1340, #7260, #13848, #19834, #23557, #39174 ),
 ( #26421, #7692, #13656, #32368, #38956, #26835, #38743, #7473, #4192, #4786, #10786, #23359, #38556, #17361, #26033, #20257, #32583, #17152, #32778, #7873, #4580, #29701, #29308, #14066, #26643, #14271, #11183, #10999, #26221, #1155, #23143, #20051, #4399, #16956 ),
 ( #36075, #29917, #39364, #23743, #36266, #20663, #16548, #29089, #5003, #39968, #17753, #33804, #37089, #11789, #21266, #11385, #2737, #30306, #5609, #8905, #40378, #21481, #27240, #27633, #27443, #8494, #39772, #18166, #30516, #40163, #34002, #30720, #5807, #5200 ),
 ( #33585, #39552, #14884, #18366, #2344, #23957, #1943, #24164, #27026, #36881, #24346, #8689, #12205, #2541, #36487, #30912, #2133, #15079, #8301, #14458, #21668, #11993, #20872, #24764, #14669, #24557, #15282, #27839, #37286, #33393, #9102, #11602, #17569, #30112 ),
 ( #36688, #21058, #5395, #17956, #15685, #34803, #18985, #16114, #38095, #9720, #22485, #34407, #19188, #16311, #6606, #21880, #15893, #6417, #22288, #28437, #6223, #6008, #25567, #35010, #13201, #9913, #18791, #22095, #31728, #6822, #2947, #707, #38294, #37907 ),
 ( #31129, #25774, #24952, #28236, #3545, #31342, #28654, #18573, #34618, #10124, #34196, #15498, #12397, #28052, #40577, #523, #37480, #9302, #31517, #19404, #3147, #31939, #3759, #28846, #99, #12596, #3329, #13016, #25156, #37695, #9518, #310, #12816, #25375 ),
 ( #32324, #13411, #25987, #38705, #35831, #17311, #39317, #911, #10525, #1705, #22700, #38906, #36027, #29865, #7644, #32134, #3937, #20208, #32934, #10341, #16499, #23095, #20000, #17106, #35621, #14225, #38512, #23512, #32533, #39125, #29043, #4141, #22903, #32733 ),
 ( #29457, #19601, #16709, #16913, #26791, #35422, #7423, #4352, #26375, #7216, #19782, #1302, #13807, #23307, #10733, #14013, #4539, #29654, #29255, #1499, #26585, #7831, #35232, #10950, #1109, #13617, #26181, #20402, #4740, #7033, #2689, #30069, #17905, #8037 ) ),
 .UNSPECIFIED., .F., .F., .F.,
 ( 4, 3, 3, 4 ),
 ( 4, 3, 3, 3, 3, 3, 3, 3, 3, 3, 3, 4 ),
 ( 0.2088659071706846226, 0.5009378285833450128, 0.6469737892896751941, 0.7930097499960053753 ),
 ( 0.3645345204366292058, 0.4439677053820508812, 0.5234008903274726121, 0.6028340752728943430, 0.6822672602183160739, 0.7617004451637376938, 0.8411336301091594247, 0.8808502225818702902, 0.9205668150545811557, 0.9602834075272920211, 0.9801417037636475094, 1.000000000000002887 ),
 .UNSPECIFIED. ) ;
#11341 = CARTESIAN_POINT ( 'NONE',  ( 0.1139667446832752368, -0.6485154308321814387, 0.4297538792301814903 ) ) ;
#11342 = CARTESIAN_POINT ( 'NONE',  ( 0.1871628350115532857, -0.7098502299333919741, 0.03075682391282563016 ) ) ;
#11343 = CARTESIAN_POINT ( 'NONE',  ( -0.2399999999999999079, -2.183180860297908144, -0.4937760292030871079 ) ) ;
#11344 = DIRECTION ( 'NONE',  ( 0.4999999999999966693, 0.3120216385968345163, 0.8078629197130845485 ) ) ;
#11345 = CARTESIAN_POINT ( 'NONE',  ( 0.4054385157837457898, -1.690091043903728663, -0.4198998561151282005 ) ) ;
#11346 = CARTESIAN_POINT ( 'NONE',  ( 0.3795613398208534384, -1.760143698493221942, -0.5723197561600823491 ) ) ;
#11347 = CARTESIAN_POINT ( 'NONE',  ( 0.000000000000000000, -0.02999999999999995379, 0.000000000000000000 ) ) ;
#11348 = DIRECTION ( 'NONE',  ( 0.9998941247116546194, -0.01455087607601020239, 0.0001066420868422379362 ) ) ;
#11349 = CARTESIAN_POINT ( 'NONE',  ( 0.3999999999999788169, -2.120743408781763595, -0.4622665795123166999 ) ) ;
#11350 = DIRECTION ( 'NONE',  ( 1.000000000000000000, 0.000000000000000000, 0.000000000000000000 ) ) ;
#11351 = CARTESIAN_POINT ( 'NONE',  ( 0.4380553862277722921, -1.229819722584721164, 0.5856983068965045947 ) ) ;
#11352 = B_SPLINE_CURVE_WITH_KNOTS ( 'NONE', 3,
 ( #1279, #4331, #16684, #16893, #25351, #37888, #25966, #6585, #26163, #38491, #35402, #7195, #9700, #38683, #19763, #16091 ),
 .UNSPECIFIED., .F., .F.,
 ( 4, 2, 2, 2, 2, 2, 2, 4 ),
 ( 4.646041361794957016E-06, 0.0005830979320143057703, 0.001161549822666816615, 0.001740001713319327351, 0.002318453603971838521, 0.002896905494624349257, 0.003475357385276859994, 0.004632261166581898813 ),
 .UNSPECIFIED. ) ;
#11353 = B_SPLINE_CURVE_WITH_KNOTS ( 'NONE', 3,
 ( #23600, #36115, #5050, #32635 ),
 .UNSPECIFIED., .F., .F.,
 ( 4, 4 ),
 ( 0.000000000000000000, 0.004359680035278114957 ),
 .UNSPECIFIED. ) ;
#11354 = AXIS2_PLACEMENT_3D ( 'NONE', #39518, #11348, #23919 ) ;
#11355 = CARTESIAN_POINT ( 'NONE',  ( 0.2026016520682514532, -1.284966195589533067, -0.7446434123579800390 ) ) ;
#11356 = CARTESIAN_POINT ( 'NONE',  ( 0.1835308262027276760, -1.352961526709849149, 0.9396307682827382823 ) ) ;
#11357 = CARTESIAN_POINT ( 'NONE',  ( 0.4045633573398161875, -1.022308794230461171, 0.6485999566564401020 ) ) ;
#11358 = PERSON_AND_ORGANIZATION ( #28500, #32463 ) ;
#11359 = AXIS2_PLACEMENT_3D ( 'NONE', #13723, #26289, #10642 ) ;
#11360 = CARTESIAN_POINT ( 'NONE',  ( 0.2978499211271074532, -0.7548715063715667473, 0.6844903506759184575 ) ) ;
#11361 = CIRCLE ( 'NONE', #4119, 0.04330708661417340122 ) ;
#11362 = CIRCLE ( 'NONE', #18589, 0.03000000000000003358 ) ;
#11363 = DIRECTION ( 'NONE',  ( -0.8660512985181135770, -0.4999551463232371207, 0.000000000000000000 ) ) ;
#11364 = CARTESIAN_POINT ( 'NONE',  ( 0.01548846960707350381, -0.07651041855118986823, -0.5222379212568243334 ) ) ;
#11365 = AXIS2_PLACEMENT_3D ( 'NONE', #7324, #1024, #38412 ) ;
#11366 = ORIENTED_EDGE ( 'NONE', *, *, #36357, .T. ) ;
#11367 = CARTESIAN_POINT ( 'NONE',  ( 0.3211013594029290541, -1.758905195063801052, 0.5654687988106404939 ) ) ;
#11368 = CARTESIAN_POINT ( 'NONE',  ( 0.01305698674251137489, -0.5857752844667294401, 0.3380397419882886223 ) ) ;
#11369 = CARTESIAN_POINT ( 'NONE',  ( 0.3191806098734731312, -1.644742521496082688, 0.4260382800181419238 ) ) ;
#11370 = AXIS2_PLACEMENT_3D ( 'NONE', #5204, #16961, #17758 ) ;
#11372 = EDGE_LOOP ( 'NONE', ( #19122, #32608, #10927, #17300, #31501 ) ) ;
#11371 = CARTESIAN_POINT ( 'NONE',  ( -0.2746410161513770931, -2.853330612949663170, -0.7088139570729240502 ) ) ;
#11373 = CARTESIAN_POINT ( 'NONE',  ( 0.1443375672974070711, 0.05141091571461162829, 0.000000000000000000 ) ) ;
#11374 = CARTESIAN_POINT ( 'NONE',  ( 0.5308880977089266429, -1.160028955924689242, 0.7442320808281387423 ) ) ;
#11376 = VERTEX_POINT ( 'NONE', #39479 ) ;
#11375 = VERTEX_POINT ( 'NONE', #26760 ) ;
#11377 = CARTESIAN_POINT ( 'NONE',  ( 0.004836683785373215722, -1.808528659688425577, -0.6707443805300201678 ) ) ;
#11378 = CARTESIAN_POINT ( 'NONE',  ( 0.5227242486541291422, -1.180980899171317322, -0.4111404562665418871 ) ) ;
#11379 = DIRECTION ( 'NONE',  ( 0.000000000000000000, 1.000000000000000000, 7.931692224083225994E-17 ) ) ;
#11380 = CALENDAR_DATE ( 2026, 13, 10 ) ;
#11381 = AXIS2_PLACEMENT_3D ( 'NONE', #30881, #25122, #37660 ) ;
#11382 = CARTESIAN_POINT ( 'NONE',  ( -0.04575334816098172719, 0.4390433668671429590, -0.2110480141057351211 ) ) ;
#11383 = ORIENTED_EDGE ( 'NONE', *, *, #12837, .F. ) ;
#11384 = CARTESIAN_POINT ( 'NONE',  ( 0.1998159314661579755, -2.070111469871240395, -0.2999320603925721973 ) ) ;
#11385 = CARTESIAN_POINT ( 'NONE',  ( 0.1177726229696089005, -0.7519543602322694698, 0.4275972577093408722 ) ) ;
#11386 = VECTOR ( 'NONE', #16240, 39.37007874015748143 ) ;
#11387 = CARTESIAN_POINT ( 'NONE',  ( 0.2968214893875291693, -1.658325148620396261, 0.8976394753983624186 ) ) ;
#11388 = AXIS2_PLACEMENT_3D ( 'NONE', #29389, #4659, #29179 ) ;
#11389 = CARTESIAN_POINT ( 'NONE',  ( 0.09764433117057016998, -0.5450118788951328064, 0.1538195766994619462 ) ) ;
#11391 = DIRECTION ( 'NONE',  ( 8.881784197001246407E-16, -2.361472542561082612E-16, 1.000000000000000000 ) ) ;
#11390 = CARTESIAN_POINT ( 'NONE',  ( 0.1139096195112916099, -0.5666989323863135253, -0.06299521055917528534 ) ) ;
#11392 = CARTESIAN_POINT ( 'NONE',  ( 0.05396242693373293209, -1.112133054815703348, 0.6504500721729179480 ) ) ;
#11393 = VERTEX_POINT ( 'NONE', #31047 ) ;
#11394 = VERTEX_POINT ( 'NONE', #15007 ) ;
#11395 = CARTESIAN_POINT ( 'NONE',  ( -0.1574377185082707353, 0.4885537809602767401, 0.1000000000000000194 ) ) ;
#11396 = CARTESIAN_POINT ( 'NONE',  ( 0.5894480801153691996, -1.254546968075577418, 0.8139536464034254903 ) ) ;
#11397 = CIRCLE ( 'NONE', #32407, 0.06250000000000001388 ) ;
#11398 = CARTESIAN_POINT ( 'NONE',  ( 0.3690965330173307524, -1.099411688709415413, 0.5182417262812423209 ) ) ;
#11399 =( GEOMETRIC_REPRESENTATION_CONTEXT ( 3 ) GLOBAL_UNCERTAINTY_ASSIGNED_CONTEXT ( ( #15737 ) ) GLOBAL_UNIT_ASSIGNED_CONTEXT ( ( #1126, #26195, #23112 ) ) REPRESENTATION_CONTEXT ( 'NONE', 'WORKASPACE' ) );
#11400 = EDGE_CURVE ( 'NONE', #4182, #3488, #26722, .T. ) ;
#11401 = CARTESIAN_POINT ( 'NONE',  ( 0.4688079631758284016, -1.116561345930851656, 0.5688791344137259509 ) ) ;
#11402 = APPLIED_DATE_AND_TIME_ASSIGNMENT ( #2918, #24930, ( #19425 ) ) ;
#11403 = CARTESIAN_POINT ( 'NONE',  ( -0.05543910610524967891, -0.4320206429437797868, -0.1617740274009885904 ) ) ;
#11404 = FACE_OUTER_BOUND ( 'NONE', #5649, .T. ) ;
#11405 = CARTESIAN_POINT ( 'NONE',  ( 0.3937935369999097657, -1.750528853568169341, -0.7155743560682789051 ) ) ;
#11406 = CARTESIAN_POINT ( 'NONE',  ( 0.3154536323005096010, -1.185489152943391078, 0.5575863575408869233 ) ) ;
#11407 = CARTESIAN_POINT ( 'NONE',  ( 0.5932568134822767680, -1.254512724160953940, 0.6928994325643027530 ) ) ;
#11408 = SHAPE_DEFINITION_REPRESENTATION ( #17355, #30147 ) ;
#11409 =( BOUNDED_SURFACE ( )  B_SPLINE_SURFACE ( 3, 2, ( 
 ( #34146, #2683, #12148 ),
 ( #27992, #37433, #9245 ),
 ( #15641, #21822, #28388 ),
 ( #28188, #53, #37640 ),
 ( #9459, #257, #12755 ),
 ( #22647, #16654, #32083 ),
 ( #32475, #13755, #32267 ),
 ( #471, #29203, #29408 ),
 ( #12968, #35177, #16444 ),
 ( #6980, #26321, #22433 ) ),
 .UNSPECIFIED., .F., .F., .F. ) 
 B_SPLINE_SURFACE_WITH_KNOTS ( ( 4, 2, 2, 2, 4 ),
 ( 3, 3 ),
 ( 1.517883041479706208E-18, 0.0005537231258318653241, 0.001107446251663729130, 0.001661169377495592828, 0.002214892503327456526 ),
 ( 0.000000000000000000, 1.000000000000000000 ),
 .UNSPECIFIED. ) 
 GEOMETRIC_REPRESENTATION_ITEM ( )  RATIONAL_B_SPLINE_SURFACE ( (
 ( 1.000000000000000000, 0.7071067811865474617, 1.000000000000000000),
 ( 1.000000000000000000, 0.7265894298401162077, 1.000000000000000000),
 ( 1.000000000000000000, 0.7434232128335919176, 1.000000000000000000),
 ( 1.000000000000000000, 0.7721148371329119575, 1.000000000000000000),
 ( 1.000000000000000000, 0.7840904396559796874, 1.000000000000000000),
 ( 1.000000000000000000, 0.8021033243800309576, 1.000000000000000000),
 ( 1.000000000000000000, 0.8082547127764595496, 1.000000000000000000),
 ( 1.000000000000000000, 0.8155145129532223036, 1.000000000000000000),
 ( 1.000000000000000000, 0.8165278830576885305, 1.000000000000000000),
 ( 1.000000000000000000, 0.8164965809277219266, 1.000000000000000000) ) ) 
 REPRESENTATION_ITEM ( '' )  SURFACE ( )  );
#11410 = DIRECTION ( 'NONE',  ( -7.771561172376107616E-16, 7.170354002788761615E-17, -1.000000000000000000 ) ) ;
#11411 = CARTESIAN_POINT ( 'NONE',  ( 0.09022811215523972306, -1.443092559558259991, -0.3376645326784880052 ) ) ;
#11412 = CARTESIAN_POINT ( 'NONE',  ( 0.1986386779382385004, -2.044490618953881178, -0.6815266969527320473 ) ) ;
#11413 = EDGE_LOOP ( 'NONE', ( #6229, #20805, #4090, #27575, #29339, #17836, #34399, #31270 ) ) ;
#11414 = CYLINDRICAL_SURFACE ( 'NONE', #6352, 0.1000000000000000194 ) ;
#11415 = DIRECTION ( 'NONE',  ( 1.000000000000000000, 2.280301054154495132E-31, -1.664003471950577689E-31 ) ) ;
#11416 = CARTESIAN_POINT ( 'NONE',  ( -0.03877220711930252917, -0.3061923002804363692, -0.3649281646214425634 ) ) ;
#11417 = AXIS2_PLACEMENT_3D ( 'NONE', #30743, #17985, #40191 ) ;
#11418 = AXIS2_PLACEMENT_3D ( 'NONE', #3487, #25508, #26131 ) ;
#11419 = ORIENTED_EDGE ( 'NONE', *, *, #26350, .T. ) ;
#11420 = CARTESIAN_POINT ( 'NONE',  ( -0.02953079040095639429, 0.4684706630666118365, 0.2484463060367366194 ) ) ;
#11421 = CARTESIAN_POINT ( 'NONE',  ( 0.4125455718730863808, -1.129683035667270685, 0.5355335411479252850 ) ) ;
#11422 = EDGE_CURVE ( 'NONE', #1137, #8761, #8057, .T. ) ;
#11423 = CIRCLE ( 'NONE', #39669, 0.04330708661417327632 ) ;
#11424 = CARTESIAN_POINT ( 'NONE',  ( 0.1284780417918266471, -1.109535762947133186, 0.7509360102231731338 ) ) ;
#11425 = VERTEX_POINT ( 'NONE', #5743 ) ;
#11426 = EDGE_CURVE ( 'NONE', #4682, #24540, #7398, .T. ) ;
#11427 = CARTESIAN_POINT ( 'NONE',  ( 0.05283102792148739596, 0.3063958269170706794, 0.3541938269410513374 ) ) ;
#11428 = CIRCLE ( 'NONE', #27212, 0.08000000000000000167 ) ;
#11429 = CARTESIAN_POINT ( 'NONE',  ( 0.4138729472876766513, -1.128955312352843965, 0.5470489658417444501 ) ) ;
#11430 = CARTESIAN_POINT ( 'NONE',  ( -0.05464101615137770263, -2.116970787486931460, -0.3045972195783253067 ) ) ;
#11431 = B_SPLINE_CURVE_WITH_KNOTS ( 'NONE', 3,
 ( #3180, #31768, #3372, #12629 ),
 .UNSPECIFIED., .F., .F.,
 ( 4, 4 ),
 ( 0.000000000000000000, 0.0008608482128229501219 ),
 .UNSPECIFIED. ) ;
#11432 = CARTESIAN_POINT ( 'NONE',  ( 0.1870594047279228178, -1.705895718177093290, -0.3287721483933107591 ) ) ;
#11433 = EDGE_CURVE ( 'NONE', #24980, #28467, #8609, .T. ) ;
#11434 = CARTESIAN_POINT ( 'NONE',  ( 0.4531756115490733205, -1.216278074989430635, 0.6647715044327879852 ) ) ;
#11436 = DIRECTION ( 'NONE',  ( -1.000000000000000000, -0.000000000000000000, -0.000000000000000000 ) ) ;
#11435 = DIRECTION ( 'NONE',  ( -1.309010496964125854E-14, 0.9672079024885572585, 0.2539859708009193917 ) ) ;
#11437 = ADVANCED_FACE ( 'NONE', ( #27562 ), #40083, .F. ) ;
#11438 = FACE_OUTER_BOUND ( 'NONE', #27695, .T. ) ;
#11439 = ORIENTED_EDGE ( 'NONE', *, *, #35638, .T. ) ;
#11440 = ORIENTED_EDGE ( 'NONE', *, *, #9778, .F. ) ;
#11441 = EDGE_CURVE ( 'NONE', #19986, #33249, #21796, .T. ) ;
#11442 = CARTESIAN_POINT ( 'NONE',  ( 0.3704697912810962501, -1.166474544107111377, 0.4182417262808778013 ) ) ;
#11443 = ORIENTED_EDGE ( 'NONE', *, *, #14031, .T. ) ;
#11444 = DIRECTION ( 'NONE',  ( 0.4999551463232373427, -0.8660512985181134660, 0.000000000000000000 ) ) ;
#11445 = CARTESIAN_POINT ( 'NONE',  ( 0.2896156192559988241, -1.230497722748672418, 0.8765274707950017063 ) ) ;
#11447 = CARTESIAN_POINT ( 'NONE',  ( 0.1991979404706940571, -0.7475258006208684858, 0.3239363664478491778 ) ) ;
#11446 = CARTESIAN_POINT ( 'NONE',  ( 0.6803372715343216637, -1.562881934859470245, 0.6028921635761279596 ) ) ;
#11448 = CARTESIAN_POINT ( 'NONE',  ( 0.5727661025814071438, -1.498384876352202744, 0.4882842553274438502 ) ) ;
#11449 = ORIENTED_EDGE ( 'NONE', *, *, #10692, .T. ) ;
#11450 = VECTOR ( 'NONE', #7777, 39.37007874015748143 ) ;
#11451 = CARTESIAN_POINT ( 'NONE',  ( 0.02999778723028691946, -2.087755359801442445, -0.2623954751430958021 ) ) ;
#11452 = CARTESIAN_POINT ( 'NONE',  ( 0.5221487387134132740, -1.408661551139909429, 0.7843041425632609753 ) ) ;
#11453 = EDGE_LOOP ( 'NONE', ( #35259, #6973, #34959, #14222, #16256, #10624 ) ) ;
#11454 = CARTESIAN_POINT ( 'NONE',  ( 0.5882251369675207675, -1.618009200102772382, 0.5801761169464535461 ) ) ;
#11455 = DIRECTION ( 'NONE',  ( -7.771561172376107616E-16, 7.170354002788761615E-17, -1.000000000000000000 ) ) ;
#11456 = AXIS2_PLACEMENT_3D ( 'NONE', #23395, #20479, #32406 ) ;
#11457 = AXIS2_PLACEMENT_3D ( 'NONE', #37790, #28322, #34700 ) ;
#11458 = EDGE_CURVE ( 'NONE', #24285, #33731, #34540, .T. ) ;
#11459 = CARTESIAN_POINT ( 'NONE',  ( 0.6465835049539245816, -1.539613817736331658, 0.4182417262808776903 ) ) ;
#11460 =( GEOMETRIC_REPRESENTATION_CONTEXT ( 3 ) GLOBAL_UNCERTAINTY_ASSIGNED_CONTEXT ( ( #9976 ) ) GLOBAL_UNIT_ASSIGNED_CONTEXT ( ( #33549, #5783, #37262 ) ) REPRESENTATION_CONTEXT ( 'NONE', 'WORKASPACE' ) );
#11461 = CARTESIAN_POINT ( 'NONE',  ( 0.2117005958754011041, -1.244844897664459271, 0.4511303960385213974 ) ) ;
#11462 = CARTESIAN_POINT ( 'NONE',  ( 0.006146411395858588159, -0.5280326101355133916, 0.1457225173264089235 ) ) ;
#11463 = CARTESIAN_POINT ( 'NONE',  ( 0.3969982963057271386, -1.750077671058422712, -0.4821875037442190370 ) ) ;
#11464 = TOROIDAL_SURFACE ( 'NONE', #40379, 0.1333070866141734256, 0.02999999999999999889 ) ;
#11465 = CARTESIAN_POINT ( 'NONE',  ( 0.6930531720067659718, -1.422936651082730375, 0.7544454077531311809 ) ) ;
#11466 = AXIS2_PLACEMENT_3D ( 'NONE', #18592, #30734, #27458 ) ;
#11467 = DIRECTION ( 'NONE',  ( 8.881784197001246407E-16, -2.361472542561082612E-16, 1.000000000000000000 ) ) ;
#11468 = CARTESIAN_POINT ( 'NONE',  ( -2.194511862571855274E-05, -0.9481927139366428392, 0.1457185332388704346 ) ) ;
#11469 = CARTESIAN_POINT ( 'NONE',  ( 0.6191930749538706591, -1.620849352080218742, -0.5429756578775681852 ) ) ;
#11470 = DIRECTION ( 'NONE',  ( -1.000000000000000000, -2.280301054154495132E-31, 1.664003471950577689E-31 ) ) ;
#11471 = CARTESIAN_POINT ( 'NONE',  ( -0.2399999999999999079, -2.409101312171279208, -0.6551853038253486750 ) ) ;
#11472 = CARTESIAN_POINT ( 'NONE',  ( 0.5908959048872449715, -1.601544548465861473, 0.4282886817583849703 ) ) ;
#11473 = CARTESIAN_POINT ( 'NONE',  ( -0.02953079040095639429, 0.4684706630666080063, -0.2484463060367437248 ) ) ;
#11474 = CARTESIAN_POINT ( 'NONE',  ( 0.3165138724069220255, -1.757609964495261190, 0.6990733182572979043 ) ) ;
#11475 = CARTESIAN_POINT ( 'NONE',  ( 0.3648248434763127768, -1.736370150272759316, -0.6021910921396982364 ) ) ;
#11476 = CARTESIAN_POINT ( 'NONE',  ( 0.1817330915907873212, -1.261857734097182160, 0.5280675647135233408 ) ) ;
#11477 = CARTESIAN_POINT ( 'NONE',  ( 0.3048336326901729953, -1.756854950747158473, 0.5690634040337300137 ) ) ;
#11478 = CIRCLE ( 'NONE', #30535, 0.1946589359789743512 ) ;
#11479 = CIRCLE ( 'NONE', #34470, 0.5302738246768086139 ) ;
#11480 = ORIENTED_EDGE ( 'NONE', *, *, #19807, .F. ) ;
#11481 = ADVANCED_FACE ( 'NONE', ( #37008 ), #24531, .T. ) ;
#11482 = DIRECTION ( 'NONE',  ( 0.8660512985181130219, 0.4999551463232377868, 0.000000000000000000 ) ) ;
#11483 = CIRCLE ( 'NONE', #16740, 0.1012268159172230869 ) ;
#11484 = CARTESIAN_POINT ( 'NONE',  ( 0.3279422950026300576, -1.178402953498526751, 0.5630877674954837264 ) ) ;
#11485 = LOCAL_TIME ( 0, 53, 7.000000000000000000, #36609 ) ;
#11486 = CARTESIAN_POINT ( 'NONE',  ( 0.06923712653936904549, -0.5400029222721455247, 0.1457185332388703236 ) ) ;
#11487 = FACE_OUTER_BOUND ( 'NONE', #11493, .T. ) ;
#11488 = EDGE_CURVE ( 'NONE', #12909, #32770, #24475, .T. ) ;
#11489 = CARTESIAN_POINT ( 'NONE',  ( 0.3793388072559690793, -1.119460787698140392, 0.7530470861100434510 ) ) ;
#11491 = ORIENTED_EDGE ( 'NONE', *, *, #2894, .T. ) ;
#11490 = CARTESIAN_POINT ( 'NONE',  ( -0.1696269498702763501, 0.4941072959623512562, 0.1354043093116702456 ) ) ;
#11492 = CARTESIAN_POINT ( 'NONE',  ( 0.5043207191046787941, -1.105492587439252494, 0.6133613128836958861 ) ) ;
#11493 = EDGE_LOOP ( 'NONE', ( #39667, #39222, #3138, #15996 ) ) ;
#11494 = EDGE_CURVE ( 'NONE', #11425, #18566, #38957, .T. ) ;
#11495 = VECTOR ( 'NONE', #14333, 39.37007874015748143 ) ;
#11496 = CYLINDRICAL_SURFACE ( 'NONE', #3999, 0.01500000000000004628 ) ;
#11497 = ORIENTED_EDGE ( 'NONE', *, *, #1666, .T. ) ;
#11498 = CARTESIAN_POINT ( 'NONE',  ( -0.01548846960712810944, 0.3688619771571925998, -0.3775276577326300287 ) ) ;
#11499 = CARTESIAN_POINT ( 'NONE',  ( 0.3563569779892122313, -1.622467549537393694, 0.5771720492809274683 ) ) ;
#11501 = CARTESIAN_POINT ( 'NONE',  ( -0.04230188431063459237, -0.2825024449121562586, 0.3739792551055085568 ) ) ;
#11500 = CARTESIAN_POINT ( 'NONE',  ( 0.6968370183900322035, -1.494039123299786942, 0.4851329554411836775 ) ) ;
#11502 = CARTESIAN_POINT ( 'NONE',  ( 0.5639234115582156814, -1.619074957229330369, -0.5155029497116575543 ) ) ;
#11503 = ORIENTED_EDGE ( 'NONE', *, *, #30467, .T. ) ;
#11504 = CARTESIAN_POINT ( 'NONE',  ( 0.1757436668871035501, -1.266759027082864586, -0.7075046458427431961 ) ) ;
#11505 = DIRECTION ( 'NONE',  ( 1.000000000000000000, 0.000000000000000000, 0.000000000000000000 ) ) ;
#11506 = EDGE_CURVE ( 'NONE', #19020, #6462, #27166, .T. ) ;
#11507 = EDGE_CURVE ( 'NONE', #892, #20310, #14811, .T. ) ;
#11508 = CARTESIAN_POINT ( 'NONE',  ( 0.2944674956371818308, -1.228845936351069978, 0.7080622490502053168 ) ) ;
#11509 = CARTESIAN_POINT ( 'NONE',  ( -2.112273405726188513E-14, -2.101105564483095822, -0.6980540538755429791 ) ) ;
#11510 = EDGE_CURVE ( 'NONE', #25560, #32375, #13989, .T. ) ;
#11511 = FACE_OUTER_BOUND ( 'NONE', #6151, .T. ) ;
#11512 = EDGE_CURVE ( 'NONE', #22691, #3242, #29120, .T. ) ;
#11513 = AXIS2_PLACEMENT_3D ( 'NONE', #28245, #9527, #6618 ) ;
#11514 = AXIS2_PLACEMENT_3D ( 'NONE', #37504, #24587, #39993 ) ;
#11515 = FACE_OUTER_BOUND ( 'NONE', #30023, .T. ) ;
#11516 = CARTESIAN_POINT ( 'NONE',  ( 0.6586645934826005355, -1.563799363216411331, 0.4177417262808784670 ) ) ;
#11517 = CARTESIAN_POINT ( 'NONE',  ( 0.01548846960707511190, 0.09061086148575973886, 0.5171215251571029681 ) ) ;
#11518 = CARTESIAN_POINT ( 'NONE',  ( -0.02000000000000000042, -2.082394770077036661, -0.4779740388940064144 ) ) ;
#11519 = CARTESIAN_POINT ( 'NONE',  ( 0.05963972588713747913, -1.330888851906829595, 0.5826259623951950406 ) ) ;
#11520 = PERSON_AND_ORGANIZATION_ROLE ( 'creator' ) ;
#11521 = APPLIED_SECURITY_CLASSIFICATION_ASSIGNMENT ( #19425, ( #37152 ) ) ;
#11522 = CARTESIAN_POINT ( 'NONE',  ( 0.4157784994257035516, -1.135080422749356943, 0.4335792570559673931 ) ) ;
#11523 = CARTESIAN_POINT ( 'NONE',  ( 0.4668905103052730654, -1.236430484539588592, 0.6057417262809813296 ) ) ;
#11524 = AXIS2_PLACEMENT_3D ( 'NONE', #18295, #30834, #15196 ) ;
#11525 = CARTESIAN_POINT ( 'NONE',  ( 0.6952357793749982529, -1.543270793921424744, 0.4282417262808777547 ) ) ;
#11526 = CARTESIAN_POINT ( 'NONE',  ( 0.01192210659473974012, -0.5278220828877545623, -0.05896525035967064426 ) ) ;
#11527 = CARTESIAN_POINT ( 'NONE',  ( -0.2746410161513779258, -2.457388234162025675, -0.5792354969483111127 ) ) ;
#11528 = DIRECTION ( 'NONE',  ( 0.8724162812079783169, -0.4887635750372991139, 0.000000000000000000 ) ) ;
#11529 = DIRECTION ( 'NONE',  ( 2.532366176626898522E-12, 0.8090169943749566661, 0.5877852522924604806 ) ) ;
#11530 = ORIENTED_EDGE ( 'NONE', *, *, #27146, .T. ) ;
#11531 = ORIENTED_EDGE ( 'NONE', *, *, #20496, .F. ) ;
#11532 = CARTESIAN_POINT ( 'NONE',  ( 0.1931842209117922704, -0.5499223536180041227, 0.2739543758472387514 ) ) ;
#11533 = VERTEX_POINT ( 'NONE', #18705 ) ;
#11534 = CARTESIAN_POINT ( 'NONE',  ( 0.4570572541747411344, -1.685982556225596118, -0.4119774522368083169 ) ) ;
#11535 = AXIS2_PLACEMENT_3D ( 'NONE', #37909, #9721, #35623 ) ;
#11536 = EDGE_CURVE ( 'NONE', #35372, #243, #36070, .T. ) ;
#11538 = ORIENTED_EDGE ( 'NONE', *, *, #39139, .F. ) ;
#11537 = CARTESIAN_POINT ( 'NONE',  ( -0.1178427669581121329, -0.4906303760369132294, 0.1227918960327501474 ) ) ;
#11540 = EDGE_LOOP ( 'NONE', ( #5376, #21104, #29479, #11125 ) ) ;
#11539 = CARTESIAN_POINT ( 'NONE',  ( 0.0008024698624184804785, -0.6024510043979661722, 0.0006787156188479290470 ) ) ;
#11541 = AXIS2_PLACEMENT_3D ( 'NONE', #24632, #15564, #34262 ) ;
#11542 = ADVANCED_FACE ( 'NONE', ( #28961 ), #22410, .T. ) ;
#11543 = B_SPLINE_CURVE_WITH_KNOTS ( 'NONE', 3,
 ( #18100, #14386, #40298, #12131, #15012, #37226 ),
 .UNSPECIFIED., .F., .F.,
 ( 4, 2, 4 ),
 ( 0.000000000000000000, 0.0005867836345122920015, 0.001173567269024584003 ),
 .UNSPECIFIED. ) ;
#11544 = EDGE_LOOP ( 'NONE', ( #26124, #34406, #9552, #16695, #28697, #3656 ) ) ;
#11545 = CARTESIAN_POINT ( 'NONE',  ( 0.1156883557706581828, -0.4553337736917355549, 0.2193215644107081586 ) ) ;
#11546 = ORIENTED_EDGE ( 'NONE', *, *, #17472, .F. ) ;
#11547 = CARTESIAN_POINT ( 'NONE',  ( -0.001584010976415602514, -0.5275152449236483188, 0.1457185332388696297 ) ) ;
#11549 = CARTESIAN_POINT ( 'NONE',  ( 0.1353747033919373288, -1.277178147914981965, 0.6051480509469141511 ) ) ;
#11548 = DIRECTION ( 'NONE',  ( 0.2549153265716599392, 0.000000000000000000, 0.9669633789750592401 ) ) ;
#11550 = APPLIED_SECURITY_CLASSIFICATION_ASSIGNMENT ( #29284, ( #40649 ) ) ;
#11551 = CARTESIAN_POINT ( 'NONE',  ( -0.2399999999999999079, -3.795222634959446673, 0.02956464416125691164 ) ) ;
#11552 = DATE_AND_TIME ( #32131, #18833 ) ;
#11553 = CARTESIAN_POINT ( 'NONE',  ( 0.5934892211655993233, -1.486388914344519696, -0.3866566986715374021 ) ) ;
#11555 = ORIENTED_EDGE ( 'NONE', *, *, #38083, .T. ) ;
#11554 = ORIENTED_EDGE ( 'NONE', *, *, #6473, .T. ) ;
#11556 = CARTESIAN_POINT ( 'NONE',  ( 0.3727794023048966454, -1.123217151053685692, 0.6232678702655031211 ) ) ;
#11557 = AXIS2_PLACEMENT_3D ( 'NONE', #33261, #17631, #27314 ) ;
#11558 = CARTESIAN_POINT ( 'NONE',  ( 0.1187265588701445079, -1.410790600435402720, 0.5974809741846841549 ) ) ;
#11559 = CARTESIAN_POINT ( 'NONE',  ( 0.09010370433594069861, -0.5674124104709881156, 0.1743615206353293645 ) ) ;
#11560 = CARTESIAN_POINT ( 'NONE',  ( 0.1870560818649253665, -0.7171819408363133697, 0.03132522962495347396 ) ) ;
#11561 = CARTESIAN_POINT ( 'NONE',  ( 0.4165761542997364897, -1.741708882820427906, 0.5182417262812423209 ) ) ;
#11562 = DIRECTION ( 'NONE',  ( 1.000000000000000000, 2.280301054154495132E-31, -1.664003471950577689E-31 ) ) ;
#11563 = DIRECTION ( 'NONE',  ( 0.000000000000000000, -0.5365213554527478168, 0.8438867430782083234 ) ) ;
#11564 = FACE_OUTER_BOUND ( 'NONE', #25977, .T. ) ;
#11565 = EDGE_CURVE ( 'NONE', #18202, #39770, #13939, .T. ) ;
#11566 = CARTESIAN_POINT ( 'NONE',  ( -0.1061036098701638175, -0.4827967145417200179, 0.3599999999999999867 ) ) ;
#11567 = FACE_OUTER_BOUND ( 'NONE', #8308, .T. ) ;
#11568 = DIRECTION ( 'NONE',  ( 0.000000000000000000, 0.000000000000000000, 1.000000000000000000 ) ) ;
#11569 = CARTESIAN_POINT ( 'NONE',  ( 0.4036829562542670335, -1.110694686686239496, 0.6196874900528862584 ) ) ;
#11570 = CARTESIAN_POINT ( 'NONE',  ( 0.01548846960707528191, -0.3880410510314710182, 0.3755318131855027719 ) ) ;
#11571 = TOROIDAL_SURFACE ( 'NONE', #18111, 0.5250000000000000222, 0.01499999999999999944 ) ;
#11572 = CIRCLE ( 'NONE', #14176, 0.5400000000000017009 ) ;
#11573 = CARTESIAN_POINT ( 'NONE',  ( -0.02000000000000000042, -2.116970787486931460, -0.3045972195783253067 ) ) ;
#11574 = CARTESIAN_POINT ( 'NONE',  ( 0.2385638199407473237, -1.468035130309864655, 0.9857930272948494110 ) ) ;
#11575 = CARTESIAN_POINT ( 'NONE',  ( 0.4646871136015383597, -1.067210575163276776, 0.6251146133038130159 ) ) ;
#11576 = CARTESIAN_POINT ( 'NONE',  ( 0.0004231800003877070619, -0.8698522374252537492, 0.3712277156174843551 ) ) ;
#11577 = PERSON_AND_ORGANIZATION ( #28500, #32463 ) ;
#11578 = CARTESIAN_POINT ( 'NONE',  ( 0.6551261771431925451, -1.361944467462807395, 0.8444247977208539924 ) ) ;
#11579 = APPROVAL_PERSON_ORGANIZATION ( #33389, #19955, #40375 ) ;
#11580 = CIRCLE ( 'NONE', #31929, 0.03000000000000002318 ) ;
#11581 = CARTESIAN_POINT ( 'NONE',  ( 0.03474878377840812799, -0.07233677907409617747, -0.5114521822558271147 ) ) ;
#11582 = CARTESIAN_POINT ( 'NONE',  ( 0.3575561407676253745, -1.730055797317831434, -0.4930369608202382348 ) ) ;
#11583 = VERTEX_POINT ( 'NONE', #13548 ) ;
#11584 = CARTESIAN_POINT ( 'NONE',  ( -0.002063022417946163214, -0.8810992990880223141, 0.1457185332388702959 ) ) ;
#11585 = CARTESIAN_POINT ( 'NONE',  ( 0.08896364796864351943, -1.020649669505796053, 0.8448254586460793858 ) ) ;
#11586 = ADVANCED_FACE ( 'NONE', ( #3264, #16030 ), #25910, .F. ) ;
#11587 = CARTESIAN_POINT ( 'NONE',  ( 0.5877158659771946070, -1.491177997581171644, 0.5692036392475393614 ) ) ;
#11588 = CARTESIAN_POINT ( 'NONE',  ( 0.3722032372398466626, -1.759169682601392948, -0.4326628031163745614 ) ) ;
#11590 = ORIENTED_EDGE ( 'NONE', *, *, #30818, .T. ) ;
#11589 = LINE ( 'NONE', #14653, #40160 ) ;
#11591 = CARTESIAN_POINT ( 'NONE',  ( 0.3418186750811026964, -0.8703758711135023418, 0.7017026408156415984 ) ) ;
#11593 = ORIENTED_EDGE ( 'NONE', *, *, #33873, .T. ) ;
#11592 = ORIENTED_EDGE ( 'NONE', *, *, #14683, .T. ) ;
#11594 = CARTESIAN_POINT ( 'NONE',  ( 0.1583587972720514880, -1.279555781728052288, -0.7002456816688629182 ) ) ;
#11595 = CARTESIAN_POINT ( 'NONE',  ( 0.3616412802241140145, -1.759290408630901803, -0.5212859374495408815 ) ) ;
#11596 = CARTESIAN_POINT ( 'NONE',  ( 0.5785166455485266646, -1.495798471460381140, 0.5520824867764277943 ) ) ;
#11597 = APPROVAL_DATE_TIME ( #30716, #3604 ) ;
#11598 = CARTESIAN_POINT ( 'NONE',  ( 0.4958908375534706869, -1.219525668783798977, 0.6057417262809816627 ) ) ;
#11599 = ORIENTED_EDGE ( 'NONE', *, *, #19073, .F. ) ;
#11600 = CARTESIAN_POINT ( 'NONE',  ( -0.02000000000000000042, -2.183180860297908144, -0.4937760292030871079 ) ) ;
#11601 = AXIS2_PLACEMENT_3D ( 'NONE', #26903, #39434, #11257 ) ;
#11602 = CARTESIAN_POINT ( 'NONE',  ( 0.08647347352317601155, -0.7251180098799488993, 0.1691244536827258838 ) ) ;
#11603 = CARTESIAN_POINT ( 'NONE',  ( 0.3025690150559682823, -1.684573983455480706, 0.8624521912671884172 ) ) ;
#11604 = CARTESIAN_POINT ( 'NONE',  ( 0.4841033199777585172, -1.510029708904473189, 0.7391567888139168874 ) ) ;
#11606 = DIRECTION ( 'NONE',  ( -0.4999999999999969469, -0.5122356157878170668, -0.6982941170584776591 ) ) ;
#11605 = DIRECTION ( 'NONE',  ( 0.000000000000000000, 0.000000000000000000, 1.000000000000000000 ) ) ;
#11607 = CARTESIAN_POINT ( 'NONE',  ( 0.1701719723773303661, -1.263281085629067269, 0.5928467369345694626 ) ) ;
#11608 = SECURITY_CLASSIFICATION ( '', '', #35229 ) ;
#11609 = ORIENTED_EDGE ( 'NONE', *, *, #1221, .T. ) ;
#11610 = ORIENTED_EDGE ( 'NONE', *, *, #27569, .F. ) ;
#11611 = CARTESIAN_POINT ( 'NONE',  ( -0.2399999999999999079, -3.285933380171606188, -0.6294744526254046901 ) ) ;
#11612 = CARTESIAN_POINT ( 'NONE',  ( 0.5360489703051245503, -1.170555442393250933, 0.8194398345008427897 ) ) ;
#11613 = AXIS2_PLACEMENT_3D ( 'NONE', #32795, #30328, #23768 ) ;
#11614 = DIRECTION ( 'NONE',  ( 0.000000000000000000, -3.885780586188049371E-16, -1.000000000000000000 ) ) ;
#11615 = CARTESIAN_POINT ( 'NONE',  ( 0.04582713223189361501, -0.4389429380065721364, 0.2108029774974868320 ) ) ;
#11616 =( CONVERSION_BASED_UNIT ( 'INCH', #39785 ) LENGTH_UNIT ( ) NAMED_UNIT ( #26255 ) );
#11617 = ADVANCED_FACE ( 'NONE', ( #825 ), #29175, .F. ) ;
#11618 = CARTESIAN_POINT ( 'NONE',  ( 0.4065932041851623713, -1.147918556006411350, 0.4182417262808777458 ) ) ;
#11619 = CARTESIAN_POINT ( 'NONE',  ( 0.3909325643991080068, -1.787092977304432173, -0.7036838712262254436 ) ) ;
#11620 = CARTESIAN_POINT ( 'NONE',  ( 0.3125015783326245966, -1.187070760913759626, 0.4876403188951574097 ) ) ;
#11621 = B_SPLINE_CURVE_WITH_KNOTS ( 'NONE', 3,
 ( #34763, #22656, #28401, #861, #19148, #35191, #6779, #31685, #19562, #32092, #25722, #29210, #28612, #3899, #9870, #16662, #22443, #19359 ),
 .UNSPECIFIED., .F., .F.,
 ( 4, 2, 2, 2, 2, 2, 2, 2, 4 ),
 ( -0.002633528389679716444, -0.001975271857855715081, -0.001317015326031713285, -0.0006587587942077119223, -5.022623837101260202E-07, 0.0006577542694402916702, 0.001316010801264292599, 0.001974267333088294395, 0.002632523864912296192 ),
 .UNSPECIFIED. ) ;
#11622 = CARTESIAN_POINT ( 'NONE',  ( 0.5556047631917466756, -1.190343314783628870, 0.5823040822259395455 ) ) ;
#11623 = CALENDAR_DATE ( 2026, 13, 10 ) ;
#11624 = DIRECTION ( 'NONE',  ( -0.9378410757839558132, -0.3470650033817760383, 1.707404996040169097E-15 ) ) ;
#11625 = CIRCLE ( 'NONE', #32644, 0.5515209409081861525 ) ;
#11626 = DIRECTION ( 'NONE',  ( -7.000205099780314469E-17, -1.000000000000000000, 6.590151126658399604E-16 ) ) ;
#11627 = LINE ( 'NONE', #33418, #18859 ) ;
#11628 = CARTESIAN_POINT ( 'NONE',  ( 0.1909286924077255310, -1.257064795538239022, -0.3824824602286830411 ) ) ;
#11629 = CARTESIAN_POINT ( 'NONE',  ( 0.6062642334505776720, -1.480048462320248559, 0.5555565214026880749 ) ) ;
#11630 = EDGE_LOOP ( 'NONE', ( #37525, #8117, #16554, #39645, #25697, #37242, #35818 ) ) ;
#11631 = CARTESIAN_POINT ( 'NONE',  ( 0.4696555196854587666, -1.075282885199456251, 0.7143639487365693874 ) ) ;
#11632 = DIRECTION ( 'NONE',  ( 1.000000000000000000, 1.450082232674701412E-15, -8.188699666868902382E-16 ) ) ;
#11633 = CARTESIAN_POINT ( 'NONE',  ( -0.03647137243074970170, -0.08366781003817859441, -0.5049290013155085521 ) ) ;
#11634 = CARTESIAN_POINT ( 'NONE',  ( 0.2129387079736155819, -1.324090063805845929, 0.6635512456264479608 ) ) ;
#11635 = VERTEX_POINT ( 'NONE', #233 ) ;
#11636 = FACE_OUTER_BOUND ( 'NONE', #5383, .T. ) ;
#11637 = DIRECTION ( 'NONE',  ( -1.000000000000000000, -1.188678714063518030E-15, -5.551115123125745108E-17 ) ) ;
#11638 = CARTESIAN_POINT ( 'NONE',  ( 0.03301162916267817715, -0.4610563966203419795, -0.2426449039644940076 ) ) ;
#11639 = CARTESIAN_POINT ( 'NONE',  ( 0.2164472520689793289, -1.620189540922670313, -0.3270271536848740057 ) ) ;
#11640 = CARTESIAN_POINT ( 'NONE',  ( 0.3900902991962562072, -1.136166487165251704, 0.6916372837714432897 ) ) ;
#11642 = CARTESIAN_POINT ( 'NONE',  ( 0.2059273467974225835, -1.283046334493782359, -0.4400554600884078460 ) ) ;
#11641 = CARTESIAN_POINT ( 'NONE',  ( 0.7009661026058806588, -1.563056106223300823, -0.5155029497116575543 ) ) ;
#11643 = DIRECTION ( 'NONE',  ( -1.188678714063518227E-15, 1.000000000000000000, 3.263080277421930985E-16 ) ) ;
#11644 = ORIENTED_EDGE ( 'NONE', *, *, #34421, .F. ) ;
#11645 = DIRECTION ( 'NONE',  ( -0.4999551463232372317, 0.8660512985181135770, -0.000000000000000000 ) ) ;
#11646 = ORIENTED_EDGE ( 'NONE', *, *, #22368, .F. ) ;
#11647 = CARTESIAN_POINT ( 'NONE',  ( 0.1904741123364903921, -0.6407273034312881421, 0.05501147976861575639 ) ) ;
#11648 = CARTESIAN_POINT ( 'NONE',  ( 0.3606268415227102397, -1.392835293988391232, 0.8657824657960605519 ) ) ;
#11650 = CARTESIAN_POINT ( 'NONE',  ( 0.1927077495703349297, -0.8180328145591141409, 0.2791508387892266407 ) ) ;
#11649 = FACE_OUTER_BOUND ( 'NONE', #4815, .T. ) ;
#11651 = CARTESIAN_POINT ( 'NONE',  ( 0.6952084031009919673, -1.569313059414498612, 0.5182417262812423209 ) ) ;
#11652 = ORIENTED_EDGE ( 'NONE', *, *, #21857, .F. ) ;
#11653 = CARTESIAN_POINT ( 'NONE',  ( 0.3905003066036929482, -1.793686422149088688, -0.5256265208041123183 ) ) ;
#11654 = CARTESIAN_POINT ( 'NONE',  ( 0.5817635102457460183, -1.493441422541048613, 0.6192858208287552735 ) ) ;
#11655 =( REPRESENTATION_RELATIONSHIP ('NONE','NONE', #27514, #35919 ) REPRESENTATION_RELATIONSHIP_WITH_TRANSFORMATION ( #35007 )SHAPE_REPRESENTATION_RELATIONSHIP( ) );
#11656 = CARTESIAN_POINT ( 'NONE',  ( 0.01548846960707524721, 0.3880410510314737382, -0.3755318131855000519 ) ) ;
#11657 = DIRECTION ( 'NONE',  ( 1.000000000000000000, -0.000000000000000000, -0.000000000000000000 ) ) ;
#11658 =( BOUNDED_SURFACE ( )  B_SPLINE_SURFACE ( 3, 2, ( 
 ( #13949, #29591, #7779 ),
 ( #30195, #32868, #1435 ),
 ( #29401, #38838, #2026 ),
 ( #39054, #10667, #14555 ),
 ( #27123, #10885, #35973 ),
 ( #26919, #20348, #4676 ),
 ( #39259, #11082, #23643 ),
 ( #36163, #8186, #7973 ),
 ( #33080, #17457, #20760 ),
 ( #4890, #30006, #11490 ),
 ( #24055, #36581, #20952 ),
 ( #40476, #40259, #21372 ),
 ( #18455, #2629, #12299 ),
 ( #34091, #6098, #18061 ) ),
 .UNSPECIFIED., .F., .F., .F. ) 
 B_SPLINE_SURFACE_WITH_KNOTS ( ( 4, 2, 2, 2, 2, 2, 4 ),
 ( 3, 3 ),
 ( 0.001271275560265211274, 0.001846161198739981746, 0.002133604017977366873, 0.002421046837214752001, 0.002708489656452137129, 0.002995932475689522256, 0.003570818114164292512 ),
 ( 0.000000000000000000, 1.000000000000000000 ),
 .UNSPECIFIED. ) 
 GEOMETRIC_REPRESENTATION_ITEM ( )  RATIONAL_B_SPLINE_SURFACE ( (
 ( 1.000000000000000000, 0.9128709291752991062, 1.000000000000000000),
 ( 1.000000000000000000, 0.9128716273348083110, 1.000000000000000000),
 ( 1.000000000000000000, 0.9128126260589567442, 1.000000000000000000),
 ( 1.000000000000000000, 0.9126599423561904123, 1.000000000000000000),
 ( 1.000000000000000000, 0.9125975471392260285, 1.000000000000000000),
 ( 1.000000000000000000, 0.9124617177697034176, 1.000000000000000000),
 ( 1.000000000000000000, 0.9123879986973735257, 1.000000000000000000),
 ( 1.000000000000000000, 0.9122366710451426108, 1.000000000000000000),
 ( 1.000000000000000000, 0.9121592624379696312, 1.000000000000000000),
 ( 1.000000000000000000, 0.9120163032376081835, 1.000000000000000000),
 ( 1.000000000000000000, 0.9119498413177286045, 1.000000000000000000),
 ( 1.000000000000000000, 0.9117793221099002032, 1.000000000000000000),
 ( 1.000000000000000000, 0.9117124009648843730, 1.000000000000000000),
 ( 1.000000000000000000, 0.9117127123830554014, 1.000000000000000000) ) ) 
 REPRESENTATION_ITEM ( '' )  SURFACE ( )  );
#11659 = LINE ( 'NONE', #30585, #39562 ) ;
#11660 = CARTESIAN_POINT ( 'NONE',  ( 0.2197619200132477080, -1.239992638468456310, 0.5547062449803537021 ) ) ;
#11661 = CARTESIAN_POINT ( 'NONE',  ( -0.1531325081225952400, 0.4743613400439437022, 0.3600421117866470233 ) ) ;
#11662 = CARTESIAN_POINT ( 'NONE',  ( 0.4904112910084666432, -1.188461936721600720, 0.4182417262808778013 ) ) ;
#11663 = CARTESIAN_POINT ( 'NONE',  ( 0.4199384557880279645, -0.9749410087210258480, 0.8268343460595501959 ) ) ;
#11664 = EDGE_CURVE ( 'NONE', #29794, #30904, #16420, .T. ) ;
#11665 = DIRECTION ( 'NONE',  ( -1.000000000000000000, -0.000000000000000000, -0.000000000000000000 ) ) ;
#11666 = DIRECTION ( 'NONE',  ( -0.8660512985181132439, -0.4999551463232375648, 0.000000000000000000 ) ) ;
#11667 = EDGE_CURVE ( 'NONE', #36888, #14981, #4787, .T. ) ;
#11668 = CARTESIAN_POINT ( 'NONE',  ( 0.6033773671567600472, -1.592159661714941832, -0.4857557934844767833 ) ) ;
#11669 = DIRECTION ( 'NONE',  ( 0.4999551463232372317, -0.8660512985181134660, 0.000000000000000000 ) ) ;
#11670 = CARTESIAN_POINT ( 'NONE',  ( 0.5775994654647633730, -1.623302777163974309, 0.5622733483718397318 ) ) ;
#11671 = EDGE_CURVE ( 'NONE', #5331, #38334, #31654, .T. ) ;
#11672 = CARTESIAN_POINT ( 'NONE',  ( 0.3755263365652165009, -1.754697207561586980, -0.4344311325575616611 ) ) ;
#11673 = DIRECTION ( 'NONE',  ( 8.881784197001246407E-16, -2.361472542561082612E-16, 1.000000000000000000 ) ) ;
#11674 = CARTESIAN_POINT ( 'NONE',  ( 0.1805970051927620057, -0.5031265787226441022, 0.1274127068463872803 ) ) ;
#11675 = CARTESIAN_POINT ( 'NONE',  ( 0.4052584708005012026, -1.689779467654166201, -0.6110500361598382169 ) ) ;
#11676 = DIRECTION ( 'NONE',  ( 1.000000000000000000, 6.779273404243070203E-32, 4.314083075427408311E-32 ) ) ;
#11677 = CARTESIAN_POINT ( 'NONE',  ( 5.463695987328526437E-16, -0.2899999999999993694, -7.171100983368691195E-16 ) ) ;
#11679 = ORIENTED_EDGE ( 'NONE', *, *, #22873, .F. ) ;
#11678 = B_SPLINE_SURFACE_WITH_KNOTS ( 'NONE', 5, 5, ( 
 ( #24132, #33546, #17918, #30482, #2311, #21844 ),
 ( #37051, #37259, #30692, #18337, #9266, #14851 ),
 ( #2512, #30882, #24315, #36839, #21226, #33764 ),
 ( #24521, #5973, #30262, #27803, #40339, #31090 ),
 ( #2909, #12168, #24730, #9076, #21640, #15462 ),
 ( #28011, #12367, #24923, #37450, #489, #13164 ) ),
 .UNSPECIFIED., .F., .F., .F.,
 ( 6, 6 ),
 ( 6, 6 ),
 ( -6.477000000001651436, 6.477000000001640778 ),
 ( -2.080605796196440593, 4.396394203803596135 ),
 .UNSPECIFIED. ) ;
#11680 = CARTESIAN_POINT ( 'NONE',  ( 0.4679018147548930084, -1.094320404139347058, -0.6313355493825376641 ) ) ;
#11681 = EDGE_CURVE ( 'NONE', #7026, #4884, #3475, .T. ) ;
#11682 = ORIENTED_EDGE ( 'NONE', *, *, #11263, .T. ) ;
#11683 = CARTESIAN_POINT ( 'NONE',  ( -19685.04193433331602, 285.7890798983738136, -1.951739244310253252 ) ) ;
#11684 = APPROVAL ( #7331, 'UNSPECIFIED' ) ;
#11685 = CARTESIAN_POINT ( 'NONE',  ( -0.03650581953630684107, 0.3643937567481969619, -0.3592734714612021429 ) ) ;
#11686 = CARTESIAN_POINT ( 'NONE',  ( 0.5211427556806288441, -1.328754734744161503, 0.6184543104854637319 ) ) ;
#11688 = ORIENTED_EDGE ( 'NONE', *, *, #12008, .F. ) ;
#11687 = DIRECTION ( 'NONE',  ( 1.000000000000000000, 1.998486013202558684E-12, 1.557674999835062714E-12 ) ) ;
#11689 = CARTESIAN_POINT ( 'NONE',  ( 0.5127940875192875669, -1.116701596374397587, 0.5863938561526392812 ) ) ;
#11690 = ORIENTED_EDGE ( 'NONE', *, *, #35806, .F. ) ;
#11691 = CARTESIAN_POINT ( 'NONE',  ( 0.07195434016001761579, -1.416717534487766272, -0.3655371694413775963 ) ) ;
#11692 = EDGE_LOOP ( 'NONE', ( #33630, #1290, #18974, #30795 ) ) ;
#11693 = CARTESIAN_POINT ( 'NONE',  ( -0.04229956186878654906, 0.2683474741743145375, -0.3842687663629381079 ) ) ;
#11694 = EDGE_LOOP ( 'NONE', ( #36625, #27985, #40625, #26777 ) ) ;
#11695 = CARTESIAN_POINT ( 'NONE',  ( 0.03624043082992319670, -0.5539225501819573516, 0.2410209412657329242 ) ) ;
#11697 = FACE_OUTER_BOUND ( 'NONE', #28880, .T. ) ;
#11696 = CARTESIAN_POINT ( 'NONE',  ( 0.7001105832783358629, -1.490154023927230620, 0.4954520656533412670 ) ) ;
#11698 = DIRECTION ( 'NONE',  ( -0.8660512985181130219, -0.4999551463232378978, 0.000000000000000000 ) ) ;
#11699 = ORIENTED_EDGE ( 'NONE', *, *, #15243, .F. ) ;
#11700 = ORIENTED_EDGE ( 'NONE', *, *, #4205, .T. ) ;
#11701 = CARTESIAN_POINT ( 'NONE',  ( 0.4091989031083814732, -1.120218831783651225, 0.6059596497380331792 ) ) ;
#11702 = VERTEX_POINT ( 'NONE', #28776 ) ;
#11703 = FACE_OUTER_BOUND ( 'NONE', #6045, .T. ) ;
#11704 = DIRECTION ( 'NONE',  ( 0.2828184691483936475, -0.9591734532964092397, 4.074771315709934095E-15 ) ) ;
#11705 = CARTESIAN_POINT ( 'NONE',  ( 0.2618259362272229440, -1.171708162254243346, 0.7401477599866793655 ) ) ;
#11706 = CYLINDRICAL_SURFACE ( 'NONE', #4056, 0.03749999999977557397 ) ;
#11707 = CARTESIAN_POINT ( 'NONE',  ( -0.1572280491643743283, 0.4879031095700123721, 0.3568535915792940827 ) ) ;
#11708 = DIRECTION ( 'NONE',  ( 0.8733930460526325712, 0.4870160029269101076, 1.225071845210601238E-12 ) ) ;
#11709 = EDGE_CURVE ( 'NONE', #1249, #9291, #1546, .T. ) ;
#11710 = DIRECTION ( 'NONE',  ( -1.000000000000000000, -6.779273404243070203E-32, -4.314083075427408311E-32 ) ) ;
#11711 = CARTESIAN_POINT ( 'NONE',  ( 0.3665423450487189094, -1.157372158458239930, 0.4269203576084827367 ) ) ;
#11712 = CARTESIAN_POINT ( 'NONE',  ( -0.2746410161513779258, -3.941790907013290823, 0.1405840032208834911 ) ) ;
#11713 = DIRECTION ( 'NONE',  ( 1.000000000000000000, 0.000000000000000000, 0.000000000000000000 ) ) ;
#11714 = APPLICATION_PROTOCOL_DEFINITION ( 'international standard', 'automotive_design', 2000, #12985 ) ;
#11715 = EDGE_CURVE ( 'NONE', #15152, #4767, #29770, .T. ) ;
#11716 = CARTESIAN_POINT ( 'NONE',  ( 0.4853835224616649957, -1.121831837822684363, 0.5320487966727919238 ) ) ;
#11717 = EDGE_CURVE ( 'NONE', #8537, #2630, #23015, .T. ) ;
#11718 = CARTESIAN_POINT ( 'NONE',  ( 0.4669913346123752418, -1.236372280561029768, 0.6057417262809813296 ) ) ;
#11719 = AXIS2_PLACEMENT_3D ( 'NONE', #4584, #20261, #7479 ) ;
#11720 = CARTESIAN_POINT ( 'NONE',  ( 0.01548846960707511190, -0.5198120922912221609, 0.07362328916738264395 ) ) ;
#11721 = CARTESIAN_POINT ( 'NONE',  ( 0.0003234651869381446995, -0.4702172293755216281, 0.02383708635093780698 ) ) ;
#11722 = CARTESIAN_POINT ( 'NONE',  ( -0.2399999999999999079, -2.853330612949663170, -0.7688139570729241035 ) ) ;
#11723 = CARTESIAN_POINT ( 'NONE',  ( 0.01853211186653049014, -0.5933771545062531683, 0.5476569912671933604 ) ) ;
#11724 = CARTESIAN_POINT ( 'NONE',  ( -0.02000000000000000042, -1.546789565643408526, -0.06332195561662121164 ) ) ;
#11725 = ORIENTED_EDGE ( 'NONE', *, *, #12014, .T. ) ;
#11726 = EDGE_LOOP ( 'NONE', ( #36015, #21000, #37913, #3188 ) ) ;
#11727 = EDGE_CURVE ( 'NONE', #10166, #22691, #35156, .T. ) ;
#11728 = CARTESIAN_POINT ( 'NONE',  ( -0.1171721259116252079, -0.4872713820691122466, 0.1209876223252399491 ) ) ;
#11729 = VERTEX_POINT ( 'NONE', #19709 ) ;
#11730 = CARTESIAN_POINT ( 'NONE',  ( 0.4256128369825924462, -1.668893475541606053, -0.3965718019701741093 ) ) ;
#11732 = VERTEX_POINT ( 'NONE', #32241 ) ;
#11731 = CARTESIAN_POINT ( 'NONE',  ( -0.1129900121204075181, -0.5167580615069143901, 0.1415474730881016441 ) ) ;
#11734 = VERTEX_POINT ( 'NONE', #4061 ) ;
#11733 = DIRECTION ( 'NONE',  ( 0.9378410757839521494, 0.2807814858886644171, -0.2039996905746503109 ) ) ;
#11735 = ORIENTED_EDGE ( 'NONE', *, *, #17502, .T. ) ;
#11736 = DIRECTION ( 'NONE',  ( 0.000000000000000000, 0.9672079024885570364, 0.2539859708009205019 ) ) ;
#11737 = VERTEX_POINT ( 'NONE', #16628 ) ;
#11738 = CARTESIAN_POINT ( 'NONE',  ( 0.2665790487942257814, -1.675396594968343589, 0.5762402978905174500 ) ) ;
#11740 = CARTESIAN_POINT ( 'NONE',  ( 0.1548133193268841079, -1.266291356060329942, 0.6052138703867981917 ) ) ;
#11739 = CARTESIAN_POINT ( 'NONE',  ( 0.1834964085430285941, -1.226715333008844055, -0.5155029497116575543 ) ) ;
#11741 = CARTESIAN_POINT ( 'NONE',  ( 0.3924513946351673721, -1.141110873382124913, 0.4807468720547258823 ) ) ;
#11742 = DATE_AND_TIME ( #20819, #37233 ) ;
#11743 = DIRECTION ( 'NONE',  ( 0.000000000000000000, -0.9510565162951422069, 0.3090169943749823678 ) ) ;
#11745 = ORIENTED_EDGE ( 'NONE', *, *, #39859, .F. ) ;
#11744 = ORIENTED_EDGE ( 'NONE', *, *, #5903, .T. ) ;
#11746 = CARTESIAN_POINT ( 'NONE',  ( 0.3546663891935897261, -1.141357238359193227, 0.6167818336462109752 ) ) ;
#11747 = CARTESIAN_POINT ( 'NONE',  ( -0.04139678531769439007, -0.4525211694413290853, 0.1291682248591894677 ) ) ;
#11748 = CARTESIAN_POINT ( 'NONE',  ( 0.2963953263377933633, -0.9883368321787951993, 0.7520588641002025065 ) ) ;
#11749 = CARTESIAN_POINT ( 'NONE',  ( 0.1862608185035845298, -0.7716910769734633968, 0.05026386998840438880 ) ) ;
#11750 = CARTESIAN_POINT ( 'NONE',  ( -2.128280327564064936E-14, -2.101101183304413311, -0.6980525384215444662 ) ) ;
#11751 = CARTESIAN_POINT ( 'NONE',  ( -0.1167294259372891468, -0.5331983348239500708, 0.1528658435937000626 ) ) ;
#11752 = CARTESIAN_POINT ( 'NONE',  ( 0.4144479545766268647, -1.706837603466250686, -0.4202405736507541789 ) ) ;
#11753 = CARTESIAN_POINT ( 'NONE',  ( 0.3938619850121877763, -1.751888204654250325, -0.5728934638734284324 ) ) ;
#11754 = CARTESIAN_POINT ( 'NONE',  ( 5.463695987328526437E-16, -0.2899999999999993694, -7.171100983368691195E-16 ) ) ;
#11755 = LINE ( 'NONE', #30080, #36953 ) ;
#11756 = EDGE_CURVE ( 'NONE', #12799, #35807, #36342, .T. ) ;
#11757 = DIRECTION ( 'NONE',  ( -1.000000000000000000, -6.779273404243070203E-32, -4.314083075427408311E-32 ) ) ;
#11758 = CARTESIAN_POINT ( 'NONE',  ( 0.4438204728424792744, -1.112778709206400540, 0.5971037950205706490 ) ) ;
#11759 = CARTESIAN_POINT ( 'NONE',  ( -0.02953079040095707777, -0.5250338024619269905, -0.07436286310882420092 ) ) ;
#11760 = DIRECTION ( 'NONE',  ( 0.000000000000000000, 0.000000000000000000, 1.000000000000000000 ) ) ;
#11761 = ADVANCED_FACE ( 'NONE', ( #14342 ), #13205, .T. ) ;
#11762 = CARTESIAN_POINT ( 'NONE',  ( 0.01899496522504870444, -0.2428513482851170358, 0.4597779644694723333 ) ) ;
#11763 = CARTESIAN_POINT ( 'NONE',  ( 0.02434420200121316033, -0.6484821100597173427, 0.5849520929678148073 ) ) ;
#11764 = CARTESIAN_POINT ( 'NONE',  ( 0.1499999999999994671, 0.3772621329472654605, -0.3651003739303476658 ) ) ;
#11765 = SECURITY_CLASSIFICATION_LEVEL ( 'unclassified' ) ;
#11766 = CARTESIAN_POINT ( 'NONE',  ( 0.6005716857727874114, -1.273429356927226364, 0.8451723082856259506 ) ) ;
#11767 = DIRECTION ( 'NONE',  ( 1.000000000000000000, 0.000000000000000000, 0.000000000000000000 ) ) ;
#11768 = CARTESIAN_POINT ( 'NONE',  ( 0.02872242845529800886, 0.07817994906157710311, -0.5268390348591307504 ) ) ;
#11769 = CARTESIAN_POINT ( 'NONE',  ( 0.3500164589514257463, -1.719894267657803733, -0.4370873290842924308 ) ) ;
#11770 = ORIENTED_EDGE ( 'NONE', *, *, #25390, .F. ) ;
#11771 = FACE_OUTER_BOUND ( 'NONE', #16700, .T. ) ;
#11772 = CARTESIAN_POINT ( 'NONE',  ( 0.02531197093827743799, -0.7324061903732035361, 0.5907467694136248060 ) ) ;
#11773 = EDGE_CURVE ( 'NONE', #12086, #14616, #35699, .T. ) ;
#11774 = APPROVAL ( #11133, 'UNKNOWN' ) ;
#11775 = CARTESIAN_POINT ( 'NONE',  ( 0.1660212896393471194, -0.7004965508887009973, 0.4943758604162845627 ) ) ;
#11776 = CARTESIAN_POINT ( 'NONE',  ( 0.3695052819757338458, -1.758428263776098621, -0.4278193900811942396 ) ) ;
#11778 = ORIENTED_EDGE ( 'NONE', *, *, #5958, .F. ) ;
#11777 = CARTESIAN_POINT ( 'NONE',  ( 0.3923243630925575820, -1.966611948492509088, -0.4968729097669151162 ) ) ;
#11779 = EDGE_CURVE ( 'NONE', #40488, #21878, #20346, .T. ) ;
#11780 = CARTESIAN_POINT ( 'NONE',  ( 0.3136035985995381248, -0.8251737266935038617, 0.6634070228338775355 ) ) ;
#11782 = VERTEX_POINT ( 'NONE', #33061 ) ;
#11781 = VERTEX_POINT ( 'NONE', #20331 ) ;
#11783 = CARTESIAN_POINT ( 'NONE',  ( 0.1809287994913508502, -1.262837545876213108, -0.7414037396183945638 ) ) ;
#11784 = CARTESIAN_POINT ( 'NONE',  ( 0.4356662251172991329, -1.610775558009423847, -0.3686272921855576756 ) ) ;
#11785 = DIRECTION ( 'NONE',  ( -0.8660512985181135770, -0.4999551463232371207, 0.000000000000000000 ) ) ;
#11786 = DATE_TIME_ROLE ( 'classification_date' ) ;
#11787 = SPHERICAL_SURFACE ( 'NONE', #40156, 0.01499999999999999944 ) ;
#11788 = ORIENTED_EDGE ( 'NONE', *, *, #38315, .F. ) ;
#11789 = CARTESIAN_POINT ( 'NONE',  ( 0.1308037668030993250, -0.7698811990532283822, 0.4769619041194265163 ) ) ;
#11790 = CARTESIAN_POINT ( 'NONE',  ( -0.01548846960707524721, 0.3772621329472709006, 0.3651003739303413931 ) ) ;
#11791 = CARTESIAN_POINT ( 'NONE',  ( 0.4986356724744993030, -1.542411423100964685, 0.5955585433317269750 ) ) ;
#11793 = CARTESIAN_POINT ( 'NONE',  ( 0.001416521061405088058, -0.5542609177154461664, 0.04326317503830075240 ) ) ;
#11792 = CARTESIAN_POINT ( 'NONE',  ( 0.3387747544451191195, -1.750987805599188762, 0.4530632734751737778 ) ) ;
#11794 = CARTESIAN_POINT ( 'NONE',  ( 0.03379672557156814666, -1.165057834625447430, 0.6664856670883784195 ) ) ;
#11795 = VERTEX_POINT ( 'NONE', #27104 ) ;
#11796 = ORIENTED_EDGE ( 'NONE', *, *, #7930, .T. ) ;
#11797 = CARTESIAN_POINT ( 'NONE',  ( -0.01548846960707524721, 0.000000000000000000, 0.000000000000000000 ) ) ;
#11798 = CARTESIAN_POINT ( 'NONE',  ( 0.5942568569871560236, -1.385430782096122915, 0.8695712771822926568 ) ) ;
#11799 = CARTESIAN_POINT ( 'NONE',  ( 0.4686299618660970667, -1.116544485314582058, 0.5688522617922341373 ) ) ;
#11800 = EDGE_CURVE ( 'NONE', #29395, #23547, #32853, .T. ) ;
#11801 = CARTESIAN_POINT ( 'NONE',  ( 0.3791158569359883712, -1.152399346284787240, 0.4250371444196747728 ) ) ;
#11802 = FACE_OUTER_BOUND ( 'NONE', #34541, .T. ) ;
#11803 = EDGE_CURVE ( 'NONE', #1288, #13846, #27194, .T. ) ;
#11804 = CARTESIAN_POINT ( 'NONE',  ( 0.3187440932968347851, -1.183579951292570431, 0.5368940269945723376 ) ) ;
#11805 = CARTESIAN_POINT ( 'NONE',  ( 0.5416676161616581497, -1.167047932790743037, 0.6420073683128293407 ) ) ;
#11806 = PERSON ( 'NAUO-PER17', 'UNSPECIFIED', 'UNSPECIFIED', ('UNSPECIFIED'), ('UNSPECIFIED'), ('UNSPECIFIED') ) ;
#11807 = PERSON_AND_ORGANIZATION ( #28500, #32463 ) ;
#11808 = CARTESIAN_POINT ( 'NONE',  ( 0.6280011288705396044, -1.582389882725783403, 0.6191887264445070649 ) ) ;
#11809 = CARTESIAN_POINT ( 'NONE',  ( 0.4030327056921976792, -1.680968334469209680, -0.4031266960524464982 ) ) ;
#11810 = DIRECTION ( 'NONE',  ( 0.8660512985181125778, 0.4999551463232387860, 0.000000000000000000 ) ) ;
#11811 = CARTESIAN_POINT ( 'NONE',  ( -0.04285561529641390005, -0.3459893009864985491, -0.3537429040513713763 ) ) ;
#11812 = ORIENTED_EDGE ( 'NONE', *, *, #31189, .F. ) ;
#11813 = CARTESIAN_POINT ( 'NONE',  ( -0.1210148435730249716, -0.5061394519557976812, 0.3122829191278992389 ) ) ;
#11814 = CIRCLE ( 'NONE', #17166, 0.5088493849861025486 ) ;
#11815 = CARTESIAN_POINT ( 'NONE',  ( -0.2399999999999999079, -3.904891172116972786, -0.3813182129431079148 ) ) ;
#11816 = ORIENTED_EDGE ( 'NONE', *, *, #8783, .F. ) ;
#11817 = CARTESIAN_POINT ( 'NONE',  ( -0.04762200653274617501, -0.04294689284307315336, -0.4802757286814972049 ) ) ;
#11818 = CARTESIAN_POINT ( 'NONE',  ( 0.06533280422175168078, -0.9217453127808572511, 0.5945887534868308233 ) ) ;
#11820 = ORIENTED_EDGE ( 'NONE', *, *, #13972, .F. ) ;
#11819 = ORIENTED_EDGE ( 'NONE', *, *, #28653, .F. ) ;
#11821 = CARTESIAN_POINT ( 'NONE',  ( 0.03309060444528774680, 0.3730661130945450155, 0.3633899800202370911 ) ) ;
#11822 = AXIS2_PLACEMENT_3D ( 'NONE', #32909, #7618, #32712 ) ;
#11823 = CARTESIAN_POINT ( 'NONE',  ( 0.3048982267989297501, -1.756746414302344350, 0.5594309555313059512 ) ) ;
#11824 = CARTESIAN_POINT ( 'NONE',  ( 0.05269111014006322424, -0.4428579967164673614, -0.1534656216456658784 ) ) ;
#11825 = CARTESIAN_POINT ( 'NONE',  ( 0.3686706805007330390, -2.055989704601955292, -0.4776676948433997705 ) ) ;
#11826 = CARTESIAN_POINT ( 'NONE',  ( 0.3392040500280487647, -1.075138255607900994, 0.7131914377028192309 ) ) ;
#11827 = ADVANCED_FACE ( 'NONE', ( #18248 ), #37173, .T. ) ;
#11829 = CARTESIAN_POINT ( 'NONE',  ( -0.0003416957584554876381, -0.9395563572588278012, 0.1457085237891919405 ) ) ;
#11828 = CARTESIAN_POINT ( 'NONE',  ( 0.05615703521555099470, 0.4399943745474645951, 0.1321275321584946816 ) ) ;
#11830 = CARTESIAN_POINT ( 'NONE',  ( 0.1999999999999789724, -2.166079853131637645, -0.4467913981637917087 ) ) ;
#11831 = ORIENTED_EDGE ( 'NONE', *, *, #7909, .F. ) ;
#11832 = EDGE_LOOP ( 'NONE', ( #28186, #9334, #4677, #26353 ) ) ;
#11833 = CARTESIAN_POINT ( 'NONE',  ( -0.3000000000000000999, -3.335205990917129881, -0.4042613180508735082 ) ) ;
#11834 = ORIENTED_EDGE ( 'NONE', *, *, #15702, .F. ) ;
#11835 = CARTESIAN_POINT ( 'NONE',  ( 0.1854056692992981370, -0.7337134285967986669, 0.008518417185872215538 ) ) ;
#11836 = CARTESIAN_POINT ( 'NONE',  ( 0.4195515592568131447, -1.516513744509174977, 0.7855708791636160093 ) ) ;
#11838 = CARTESIAN_POINT ( 'NONE',  ( 0.5835029919942696930, -1.605605060618692459, 0.4537850722327775865 ) ) ;
#11837 = FACE_OUTER_BOUND ( 'NONE', #29789, .T. ) ;
#11839 = CARTESIAN_POINT ( 'NONE',  ( 0.4148946963616447769, -1.144346411133103869, 0.4245081400086456180 ) ) ;
#11840 = EDGE_LOOP ( 'NONE', ( #20435, #40056, #34076, #16751 ) ) ;
#11841 = DIRECTION ( 'NONE',  ( 0.000000000000000000, 0.000000000000000000, -1.000000000000000000 ) ) ;
#11842 = ORIENTED_EDGE ( 'NONE', *, *, #14862, .T. ) ;
#11843 = CARTESIAN_POINT ( 'NONE',  ( 0.1913042973830217097, -1.953999136512327039, -0.2983785852701217323 ) ) ;
#11844 = CARTESIAN_POINT ( 'NONE',  ( 0.1594335956643706809, -0.7007958973334156294, 0.4972769676686734641 ) ) ;
#11845 = CARTESIAN_POINT ( 'NONE',  ( 0.4829940418909406952, -1.675148570078003551, 0.5372820393660157068 ) ) ;
#11846 = CARTESIAN_POINT ( 'NONE',  ( -0.05464101615137785528, -2.180132361182266720, -0.6941833704005058170 ) ) ;
#11847 = FACE_OUTER_BOUND ( 'NONE', #26699, .T. ) ;
#11848 = CARTESIAN_POINT ( 'NONE',  ( 0.4861231359011924380, -1.648611998150725899, 0.4182417262808776348 ) ) ;
#11849 = AXIS2_PLACEMENT_3D ( 'NONE', #32461, #33074, #7966 ) ;
#11850 = CARTESIAN_POINT ( 'NONE',  ( -0.1508044614562676355, 0.4665164580004940720, 0.3602693336111439382 ) ) ;
#11851 = CARTESIAN_POINT ( 'NONE',  ( -0.08000000000000000167, -1.984114763688379579, -0.7731012124309359912 ) ) ;
#11852 = CARTESIAN_POINT ( 'NONE',  ( 0.1927903040881008279, -0.5292341811144671837, 0.2767179517167643321 ) ) ;
#11853 = AXIS2_PLACEMENT_3D ( 'NONE', #4935, #20995, #5132 ) ;
#11854 = CARTESIAN_POINT ( 'NONE',  ( -0.05489899477340535322, 0.2510719788555840215, 0.3887182106515215674 ) ) ;
#11855 = FACE_OUTER_BOUND ( 'NONE', #13881, .T. ) ;
#11856 = B_SPLINE_CURVE_WITH_KNOTS ( 'NONE', 3,
 ( #27799, #2904, #9472, #9072, #5968, #15850, #40333, #15457, #37657, #12164 ),
 .UNSPECIFIED., .F., .F.,
 ( 4, 2, 2, 2, 4 ),
 ( 0.000000000000000000, 0.0005579115002213586028, 0.001115823000442717206, 0.001673734500664075808, 0.002231646000885434411 ),
 .UNSPECIFIED. ) ;
#11857 = CARTESIAN_POINT ( 'NONE',  ( 0.6253075507800407440, -1.612178444674642108, -0.4646957544917997840 ) ) ;
#11858 = CARTESIAN_POINT ( 'NONE',  ( -0.2399999999999999079, -4.176085227118957022, -0.6840180543573738392 ) ) ;
#11859 = CARTESIAN_POINT ( 'NONE',  ( 0.3222810527215910770, -1.758570551863011922, 0.4849083929475442867 ) ) ;
#11860 = CARTESIAN_POINT ( 'NONE',  ( 0.4071174156400276245, -1.728162493485833284, -0.4292401697313079079 ) ) ;
#11861 = CARTESIAN_POINT ( 'NONE',  ( -0.2746410161513779258, -4.320736256378554963, -0.8145269479932405465 ) ) ;
#11862 = ORIENTED_EDGE ( 'NONE', *, *, #28072, .T. ) ;
#11863 = CARTESIAN_POINT ( 'NONE',  ( 0.3649706973906967633, -1.747755802024545835, -0.5186209711426437163 ) ) ;
#11864 = CARTESIAN_POINT ( 'NONE',  ( -0.1167294259372888832, -0.5331983348239500708, 0.1528658435937002014 ) ) ;
#11865 = CARTESIAN_POINT ( 'NONE',  ( 0.4624855077751916510, -1.656167738812893475, -0.6359952755422354498 ) ) ;
#11866 = ORIENTED_EDGE ( 'NONE', *, *, #30467, .F. ) ;
#11867 = CARTESIAN_POINT ( 'NONE',  ( 0.4209912206648682154, -1.078067379053157193, -0.5155029497116575543 ) ) ;
#11868 = CARTESIAN_POINT ( 'NONE',  ( 0.3998620935691252209, -1.132090473766684147, 0.6053150776564959479 ) ) ;
#11869 = CARTESIAN_POINT ( 'NONE',  ( 0.02999999999997886302, -2.183180860297921466, -0.7437760292030870524 ) ) ;
#11870 = DIRECTION ( 'NONE',  ( 0.4999551463232372317, -0.8660512985181135770, 0.000000000000000000 ) ) ;
#11871 = CARTESIAN_POINT ( 'NONE',  ( 0.4683334428778225811, -1.244683268694764422, 0.7181273297428137914 ) ) ;
#11872 = AXIS2_PLACEMENT_3D ( 'NONE', #37083, #8294, #17745 ) ;
#11874 = CARTESIAN_POINT ( 'NONE',  ( 0.4646886455416142647, -1.611488784964096643, -0.6527336024875409759 ) ) ;
#11873 = CARTESIAN_POINT ( 'NONE',  ( 0.05999999999999990757, 0.000000000000000000, 0.000000000000000000 ) ) ;
#11875 = CARTESIAN_POINT ( 'NONE',  ( 0.4598226378601848463, -1.064312249210862982, 0.6507415875188953258 ) ) ;
#11876 = VERTEX_POINT ( 'NONE', #9175 ) ;
#11877 = PERSON_AND_ORGANIZATION_ROLE ( 'creator' ) ;
#11878 = EDGE_CURVE ( 'NONE', #22635, #36573, #2614, .T. ) ;
#11879 = DIRECTION ( 'NONE',  ( 0.4999551463232373427, -0.8660512985181134660, 0.000000000000000000 ) ) ;
#11880 = ORIENTED_EDGE ( 'NONE', *, *, #31269, .F. ) ;
#11881 = DIRECTION ( 'NONE',  ( 1.188678714063518227E-15, -1.000000000000000000, -3.263080277421930985E-16 ) ) ;
#11882 = CIRCLE ( 'NONE', #18463, 0.07999999999999996003 ) ;
#11883 =( BOUNDED_SURFACE ( )  B_SPLINE_SURFACE ( 3, 2, ( 
 ( #10400, #22962, #16983 ),
 ( #39201, #20474, #13872 ),
 ( #23580, #26246, #13682 ),
 ( #29523, #11023, #4223 ),
 ( #29336, #36293, #26667 ),
 ( #39389, #32612, #10597 ),
 ( #5031, #26447, #17596 ),
 ( #29725, #23170, #38983 ),
 ( #35698, #14094, #8113 ),
 ( #7504, #4422, #1363 ),
 ( #17388, #23390, #35906 ),
 ( #7715, #20281, #32802 ),
 ( #36098, #7903, #4603 ),
 ( #1569, #20693, #29946 ),
 ( #1784, #14299, #11209 ),
 ( #11416, #36516, #21689 ),
 ( #6034, #15098, #33420 ),
 ( #39990, #23988, #33837 ),
 ( #5639, #1968, #11811 ),
 ( #8327, #20899, #5228 ),
 ( #14704, #40405, #17778 ),
 ( #27271, #24582, #8717 ) ),
 .UNSPECIFIED., .F., .F., .T. ) 
 B_SPLINE_SURFACE_WITH_KNOTS ( ( 4, 2, 2, 2, 2, 2, 2, 2, 2, 2, 4 ),
 ( 3, 3 ),
 ( 0.002013519961495850892, 0.002780892266055758240, 0.003548264570615666021, 0.004315636875175573803, 0.004699323027455527477, 0.005083009179735481151, 0.005466695332015434824, 0.005850381484295388498, 0.006617753788855296714, 0.007385126093415204929, 0.008152498397975112276 ),
 ( 0.000000000000000000, 1.000000000000000000 ),
 .UNSPECIFIED. ) 
 GEOMETRIC_REPRESENTATION_ITEM ( )  RATIONAL_B_SPLINE_SURFACE ( (
 ( 1.000000000000000000, 0.7283825911960389865, 1.000000000000000000),
 ( 1.000000000000000000, 0.7404375345927034502, 1.000000000000000000),
 ( 1.000000000000000000, 0.7521483142435980707, 1.000000000000000000),
 ( 1.000000000000000000, 0.7744460733776445949, 1.000000000000000000),
 ( 1.000000000000000000, 0.7845612039382956482, 1.000000000000000000),
 ( 1.000000000000000000, 0.8022035258261175361, 1.000000000000000000),
 ( 1.000000000000000000, 0.8093965293321856436, 1.000000000000000000),
 ( 1.000000000000000000, 0.8169028692725391894, 1.000000000000000000),
 ( 1.000000000000000000, 0.8188329634863381612, 1.000000000000000000),
 ( 1.000000000000000000, 0.8214004505363993180, 1.000000000000000000),
 ( 1.000000000000000000, 0.8220602406261371398, 1.000000000000000000),
 ( 1.000000000000000000, 0.8220736605435244870, 1.000000000000000000),
 ( 1.000000000000000000, 0.8214126668415641097, 1.000000000000000000),
 ( 1.000000000000000000, 0.8188520474558359519, 1.000000000000000000),
 ( 1.000000000000000000, 0.8169545908333891715, 1.000000000000000000),
 ( 1.000000000000000000, 0.8094771004220669974, 1.000000000000000000),
 ( 1.000000000000000000, 0.8022723753808039815, 1.000000000000000000),
 ( 1.000000000000000000, 0.7845733350636995285, 1.000000000000000000),
 ( 1.000000000000000000, 0.7744472902493304556, 1.000000000000000000),
 ( 1.000000000000000000, 0.7522916829163448504, 1.000000000000000000),
 ( 1.000000000000000000, 0.7403553004665824888, 1.000000000000000000),
 ( 1.000000000000000000, 0.7283825911960383204, 1.000000000000000000) ) ) 
 REPRESENTATION_ITEM ( '' )  SURFACE ( )  );
#11884 = CARTESIAN_POINT ( 'NONE',  ( 0.3561347686598763107, -1.622407662918015525, 0.5742129511320137603 ) ) ;
#11886 = CARTESIAN_POINT ( 'NONE',  ( 0.1866284055609182813, -0.6442149268503359894, -0.01633133720890060300 ) ) ;
#11885 = CARTESIAN_POINT ( 'NONE',  ( 0.3609773110263161389, -1.159644750248734590, 0.4285221785616858958 ) ) ;
#11887 = CYLINDRICAL_SURFACE ( 'NONE', #20154, 0.2200000000000000289 ) ;
#11888 = AXIS2_PLACEMENT_3D ( 'NONE', #15670, #36857, #12188 ) ;
#11889 = AXIS2_PLACEMENT_3D ( 'NONE', #36884, #2136, #18169 ) ;
#11890 = ORIENTED_EDGE ( 'NONE', *, *, #36841, .T. ) ;
#11891 = VERTEX_POINT ( 'NONE', #21556 ) ;
#11892 = CARTESIAN_POINT ( 'NONE',  ( 0.4952507122378954074, -1.106196709240402587, 0.6973901343829200794 ) ) ;
#11893 = EDGE_CURVE ( 'NONE', #8227, #34098, #38978, .T. ) ;
#11894 = CARTESIAN_POINT ( 'NONE',  ( 0.5540806847553930714, -1.510732556792533376, 0.6006766572140512794 ) ) ;
#11895 = ORIENTED_EDGE ( 'NONE', *, *, #28764, .T. ) ;
#11896 = DIRECTION ( 'NONE',  ( -0.000000000000000000, 0.8159412518334716591, 0.5781348229923772841 ) ) ;
#11897 = CARTESIAN_POINT ( 'NONE',  ( -0.05464101615137796630, -2.070343076906777213, -0.2454056712452573896 ) ) ;
#11898 = PLANE ( 'NONE',  #29709 ) ;
#11899 = CARTESIAN_POINT ( 'NONE',  ( -0.2746410161513770931, -2.891403747035983240, -0.7012825271972917829 ) ) ;
#11900 = CARTESIAN_POINT ( 'NONE',  ( 0.4284886185654731561, -1.682582563036773227, 0.4182417262808776903 ) ) ;
#11901 = CARTESIAN_POINT ( 'NONE',  ( 0.4787764723021453728, -1.660223331282874915, 0.4687417262808790119 ) ) ;
#11902 = CARTESIAN_POINT ( 'NONE',  ( -0.3000000000000000999, -2.183180860297908144, -0.4312760292030870524 ) ) ;
#11903 = EDGE_CURVE ( 'NONE', #27374, #20774, #10492, .T. ) ;
#11904 = FACE_OUTER_BOUND ( 'NONE', #36523, .T. ) ;
#11905 = LINE ( 'NONE', #24083, #19366 ) ;
#11906 = DATE_AND_TIME ( #15003, #11485 ) ;
#11907 = PRODUCT_DEFINITION ( 'UNKNOWN', '', #17475, #23273 ) ;
#11908 = AXIS2_PLACEMENT_3D ( 'NONE', #22982, #1801, #11226 ) ;
#11909 = CARTESIAN_POINT ( 'NONE',  ( 0.4521395518622611243, -1.131665481844795540, 0.4506733450461792301 ) ) ;
#11910 = AXIS2_PLACEMENT_3D ( 'NONE', #33701, #2648, #37207 ) ;
#11911 = CARTESIAN_POINT ( 'NONE',  ( 0.01548846960712800709, -0.4730347584885825629, 0.2341461249029146152 ) ) ;
#11912 = DIRECTION ( 'NONE',  ( 0.4999551463232372317, -0.8660512985181134660, 0.000000000000000000 ) ) ;
#11913 = AXIS2_PLACEMENT_3D ( 'NONE', #40007, #20913, #27288 ) ;
#11914 = VECTOR ( 'NONE', #17286, 39.37007874015748143 ) ;
#11915 = CARTESIAN_POINT ( 'NONE',  ( 6.932235465596841962E-06, -0.5784058487176239050, -0.09163823625527117711 ) ) ;
#11916 = DIRECTION ( 'NONE',  ( 0.000000000000000000, -0.8834504764630435325, -0.4685245517976845409 ) ) ;
#11917 = AXIS2_PLACEMENT_3D ( 'NONE', #35219, #38500, #19389 ) ;
#11918 = DIRECTION ( 'NONE',  ( 0.8724162812079769846, -0.4887635750373016119, 0.000000000000000000 ) ) ;
#11919 = CARTESIAN_POINT ( 'NONE',  ( -0.2746410161513779258, -3.334889855281614857, -0.6641625420049475093 ) ) ;
#11920 = EDGE_LOOP ( 'NONE', ( #16341, #35660, #3270, #21045, #34599, #36806 ) ) ;
#11921 = EDGE_LOOP ( 'NONE', ( #11282, #19013, #38537, #36025 ) ) ;
#11922 = CARTESIAN_POINT ( 'NONE',  ( 0.2411830127710683502, -1.239411202381304644, 0.4182417262808778013 ) ) ;
#11923 = VERTEX_POINT ( 'NONE', #26062 ) ;
#11924 = DIRECTION ( 'NONE',  ( 0.9480245940703959651, 0.3181970600707381691, 1.138269997360108787E-15 ) ) ;
#11925 = DIRECTION ( 'NONE',  ( 0.000000000000000000, 0.000000000000000000, -1.000000000000000000 ) ) ;
#11927 = ORIENTED_EDGE ( 'NONE', *, *, #1717, .T. ) ;
#11926 = CARTESIAN_POINT ( 'NONE',  ( 0.002241505894149531299, -0.5197024079959072784, 0.1379092258170560858 ) ) ;
#11928 = AXIS2_PLACEMENT_3D ( 'NONE', #40384, #31135, #9106 ) ;
#11929 = ORIENTED_EDGE ( 'NONE', *, *, #7465, .F. ) ;
#11930 = CARTESIAN_POINT ( 'NONE',  ( 0.02869712619511918458, 0.4892154842446461149, -0.09550911579581898569 ) ) ;
#11931 = EDGE_CURVE ( 'NONE', #3966, #32833, #34075, .T. ) ;
#11932 = ORIENTED_EDGE ( 'NONE', *, *, #38924, .F. ) ;
#11933 = CARTESIAN_POINT ( 'NONE',  ( -0.001587914043712823457, -0.5315844267872958939, 0.1859523187655416077 ) ) ;
#11935 = CARTESIAN_POINT ( 'NONE',  ( 0.1930470874137825976, -1.251549148891850205, 0.5897281480909083440 ) ) ;
#11934 = CARTESIAN_POINT ( 'NONE',  ( 0.08206746009357554494, -0.8455242767393098546, 0.3585407082876929663 ) ) ;
#11936 = DIRECTION ( 'NONE',  ( 0.4999999999999953926, 0.8179688131725333378, 0.2844767489218082979 ) ) ;
#11937 = DATE_AND_TIME ( #23903, #4368 ) ;
#11938 = EDGE_CURVE ( 'NONE', #7698, #33903, #38306, .T. ) ;
#11939 = CIRCLE ( 'NONE', #34935, 0.1600000000000004752 ) ;
#11940 = DIRECTION ( 'NONE',  ( 1.000000000000000000, 1.188678714063518030E-15, 5.551115123125745108E-17 ) ) ;
#11942 = ORIENTED_EDGE ( 'NONE', *, *, #26532, .T. ) ;
#11941 = VERTEX_POINT ( 'NONE', #27322 ) ;
#11943 = EDGE_CURVE ( 'NONE', #13608, #25709, #13357, .T. ) ;
#11944 = CARTESIAN_POINT ( 'NONE',  ( 0.01173648626945268322, -0.6872203660140956405, -0.1131804859792006068 ) ) ;
#11945 = CARTESIAN_POINT ( 'NONE',  ( 0.3527394985022780372, -1.741207400137176897, 0.4357698812951643075 ) ) ;
#11946 = CARTESIAN_POINT ( 'NONE',  ( -0.05615703521554993999, -0.4399943745474717560, 0.1321275321584853002 ) ) ;
#11947 = CARTESIAN_POINT ( 'NONE',  ( 0.5242754061866402582, -1.337501420007544795, 0.7785695029743999740 ) ) ;
#11948 = AXIS2_PLACEMENT_3D ( 'NONE', #6604, #25154, #521 ) ;
#11949 = AXIS2_PLACEMENT_3D ( 'NONE', #38756, #26659, #19855 ) ;
#11950 = CARTESIAN_POINT ( 'NONE',  ( 0.02999999999997876934, -2.097675824466503691, -0.7286991843995640483 ) ) ;
#11951 = DIRECTION ( 'NONE',  ( -3.389636702121531817E-32, 0.8709776783778059306, -0.4913225862583635584 ) ) ;
#11952 = CIRCLE ( 'NONE', #34944, 0.1400000000000005684 ) ;
#11953 = CARTESIAN_POINT ( 'NONE',  ( 0.3114014046812714209, -1.661719107297196407, 0.8995554786316910523 ) ) ;
#11954 = CARTESIAN_POINT ( 'NONE',  ( 0.4073028344303278314, -1.718531852617160682, 0.4257392557717242232 ) ) ;
#11955 = DIRECTION ( 'NONE',  ( 2.341930812374876608E-31, 0.6954292836768424246, -0.7185945389471826150 ) ) ;
#11956 = FACE_OUTER_BOUND ( 'NONE', #24146, .T. ) ;
#11957 = FACE_OUTER_BOUND ( 'NONE', #5208, .T. ) ;
#11958 = CARTESIAN_POINT ( 'NONE',  ( 0.3918182118607623221, -1.107073211027153725, 0.6042946153017959565 ) ) ;
#11959 = EDGE_CURVE ( 'NONE', #39658, #22474, #20589, .T. ) ;
#11960 = CARTESIAN_POINT ( 'NONE',  ( 0.3595715536228113463, -1.625401886829162201, -0.3696110269036072538 ) ) ;
#11961 = DIRECTION ( 'NONE',  ( -1.232595164407830946E-32, 1.110223024625156540E-16, 0.9999999999999998890 ) ) ;
#11962 = DIRECTION ( 'NONE',  ( -0.8660254037844387076, -5.423418723394462293E-31, -0.5000000000000001110 ) ) ;
#11963 = CARTESIAN_POINT ( 'NONE',  ( 0.2912354967743938094, -1.730409171686111414, 0.5958501190287942562 ) ) ;
#11964 = B_SPLINE_CURVE_WITH_KNOTS ( 'NONE', 3,
 ( #40524, #12345, #34553, #5547 ),
 .UNSPECIFIED., .F., .F.,
 ( 4, 4 ),
 ( 1.245646092707955119E-09, 0.0005051110321922458674 ),
 .UNSPECIFIED. ) ;
#11965 = CARTESIAN_POINT ( 'NONE',  ( 0.04274323293624435194, -0.9931624692768277196, 0.6843196792473072998 ) ) ;
#11966 = COORDINATED_UNIVERSAL_TIME_OFFSET ( 0, 0, .AHEAD. ) ;
#11967 = CARTESIAN_POINT ( 'NONE',  ( 0.7145247768745858208, -1.460049439684881323, 0.6872404240164239342 ) ) ;
#11968 = AXIS2_PLACEMENT_3D ( 'NONE', #24515, #9258, #34580 ) ;
#11969 = CARTESIAN_POINT ( 'NONE',  ( 0.7054299102235100927, -1.513544197856392826, 0.5664287308913636965 ) ) ;
#11970 = CARTESIAN_POINT ( 'NONE',  ( 0.04047043078435642177, 0.06271696546453996157, -0.4973274026419952643 ) ) ;
#11971 = AXIS2_PLACEMENT_3D ( 'NONE', #21444, #5775, #30876 ) ;
#11972 = CIRCLE ( 'NONE', #36960, 0.08000000000000000167 ) ;
#11973 = ORIENTED_EDGE ( 'NONE', *, *, #32320, .T. ) ;
#11974 = CARTESIAN_POINT ( 'NONE',  ( 0.05999999999999990757, 0.000000000000000000, 0.2000000000000000111 ) ) ;
#11975 = ORIENTED_EDGE ( 'NONE', *, *, #11803, .F. ) ;
#11976 = CARTESIAN_POINT ( 'NONE',  ( 0.1399999999999994582, 0.000000000000000000, 0.000000000000000000 ) ) ;
#11977 = CARTESIAN_POINT ( 'NONE',  ( 0.2619807479409076434, -1.590845703386517096, 0.8456310547791294763 ) ) ;
#11978 = VECTOR ( 'NONE', #34036, 39.37007874015748143 ) ;
#11979 = CARTESIAN_POINT ( 'NONE',  ( 0.5070218031793033431, -1.372995523392680273, 0.8015102820899869807 ) ) ;
#11981 = VERTEX_POINT ( 'NONE', #5478 ) ;
#11980 = DIRECTION ( 'NONE',  ( 1.000000000000000000, 2.280301054154496446E-31, 1.355854680848613603E-31 ) ) ;
#11982 = CARTESIAN_POINT ( 'NONE',  ( 0.6149708076787919753, -1.290796914294373154, 0.6294291921256529587 ) ) ;
#11984 = ORIENTED_EDGE ( 'NONE', *, *, #16729, .F. ) ;
#11983 = EDGE_LOOP ( 'NONE', ( #35805, #15396, #16946, #28837 ) ) ;
#11985 = CARTESIAN_POINT ( 'NONE',  ( 0.6985364634159124675, -1.438850461896725275, 0.5682400285031795617 ) ) ;
#11986 = EDGE_CURVE ( 'NONE', #17567, #2349, #32400, .T. ) ;
#11987 = CARTESIAN_POINT ( 'NONE',  ( 0.3699999999999786793, -2.183180860297921466, -0.4937760292030871079 ) ) ;
#11988 = CARTESIAN_POINT ( 'NONE',  ( 0.05999999999999990757, 0.5632502439596359656, -0.2139757610878384453 ) ) ;
#11989 = APPROVAL_DATE_TIME ( #15076, #32756 ) ;
#11990 = ADVANCED_FACE ( 'NONE', ( #18440 ), #12710, .T. ) ;
#11991 = VERTEX_POINT ( 'NONE', #24641 ) ;
#11992 = EDGE_CURVE ( 'NONE', #2621, #34142, #40460, .T. ) ;
#11993 = CARTESIAN_POINT ( 'NONE',  ( 0.09613268118642956384, -0.7396151843482207111, 0.3087118449850515534 ) ) ;
#11994 = CARTESIAN_POINT ( 'NONE',  ( 0.3253043410525603418, -1.741901272161220149, 0.7439933838227589247 ) ) ;
#11995 = CARTESIAN_POINT ( 'NONE',  ( 0.1241130014567568551, -0.6538280912446031712, 0.4339932856162626029 ) ) ;
#11997 = CARTESIAN_POINT ( 'NONE',  ( -0.1157923916715208196, -0.5295015842444287246, 0.1380392329925462791 ) ) ;
#11996 = DIRECTION ( 'NONE',  ( 0.000000000000000000, -0.3090169943749375148, 0.9510565162951567508 ) ) ;
#11998 = CARTESIAN_POINT ( 'NONE',  ( 0.002016835409016338402, -0.9611306028646753319, 0.3504772518132928116 ) ) ;
#11999 = EDGE_LOOP ( 'NONE', ( #32081, #37842, #33030, #32523 ) ) ;
#12000 = EDGE_CURVE ( 'NONE', #34243, #13895, #6082, .T. ) ;
#12001 = ORIENTED_EDGE ( 'NONE', *, *, #23266, .T. ) ;
#12002 = CIRCLE ( 'NONE', #4088, 0.1000000000000000194 ) ;
#12003 = CARTESIAN_POINT ( 'NONE',  ( -0.1670982076487675938, 0.5191099701766059837, 0.1307156235296929869 ) ) ;
#12004 = CARTESIAN_POINT ( 'NONE',  ( 0.6448553937467123021, -1.345730860570678589, 0.8527667722720939647 ) ) ;
#12005 = CARTESIAN_POINT ( 'NONE',  ( 0.000000000000000000, 0.000000000000000000, 0.000000000000000000 ) ) ;
#12006 = AXIS2_PLACEMENT_3D ( 'NONE', #32392, #35294, #4216 ) ;
#12007 = AXIS2_PLACEMENT_3D ( 'NONE', #8519, #21084, #33610 ) ;
#12008 = EDGE_CURVE ( 'NONE', #19840, #37283, #18613, .T. ) ;
#12009 = LINE ( 'NONE', #34013, #14027 ) ;
#12010 = DIRECTION ( 'NONE',  ( 0.4999999999999982792, 0.6484591962157929546, 0.5740214898792285192 ) ) ;
#12011 = EDGE_CURVE ( 'NONE', #12860, #29794, #23214, .T. ) ;
#12012 = CIRCLE ( 'NONE', #10044, 0.01499999999999995087 ) ;
#12013 = CARTESIAN_POINT ( 'NONE',  ( 0.3740960844805631957, -1.108072201694596526, 0.5182417262812423209 ) ) ;
#12014 = EDGE_CURVE ( 'NONE', #19186, #5500, #6113, .T. ) ;
#12015 = CARTESIAN_POINT ( 'NONE',  ( 0.000000000000000000, -0.03575622569115821658, -0.2978615321325044363 ) ) ;
#12016 = CARTESIAN_POINT ( 'NONE',  ( 0.3412847681102941233, -1.170475593325866592, 0.4399642596021446916 ) ) ;
#12017 = CARTESIAN_POINT ( 'NONE',  ( 0.2256328605772283669, -0.7491591359250245885, 0.4461645245400559512 ) ) ;
#12018 = B_SPLINE_SURFACE_WITH_KNOTS ( 'NONE', 3, 3, ( 
 ( #34579, #28404, #18746, #31299, #9257, #9471, #40541, #31689, #9686, #671, #6384, #28007, #19362, #3511, #16066, #64, #6572, #31487, #3294, #12768, #28614, #5967, #18528, #2903, #21838, #484, #15651, #3108, #272, #25330, #12980, #31899, #22253, #28200, #22445, #25531, #34975, #3718, #7176, #32280, #19744, #26149, #29821, #865, #38471, #7595, #32485, #20363, #1659, #4695, #32696, #17267 ),
 ( #26331, #1264, #6994, #35576, #13372, #25946, #13584, #10687, #10305, #32886, #25724, #38257, #22869, #29212, #4098, #38855, #10484, #16665, #1074, #38664, #23260, #35386, #35784, #7795, #20170, #23049, #29417, #10086, #13766, #22658, #4501, #17064, #35193, #39076, #19564, #29610, #4311, #7377, #1452, #32094, #13967, #19953, #26539, #3902, #10902, #16458, #23473, #35988, #29000, #16877, #5517, #39887 ),
 ( #26934, #24261, #30210, #14370, #23658, #17862, #17474, #2459, #39467, #33301, #36599, #30427, #2255, #2041, #30028, #18080, #5108, #27143, #36784, #21170, #26746, #1855, #8402, #11292, #14573, #23863, #27548, #20972, #33704, #30633, #36387, #14181, #8203, #39673, #11705, #7989, #4906, #14794, #8597, #11508, #36180, #27358, #20777, #17663, #24073, #33490, #14995, #20568, #39275, #11098, #33099, #5297 ),
 ( #29345, #19667, #4018, #29953, #10604, #14303, #23399, #989, #16797, #7513, #32204, #1373, #29530, #13880, #10217, #20092, #35310, #16582, #29130, #13505, #26069, #22968, #7910, #38586, #16990, #22785, #26257, #23178, #1790, #39208, #35916, #26454, #33016, #14100, #10409, #38773, #35489, #26674, #13689, #7295, #29731, #26865, #19871, #38992, #32408, #4231, #7098, #1188, #11029, #35706, #32621, #23586 ),
 ( #4431, #10824, #7722, #20289, #32809, #4611, #36104, #4821, #20481, #17187, #1577, #17393, #17600, #33425, #33230, #8334, #11818, #5232, #21093, #8123, #30144, #23781, #5834, #5647, #14492, #27060, #39590, #11424, #36299, #8941, #39997, #15320, #36522, #33618, #20698, #27275, #39394, #23994, #11215, #34032, #5038, #30341, #1973, #11634, #20903, #17785, #2172, #24192, #30554, #14712, #39808, #36715 ),
 ( #21305, #24379, #30947, #8525, #5428, #21517, #18201, #30751, #17994, #36915, #2375, #14918, #27472, #2570, #8727, #18394, #33845, #15105, #27666, #40198, #12032, #24594, #37128, #2771, #38129, #34647, #28084, #552, #37732, #3581, #34231, #9333, #34441, #21914, #28265, #31969, #2982, #40612, #9749, #6448, #22520, #3786, #6857, #34836, #19435, #25600, #27877, #28469, #3367, #9130, #9554, #15532 ),
 ( #12847, #12428, #35045, #40414, #12240, #24978, #31372, #6257, #344, #12624, #18828, #3176, #130, #25408, #37511, #37939, #9952, #22320, #25188, #31550, #24802, #15922, #37321, #15717, #22131, #19019, #6647, #19221, #31761, #21697, #16147, #28685, #13048, #6041, #18609, #31169, #19109, #22007, #31856, #16412, #12722, #32235, #22405, #22616, #37827, #28955, #38024, #9643, #34532, #10042, #28358, #4054 ) ),
 .UNSPECIFIED., .F., .F., .F.,
 ( 4, 3, 4 ),
 ( 4, 3, 3, 3, 3, 3, 3, 3, 3, 3, 3, 3, 3, 3, 3, 3, 3, 4 ),
 ( 0.2346985215076158870, 0.6110997835933865696, 0.9875010456791571967 ),
 ( -7.634747961624772664E-15, 0.1249999999999946293, 0.2499999999999968914, 0.3749999999999991673, 0.4375000000000003331, 0.5000000000000014433, 0.5625000000000026645, 0.6250000000000037748, 0.6875000000000048850, 0.7500000000000059952, 0.8125000000000071054, 0.8437500000000076605, 0.8750000000000082157, 0.9062500000000087708, 0.9375000000000093259, 0.9687500000000098810, 0.9843750000000102141, 1.000000000000010436 ),
 .UNSPECIFIED. ) ;
#12019 = PERSON_AND_ORGANIZATION_ROLE ( 'design_supplier' ) ;
#12020 = ADVANCED_FACE ( 'NONE', ( #37364 ), #14671, .T. ) ;
#12021 = CARTESIAN_POINT ( 'NONE',  ( 0.05999999999999990757, 0.2954784694557334168, 0.05188905557145093855 ) ) ;
#12022 = TOROIDAL_SURFACE ( 'NONE', #17274, 0.2200000000000000566, 0.02999999999999999889 ) ;
#12023 = CARTESIAN_POINT ( 'NONE',  ( 0.1894590026941424810, -1.967797451371194439, -0.6662202007303367202 ) ) ;
#12024 = CARTESIAN_POINT ( 'NONE',  ( 0.05999999999999990757, 0.1969856463038233696, 0.03459270371430114843 ) ) ;
#12025 = ORIENTED_EDGE ( 'NONE', *, *, #17073, .F. ) ;
#12026 = CARTESIAN_POINT ( 'NONE',  ( 0.2189426737742418139, -1.305592238685004736, -0.4125659523519144001 ) ) ;
#12027 = CARTESIAN_POINT ( 'NONE',  ( -0.03647137243075283808, -0.2291011402249958639, 0.4576748478490594296 ) ) ;
#12028 = CIRCLE ( 'NONE', #31733, 0.09249999999977555343 ) ;
#12029 = CARTESIAN_POINT ( 'NONE',  ( 0.08829612734217157088, -0.8123682747727402065, 0.2531801848959081558 ) ) ;
#12030 = ORIENTED_EDGE ( 'NONE', *, *, #40432, .T. ) ;
#12031 = CARTESIAN_POINT ( 'NONE',  ( -0.01896968469605126578, -0.07379952543979935442, -0.5147668824877623672 ) ) ;
#12032 = CARTESIAN_POINT ( 'NONE',  ( 0.04854223356900850411, -0.9826572199518598394, 0.6756526958422652829 ) ) ;
#12034 = ORIENTED_EDGE ( 'NONE', *, *, #36368, .T. ) ;
#12033 = ORIENTED_EDGE ( 'NONE', *, *, #12551, .F. ) ;
#12035 = CARTESIAN_POINT ( 'NONE',  ( -0.1127636766158878062, -0.5184084763139832353, 0.1453728055589162682 ) ) ;
#12036 = AXIS2_PLACEMENT_3D ( 'NONE', #9649, #13336, #13127 ) ;
#12037 = CIRCLE ( 'NONE', #25193, 0.2526340763130724976 ) ;
#12038 = CARTESIAN_POINT ( 'NONE',  ( 0.04230170315644469353, -0.008603754326271256456, 0.4686066795590708711 ) ) ;
#12039 = CARTESIAN_POINT ( 'NONE',  ( 0.01896931156525832537, -0.4667677622193532327, -0.2292597581959257558 ) ) ;
#12040 = CARTESIAN_POINT ( 'NONE',  ( 0.2327253210492125635, -1.594686327790063363, -0.3238482666460236192 ) ) ;
#12041 = FACE_OUTER_BOUND ( 'NONE', #25108, .T. ) ;
#12042 = EDGE_CURVE ( 'NONE', #8991, #10935, #5431, .T. ) ;
#12044 = CARTESIAN_POINT ( 'NONE',  ( 0.1637585665034339832, -0.5994899851647166322, 0.1022936816274461203 ) ) ;
#12043 = CARTESIAN_POINT ( 'NONE',  ( 0.05186792262756725197, 0.4530091620765404059, 0.1282979832840893120 ) ) ;
#12045 = CARTESIAN_POINT ( 'NONE',  ( 5.463695987328526437E-16, -0.2899999999999993694, -7.171100983368691195E-16 ) ) ;
#12046 = ORIENTED_EDGE ( 'NONE', *, *, #39296, .T. ) ;
#12047 = ADVANCED_FACE ( 'NONE', ( #28308 ), #16189, .T. ) ;
#12048 = CARTESIAN_POINT ( 'NONE',  ( 0.2271594253415122056, -0.8546831118382453019, 0.7084329392384713930 ) ) ;
#12049 = ORIENTED_EDGE ( 'NONE', *, *, #18204, .F. ) ;
#12050 = CARTESIAN_POINT ( 'NONE',  ( 0.7053410326410682885, -1.513865973459305625, 0.5669051209305092653 ) ) ;
#12051 = CARTESIAN_POINT ( 'NONE',  ( 0.06043370286545070302, -0.5384506411558260819, 0.1457185332388693799 ) ) ;
#12053 = CARTESIAN_POINT ( 'NONE',  ( 0.5670943157340239127, -1.614800677630997772, 0.4626854145028929111 ) ) ;
#12052 = CARTESIAN_POINT ( 'NONE',  ( 0.07444041171459701844, -1.335750591677182575, 0.5458585244681498638 ) ) ;
#12054 = DIRECTION ( 'NONE',  ( -0.000000000000000000, 0.3090169943749569437, 0.9510565162951504226 ) ) ;
#12055 = CARTESIAN_POINT ( 'NONE',  ( 0.1960722456818422554, -1.288731303253011440, -0.2917126172454974076 ) ) ;
#12056 = EDGE_LOOP ( 'NONE', ( #23812, #91, #9763, #3991 ) ) ;
#12057 = PRODUCT_DEFINITION_CONTEXT ( 'detailed design', #36329, 'design' ) ;
#12058 = CARTESIAN_POINT ( 'NONE',  ( 0.4999668580349169722, -1.586321472701693214, -0.5587740707772209658 ) ) ;
#12059 = CARTESIAN_POINT ( 'NONE',  ( 0.3965441076082558691, -2.011587606276659557, -0.2840872118775558675 ) ) ;
#12060 = CARTESIAN_POINT ( 'NONE',  ( 0.1268547004962813363, -0.5950674506041877532, 0.3072773567659817240 ) ) ;
#12061 = CARTESIAN_POINT ( 'NONE',  ( 0.4828783412368256589, -1.662196317011951807, 0.4845646038109067133 ) ) ;
#12062 = CARTESIAN_POINT ( 'NONE',  ( 0.3069771088456038077, -1.146818725534535233, 0.5182417262812423209 ) ) ;
#12063 = VERTEX_POINT ( 'NONE', #10210 ) ;
#12064 = CARTESIAN_POINT ( 'NONE',  ( -0.07999999999999998779, -1.706654027108509997, -0.06438491259384498955 ) ) ;
#12065 = CARTESIAN_POINT ( 'NONE',  ( 0.2347586836304188518, -1.231494575820371917, 0.5212298410651946545 ) ) ;
#12066 = CIRCLE ( 'NONE', #34404, 0.01500000000000004281 ) ;
#12067 = DIRECTION ( 'NONE',  ( 0.8660254037844387076, 5.423418723394460541E-31, 0.5000000000000001110 ) ) ;
#12068 = CARTESIAN_POINT ( 'NONE',  ( 0.2347703329119436577, -1.231486961704138405, 0.5219302041182221075 ) ) ;
#12069 = CARTESIAN_POINT ( 'NONE',  ( 0.6802496923668470696, -1.403733334520502973, 0.6188728273484885856 ) ) ;
#12070 = AXIS2_PLACEMENT_3D ( 'NONE', #6200, #32245, #18769 ) ;
#12071 = AXIS2_PLACEMENT_3D ( 'NONE', #17236, #11676, #30395 ) ;
#12072 = CARTESIAN_POINT ( 'NONE',  ( -0.04230258372739956890, 0.2788587125276416057, 0.3766249785157091967 ) ) ;
#12073 = CARTESIAN_POINT ( 'NONE',  ( 0.01055723141996775354, -1.003148971495586350, 0.5413436042764798728 ) ) ;
#12074 = CARTESIAN_POINT ( 'NONE',  ( 0.6222686170074345213, -1.528537841564955757, -0.3994016981617310447 ) ) ;
#12075 = CARTESIAN_POINT ( 'NONE',  ( 0.1685455824392826929, -1.307862364081260775, -0.7280104148493009575 ) ) ;
#12076 = CARTESIAN_POINT ( 'NONE',  ( 0.5799012421785839644, -1.622272342335922879, 0.5669080035957854147 ) ) ;
#12077 = CARTESIAN_POINT ( 'NONE',  ( 0.1023754337098985029, 0.06118878220587092853, 0.07268054736755601153 ) ) ;
#12078 = AXIS2_PLACEMENT_3D ( 'NONE', #25636, #22357, #6487 ) ;
#12079 = CARTESIAN_POINT ( 'NONE',  ( 0.3699999999999786793, -2.143549940236731732, -0.4549916158381474007 ) ) ;
#12080 = CIRCLE ( 'NONE', #4196, 0.2500000000000000555 ) ;
#12081 = EDGE_LOOP ( 'NONE', ( #18203, #22132, #34395, #39538 ) ) ;
#12082 = CARTESIAN_POINT ( 'NONE',  ( 0.3634393234136681916, -1.759352117114970859, -0.5002830012641544810 ) ) ;
#12083 = CARTESIAN_POINT ( 'NONE',  ( 0.3828601130222601956, -1.724001686837443481, -0.5877931644812478540 ) ) ;
#12084 = CYLINDRICAL_SURFACE ( 'NONE', #27815, 0.1000000000000000194 ) ;
#12085 = CARTESIAN_POINT ( 'NONE',  ( 0.5264113014007612001, -1.640729993778266893, -0.5166151207188711680 ) ) ;
#12086 = VERTEX_POINT ( 'NONE', #37554 ) ;
#12087 = CARTESIAN_POINT ( 'NONE',  ( 0.3625003971738279263, -1.132488407015356247, 0.6206807596827853546 ) ) ;
#12088 = CARTESIAN_POINT ( 'NONE',  ( -3.757258772823647403E-22, 0.06117178301711218014, -0.1249999999999999029 ) ) ;
#12089 = CARTESIAN_POINT ( 'NONE',  ( 0.03643058821096709782, 0.2291047292463132268, -0.4577947064495169194 ) ) ;
#12090 = CIRCLE ( 'NONE', #23938, 0.01500000000000003067 ) ;
#12091 = CARTESIAN_POINT ( 'NONE',  ( 0.5234610746152311700, -1.331927276539631499, 0.6628694543310861276 ) ) ;
#12093 = CARTESIAN_POINT ( 'NONE',  ( 0.5189221204507463714, -1.603650243462305003, -0.6104946154672951097 ) ) ;
#12092 = CARTESIAN_POINT ( 'NONE',  ( -0.2746410161513779258, -1.804235510932644004, -0.1501860188971498311 ) ) ;
#12094 = CARTESIAN_POINT ( 'NONE',  ( 0.5108734140540642787, -1.113869616463002643, 0.5959577563698095215 ) ) ;
#12095 = EDGE_LOOP ( 'NONE', ( #549, #29315, #34050, #25648, #3750, #3747 ) ) ;
#12096 = CALENDAR_DATE ( 2026, 13, 10 ) ;
#12097 = CARTESIAN_POINT ( 'NONE',  ( 0.1909286924077255032, -1.257064795538239022, -0.3194753470178354759 ) ) ;
#12098 = ORIENTED_EDGE ( 'NONE', *, *, #13191, .T. ) ;
#12099 = CARTESIAN_POINT ( 'NONE',  ( -0.04230188431063500870, 0.2825024449121532055, -0.3739792551055095005 ) ) ;
#12100 = AXIS2_PLACEMENT_3D ( 'NONE', #34691, #3821, #6497 ) ;
#12101 = ORIENTED_EDGE ( 'NONE', *, *, #34374, .F. ) ;
#12102 = AXIS2_PLACEMENT_3D ( 'NONE', #19340, #31879, #32467 ) ;
#12103 = CARTESIAN_POINT ( 'NONE',  ( 0.03676551872540411575, -0.5603456902706456244, 0.2596414817900425942 ) ) ;
#12105 = CARTESIAN_POINT ( 'NONE',  ( 0.1122718071269267481, -0.8163803874974441266, -0.05810663026781571344 ) ) ;
#12104 = CARTESIAN_POINT ( 'NONE',  ( -2.112273405726188513E-14, -2.183180860297921466, -0.4937760292030871079 ) ) ;
#12106 = DIRECTION ( 'NONE',  ( 0.8660512985181134660, 0.4999551463232372317, 0.000000000000000000 ) ) ;
#12107 = ORIENTED_EDGE ( 'NONE', *, *, #8470, .T. ) ;
#12108 = VERTEX_POINT ( 'NONE', #22360 ) ;
#12109 = CARTESIAN_POINT ( 'NONE',  ( 0.3704445633776799474, -1.093428063567875475, 0.6364787831697373832 ) ) ;
#12110 = CARTESIAN_POINT ( 'NONE',  ( 0.2524445808839146377, -0.9543908899680845215, 0.7414919205053484008 ) ) ;
#12111 = VERTEX_POINT ( 'NONE', #31409 ) ;
#12112 = VECTOR ( 'NONE', #9358, 39.37007874015748143 ) ;
#12113 = CARTESIAN_POINT ( 'NONE',  ( -2.070754768975509030, -0.09959325338431655739, 0.09550516381870291505 ) ) ;
#12114 = DIRECTION ( 'NONE',  ( 1.000000000000000000, 0.000000000000000000, 0.000000000000000000 ) ) ;
#12115 = CIRCLE ( 'NONE', #4860, 0.1000000000000000194 ) ;
#12116 = CARTESIAN_POINT ( 'NONE',  ( -0.05464101615137773038, -1.599201040860868339, 0.1642182323853691728 ) ) ;
#12117 = FACE_OUTER_BOUND ( 'NONE', #31237, .T. ) ;
#12118 = DIRECTION ( 'NONE',  ( -0.000000000000000000, 0.5781348229923771731, -0.8159412518334715481 ) ) ;
#12119 = CARTESIAN_POINT ( 'NONE',  ( 0.008263909818985001182, -0.6872203660130532521, -0.01225013371141639093 ) ) ;
#12120 = CARTESIAN_POINT ( 'NONE',  ( 0.2398702836577433772, -1.946110816799010879, -0.6651903542983218509 ) ) ;
#12121 = CARTESIAN_POINT ( 'NONE',  ( 0.05889106705834949718, -1.326084810051836982, 0.5931655932887337501 ) ) ;
#12122 = DATE_TIME_ROLE ( 'creation_date' ) ;
#12123 = CIRCLE ( 'NONE', #14762, 0.08000000000000000167 ) ;
#12124 = CARTESIAN_POINT ( 'NONE',  ( 0.4673670683790682734, -1.135785369362879216, 0.4578920774821071960 ) ) ;
#12125 = CARTESIAN_POINT ( 'NONE',  ( 0.4957950520941065697, -1.219580963930161133, 0.6057417262809816627 ) ) ;
#12126 = DIRECTION ( 'NONE',  ( -0.000000000000000000, -0.7071067811865473507, -0.7071067811865475727 ) ) ;
#12127 = AXIS2_PLACEMENT_3D ( 'NONE', #39681, #4708, #29424 ) ;
#12128 = APPROVAL_PERSON_ORGANIZATION ( #29425, #40085, #23666 ) ;
#12129 = CARTESIAN_POINT ( 'NONE',  ( 0.009238630504655715933, -0.9704941665429688280, 0.5327612241319219510 ) ) ;
#12130 = CARTESIAN_POINT ( 'NONE',  ( 0.2717989554234621075, -1.672126109062499477, 0.4863275332560569875 ) ) ;
#12131 = CARTESIAN_POINT ( 'NONE',  ( 0.3122991364858720975, -1.758414243292331536, 0.5144673742672133399 ) ) ;
#12132 = CARTESIAN_POINT ( 'NONE',  ( 0.1977815345931705215, -1.253108778471563767, -0.3161890406021737876 ) ) ;
#12133 = VECTOR ( 'NONE', #6231, 39.37007874015748854 ) ;
#12134 = ORIENTED_EDGE ( 'NONE', *, *, #38921, .T. ) ;
#12135 = VERTEX_POINT ( 'NONE', #9379 ) ;
#12136 =( BOUNDED_SURFACE ( )  B_SPLINE_SURFACE ( 3, 2, ( 
 ( #1399, #16825, #23814 ),
 ( #33254, #23614, #7937 ),
 ( #13908, #30172, #22994 ),
 ( #26891, #26481, #4260 ),
 ( #7750, #17423, #8149 ),
 ( #23426, #20119, #20312 ),
 ( #29370, #35943, #32835 ),
 ( #4640, #27087, #17216 ),
 ( #7321, #13714, #5064 ),
 ( #29760, #17625, #39421 ),
 ( #1603, #26282, #35730 ),
 ( #14131, #26701, #20726 ),
 ( #39234, #2000, #10434 ),
 ( #7544, #29979, #11240 ),
 ( #36127, #11056, #20512 ),
 ( #33046, #10634, #36332 ),
 ( #35516, #38800, #19898 ),
 ( #32434, #1213, #23206 ) ),
 .UNSPECIFIED., .F., .F., .T. ) 
 B_SPLINE_SURFACE_WITH_KNOTS ( ( 4, 2, 2, 2, 2, 2, 2, 2, 4 ),
 ( 3, 3 ),
 ( -0.001532620576208883721, -0.0007637936630077779348, 5.033250193327851521E-06, 0.0007738601633944336379, 0.001542687076595539424, 0.002311513989796645102, 0.003080340902997751214, 0.003849167816198856892, 0.004617994729399962570 ),
 ( 0.000000000000000000, 1.000000000000000000 ),
 .UNSPECIFIED. ) 
 GEOMETRIC_REPRESENTATION_ITEM ( )  RATIONAL_B_SPLINE_SURFACE ( (
 ( 1.000000000000000000, 0.7283825911960434274, 1.000000000000000000),
 ( 1.000000000000000000, 0.7404385082112715510, 1.000000000000000000),
 ( 1.000000000000000000, 0.7521504257740206922, 1.000000000000000000),
 ( 1.000000000000000000, 0.7744497410759673128, 1.000000000000000000),
 ( 1.000000000000000000, 0.7845654757376588906, 1.000000000000000000),
 ( 1.000000000000000000, 0.8022083990889582461, 1.000000000000000000),
 ( 1.000000000000000000, 0.8094167424698768265, 1.000000000000000000),
 ( 1.000000000000000000, 0.8194491993617196712, 1.000000000000000000),
 ( 1.000000000000000000, 0.8220634900780805498, 1.000000000000000000),
 ( 1.000000000000000000, 0.8220705070823159932, 1.000000000000000000),
 ( 1.000000000000000000, 0.8194468812480130149, 1.000000000000000000),
 ( 1.000000000000000000, 0.8094220769840309027, 1.000000000000000000),
 ( 1.000000000000000000, 0.8022659121987061326, 1.000000000000000000),
 ( 1.000000000000000000, 0.7845681159033996988, 1.000000000000000000),
 ( 1.000000000000000000, 0.7744426415183223167, 1.000000000000000000),
 ( 1.000000000000000000, 0.7522890290930832613, 1.000000000000000000),
 ( 1.000000000000000000, 0.7403540167213815693, 1.000000000000000000),
 ( 1.000000000000000000, 0.7283825911960234434, 1.000000000000000000) ) ) 
 REPRESENTATION_ITEM ( '' )  SURFACE ( )  );
#12137 = CARTESIAN_POINT ( 'NONE',  ( -0.1157351208611892279, -0.4799584063719126159, 0.1184929141221668786 ) ) ;
#12138 = ORIENTED_EDGE ( 'NONE', *, *, #15426, .F. ) ;
#12139 = DIRECTION ( 'NONE',  ( -1.000000000000000000, -2.276539994720212446E-15, 0.000000000000000000 ) ) ;
#12140 = DIRECTION ( 'NONE',  ( 0.000000000000000000, 0.000000000000000000, -1.000000000000000000 ) ) ;
#12141 = CARTESIAN_POINT ( 'NONE',  ( -0.1133606652272212828, -0.5183057948313447572, 0.1157398326556578066 ) ) ;
#12143 = ORIENTED_EDGE ( 'NONE', *, *, #22555, .T. ) ;
#12142 = LINE ( 'NONE', #25094, #32436 ) ;
#12144 = ORIENTED_EDGE ( 'NONE', *, *, #38312, .F. ) ;
#12145 = CARTESIAN_POINT ( 'NONE',  ( 0.03158843595483479261, 0.4819971762524422609, -0.09920191295802893716 ) ) ;
#12146 = ORIENTED_EDGE ( 'NONE', *, *, #1321, .F. ) ;
#12147 = CARTESIAN_POINT ( 'NONE',  ( 0.04546828490520857941, -0.7968594640744619539, 0.6630748410649087710 ) ) ;
#12149 = CARTESIAN_POINT ( 'NONE',  ( 0.1164557078696717290, -1.290608969205410350, 0.5990493494779465244 ) ) ;
#12148 = CARTESIAN_POINT ( 'NONE',  ( 0.4887921365776452531, -1.679766821171225999, -0.4193976862638447711 ) ) ;
#12150 = APPLIED_DATE_AND_TIME_ASSIGNMENT ( #23953, #36684, ( #6983 ) ) ;
#12151 = LINE ( 'NONE', #14612, #34489 ) ;
#12152 = AXIS2_PLACEMENT_3D ( 'NONE', #660, #22650, #34964 ) ;
#12153 = DIRECTION ( 'NONE',  ( 1.188678714063520199E-15, -1.000000000000000000, 0.000000000000000000 ) ) ;
#12155 = ORIENTED_EDGE ( 'NONE', *, *, #24619, .T. ) ;
#12154 = ORIENTED_EDGE ( 'NONE', *, *, #29775, .T. ) ;
#12156 = CIRCLE ( 'NONE', #39080, 0.2000000000000000389 ) ;
#12157 = DIRECTION ( 'NONE',  ( 0.000000000000000000, 0.9510565162951525320, -0.3090169943749502268 ) ) ;
#12158 = CARTESIAN_POINT ( 'NONE',  ( 0.3768783096114196596, -1.720370743462857899, 0.4222122349756300963 ) ) ;
#12159 = CARTESIAN_POINT ( 'NONE',  ( -0.05491348488830374852, -0.4316112672892422064, 0.1667783590291052331 ) ) ;
#12160 = VECTOR ( 'NONE', #15314, 39.37007874015748143 ) ;
#12161 = CARTESIAN_POINT ( 'NONE',  ( 0.5010280360125842769, -1.301577949779766818, 0.8062107694647361322 ) ) ;
#12162 = DIRECTION ( 'NONE',  ( 0.4999551463232371762, -0.8660512985181134660, 0.000000000000000000 ) ) ;
#12163 = LOCAL_TIME ( 0, 53, 7.000000000000000000, #39088 ) ;
#12164 = CARTESIAN_POINT ( 'NONE',  ( 0.4915260346479126685, -1.695508583366576616, -0.4333519947141560857 ) ) ;
#12165 = CARTESIAN_POINT ( 'NONE',  ( -0.1102510911460810039, -0.5035121463812862741, 0.3528822442262277148 ) ) ;
#12166 = CIRCLE ( 'NONE', #7542, 0.08830708661417338567 ) ;
#12167 = CARTESIAN_POINT ( 'NONE',  ( 0.4554213719789483861, -1.084118224209758452, -0.4129387436622604657 ) ) ;
#12168 = CARTESIAN_POINT ( 'NONE',  ( 0.6588957223800396834, -1.564199738096486714, 0.5197417262808792238 ) ) ;
#12169 = EDGE_CURVE ( 'NONE', #24718, #12256, #7438, .T. ) ;
#12170 = CARTESIAN_POINT ( 'NONE',  ( 0.1784968570797965948, -1.218054820023663831, -0.5155029497116575543 ) ) ;
#12171 = DIRECTION ( 'NONE',  ( 5.551115123125718607E-17, 3.263080277421931478E-16, -1.000000000000000000 ) ) ;
#12172 = CARTESIAN_POINT ( 'NONE',  ( -0.1205998369024076505, -0.5041491367644056476, 0.3197686713205462050 ) ) ;
#12173 = CARTESIAN_POINT ( 'NONE',  ( -8.537024980200822558E-17, -0.6872203660140400183, 0.1290053960929137267 ) ) ;
#12174 = B_SPLINE_CURVE_WITH_KNOTS ( 'NONE', 1,
 ( #4371, #23712 ),
 .UNSPECIFIED., .F., .F.,
 ( 2, 2 ),
 ( 0.000000000000000000, 1.000000000000000000 ),
 .UNSPECIFIED. ) ;
#12175 = CARTESIAN_POINT ( 'NONE',  ( 0.06410545231634277863, -1.149572297890252059, 0.7543797106542713404 ) ) ;
#12176 = EDGE_CURVE ( 'NONE', #10240, #37075, #22314, .T. ) ;
#12177 = PERSON_AND_ORGANIZATION_ROLE ( 'design_supplier' ) ;
#12178 = CARTESIAN_POINT ( 'NONE',  ( 0.2320929863655918080, -0.6391054805530269611, 0.5101375161162777783 ) ) ;
#12179 = AXIS2_PLACEMENT_3D ( 'NONE', #39466, #11291, #19950 ) ;
#12180 = EDGE_CURVE ( 'NONE', #35064, #12063, #17957, .T. ) ;
#12181 = EDGE_CURVE ( 'NONE', #14515, #31373, #34408, .T. ) ;
#12182 = AXIS2_PLACEMENT_3D ( 'NONE', #1310, #26190, #38714 ) ;
#12183 = DIRECTION ( 'NONE',  ( 0.000000000000000000, -3.414809992080316105E-15, -1.000000000000000000 ) ) ;
#12184 = EDGE_CURVE ( 'NONE', #22691, #31970, #3523, .T. ) ;
#12185 = CARTESIAN_POINT ( 'NONE',  ( 0.04230170315644469353, 0.008603754326275107542, -0.4686066795590708711 ) ) ;
#12186 = DIRECTION ( 'NONE',  ( 1.000000000000000000, 2.280301054154495132E-31, -1.664003471950577689E-31 ) ) ;
#12187 = EDGE_LOOP ( 'NONE', ( #20661, #32531, #35678, #20599 ) ) ;
#12188 = DIRECTION ( 'NONE',  ( 0.000000000000000000, 0.000000000000000000, -1.000000000000000000 ) ) ;
#12189 = APPLIED_APPROVAL_ASSIGNMENT ( #33040, ( #36468 ) ) ;
#12190 = CARTESIAN_POINT ( 'NONE',  ( 0.2291492867289149638, -1.472603918266135903, 0.9192788838655852057 ) ) ;
#12191 = CARTESIAN_POINT ( 'NONE',  ( 0.1282480831355250206, -0.5607311205846683411, 0.2079606190596378357 ) ) ;
#12193 = ORIENTED_EDGE ( 'NONE', *, *, #32337, .T. ) ;
#12192 = CARTESIAN_POINT ( 'NONE',  ( -0.02000000000000000042, -2.241214508571226283, -0.3173949748123141568 ) ) ;
#12194 = VECTOR ( 'NONE', #14802, 39.37007874015748143 ) ;
#12195 = CARTESIAN_POINT ( 'NONE',  ( 0.5553494029534283838, -1.189621637772522389, 0.5881472999875582142 ) ) ;
#12197 = ORIENTED_EDGE ( 'NONE', *, *, #22498, .F. ) ;
#12196 = ORIENTED_EDGE ( 'NONE', *, *, #21805, .F. ) ;
#12198 = CARTESIAN_POINT ( 'NONE',  ( 0.6991393458465392508, -1.438784036003081246, 0.5823241596405769327 ) ) ;
#12199 = CARTESIAN_POINT ( 'NONE',  ( 0.3395539693250317348, -1.657457255472329027, -0.5807180344419580198 ) ) ;
#12200 = EDGE_CURVE ( 'NONE', #30753, #23563, #33727, .T. ) ;
#12201 = CARTESIAN_POINT ( 'NONE',  ( -0.2746410161513776482, -3.672249662662566472, -0.1880352225538197142 ) ) ;
#12202 = CALENDAR_DATE ( 2026, 13, 10 ) ;
#12203 = CARTESIAN_POINT ( 'NONE',  ( 0.3098980262120963891, -1.765718015157915710, 0.5682965708553142647 ) ) ;
#12204 = EDGE_LOOP ( 'NONE', ( #1927, #30422, #1808, #27668 ) ) ;
#12205 = CARTESIAN_POINT ( 'NONE',  ( 0.1402790378157611761, -0.7973165635238237403, 0.5029188386495354601 ) ) ;
#12206 = CARTESIAN_POINT ( 'NONE',  ( 0.3098600959331583304, -1.724931092596566851, 0.7848886570988899969 ) ) ;
#12207 = CARTESIAN_POINT ( 'NONE',  ( 0.1481794566618464815, -0.7263954259819791481, 0.5403200226437546716 ) ) ;
#12209 = LINE ( 'NONE', #14888, #32918 ) ;
#12208 = FACE_OUTER_BOUND ( 'NONE', #39181, .T. ) ;
#12210 = CARTESIAN_POINT ( 'NONE',  ( 0.02729138952952809422, -0.9928868837826979599, 0.4957075431573730318 ) ) ;
#12211 = ORIENTED_EDGE ( 'NONE', *, *, #14177, .T. ) ;
#12212 = PLANE ( 'NONE',  #14093 ) ;
#12213 = VECTOR ( 'NONE', #36926, 39.37007874015748143 ) ;
#12214 = CARTESIAN_POINT ( 'NONE',  ( 0.4297110609522239999, -1.008900777665432846, 0.7743681538882086768 ) ) ;
#12215 = AXIS2_PLACEMENT_3D ( 'NONE', #29325, #4413, #7890 ) ;
#12216 = CARTESIAN_POINT ( 'NONE',  ( -1.502516396515344672E-15, -0.3899999999999999578, 0.05000000000000055789 ) ) ;
#12217 = CARTESIAN_POINT ( 'NONE',  ( 0.3699999999999786793, -2.080230235891529667, -0.5026132101038165434 ) ) ;
#12218 = APPROVAL_PERSON_ORGANIZATION ( #3121, #19210, #19165 ) ;
#12219 = CARTESIAN_POINT ( 'NONE',  ( 0.03113248654051816583, -0.4578766358967566452, -0.4053162176620345170 ) ) ;
#12220 = PLANE ( 'NONE',  #1090 ) ;
#12221 = CARTESIAN_POINT ( 'NONE',  ( 0.04074269369199766400, -1.520498175474628511, -0.6410478022143386578 ) ) ;
#12222 = CIRCLE ( 'NONE', #8278, 0.04500000000000044242 ) ;
#12223 = DIRECTION ( 'NONE',  ( -1.000000000000000000, -7.857794173099924470E-32, -8.628166150854818811E-32 ) ) ;
#12224 = CARTESIAN_POINT ( 'NONE',  ( 0.4661750196922136991, -1.070732324447800421, 0.6917658376937553255 ) ) ;
#12225 = EDGE_CURVE ( 'NONE', #755, #26173, #37507, .T. ) ;
#12226 = CALENDAR_DATE ( 2026, 13, 10 ) ;
#12227 = CARTESIAN_POINT ( 'NONE',  ( 0.4722565137939111479, -1.077278095797315149, -0.4218496756560511374 ) ) ;
#12228 = EDGE_CURVE ( 'NONE', #18399, #31675, #22564, .T. ) ;
#12229 = CARTESIAN_POINT ( 'NONE',  ( 0.3810179107970706469, -1.714231790258144317, -0.4910716250263590377 ) ) ;
#12230 = CARTESIAN_POINT ( 'NONE',  ( 0.4026370839150509306, -1.708716391613837704, 0.4182417262808776903 ) ) ;
#12231 = ADVANCED_FACE ( 'NONE', ( #982, #3816, #28911 ), #13283, .F. ) ;
#12232 = CARTESIAN_POINT ( 'NONE',  ( -0.1163196563843193754, -0.5318992644065130282, 0.3135508459095576184 ) ) ;
#12233 = ORIENTED_EDGE ( 'NONE', *, *, #37908, .T. ) ;
#12234 = CARTESIAN_POINT ( 'NONE',  ( 0.4310167615618634707, -1.587237252056899584, -0.3866364743305638618 ) ) ;
#12235 = DIRECTION ( 'NONE',  ( 0.000000000000000000, -3.725247264087630335E-15, -1.000000000000000000 ) ) ;
#12236 = CARTESIAN_POINT ( 'NONE',  ( 0.08964054516919921223, -0.5683534925436617424, 0.1144277174209273190 ) ) ;
#12237 = ORIENTED_EDGE ( 'NONE', *, *, #17031, .T. ) ;
#12238 = CARTESIAN_POINT ( 'NONE',  ( -0.05252359774140243770, -0.009047791085682871728, -0.4689872004378276005 ) ) ;
#12239 = AXIS2_PLACEMENT_3D ( 'NONE', #36642, #36437, #33342 ) ;
#12240 = CARTESIAN_POINT ( 'NONE',  ( -0.01390182309215610978, -0.8546603537104834336, 0.2908326285636944619 ) ) ;
#12242 = ORIENTED_EDGE ( 'NONE', *, *, #15432, .F. ) ;
#12241 = ORIENTED_EDGE ( 'NONE', *, *, #39340, .F. ) ;
#12243 = CARTESIAN_POINT ( 'NONE',  ( 0.3061198483567182382, -1.759173221084211702, 0.5682343826784257423 ) ) ;
#12244 = FACE_OUTER_BOUND ( 'NONE', #6589, .T. ) ;
#12245 = ADVANCED_FACE ( 'NONE', ( #17179 ), #7287, .T. ) ;
#12246 = LOCAL_TIME ( 0, 53, 7.000000000000000000, #30301 ) ;
#12247 = CARTESIAN_POINT ( 'NONE',  ( 0.7394099696849650849, -1.503374687208528737, 0.6698237402283935271 ) ) ;
#12248 = CARTESIAN_POINT ( 'NONE',  ( 0.3573642944564824342, -1.883588035281504647, -0.5128792341014730694 ) ) ;
#12249 = CARTESIAN_POINT ( 'NONE',  ( 0.3885612764051886714, -1.758570040784675159, -0.5425266244860569298 ) ) ;
#12251 = DIRECTION ( 'NONE',  ( 1.000000000000000000, 6.779273404243070203E-32, 4.314083075427408311E-32 ) ) ;
#12250 = CARTESIAN_POINT ( 'NONE',  ( 0.05137569054208863950, 0.4554428576827989628, 0.1244487204292523824 ) ) ;
#12252 = DIRECTION ( 'NONE',  ( -1.000000000000000000, 0.000000000000000000, -1.138269997360105631E-15 ) ) ;
#12253 = EDGE_LOOP ( 'NONE', ( #9555, #20640, #28872, #25322 ) ) ;
#12254 = AXIS2_PLACEMENT_3D ( 'NONE', #39792, #5024, #32603 ) ;
#12255 = CARTESIAN_POINT ( 'NONE',  ( 0.1256500344729209739, -0.6634235672001109752, 0.4782051305092041571 ) ) ;
#12256 = VERTEX_POINT ( 'NONE', #30140 ) ;
#12257 = PERSON ( 'NAUO-PER16', 'UNSPECIFIED', 'UNSPECIFIED', ('UNSPECIFIED'), ('UNSPECIFIED'), ('UNSPECIFIED') ) ;
#12258 = DIRECTION ( 'NONE',  ( 0.000000000000000000, 0.000000000000000000, 1.000000000000000000 ) ) ;
#12259 = CARTESIAN_POINT ( 'NONE',  ( 0.1060801343968929555, -0.7029796262605895185, 0.5196367930449407035 ) ) ;
#12261 = CARTESIAN_POINT ( 'NONE',  ( 0.5546727557022121946, -1.622188815229450576, 0.4987667657539088251 ) ) ;
#12260 = CARTESIAN_POINT ( 'NONE',  ( -0.02000000000000000042, -2.177105168660885326, -0.2518349584362399862 ) ) ;
#12262 = CARTESIAN_POINT ( 'NONE',  ( 0.5022839945508311699, -1.192782407697791980, 0.4224083929475445642 ) ) ;
#12263 = CARTESIAN_POINT ( 'NONE',  ( -0.2343922129835739054, -0.5166151207188712791, 0.3599999999999997646 ) ) ;
#12264 = CARTESIAN_POINT ( 'NONE',  ( -0.1743922129835733803, -0.5166151207188712791, 0.3749999999999999445 ) ) ;
#12265 = CARTESIAN_POINT ( 'NONE',  ( 0.3999999999999789280, -2.087081592863325952, -0.4706838381558562379 ) ) ;
#12266 = CARTESIAN_POINT ( 'NONE',  ( 0.1536443843255308750, -0.6766421297890219400, 0.4621652830613652840 ) ) ;
#12267 = EDGE_CURVE ( 'NONE', #6859, #2486, #5605, .T. ) ;
#12268 = CARTESIAN_POINT ( 'NONE',  ( 0.4843194246718440232, -1.673553810144886578, 0.5158839267268513495 ) ) ;
#12269 = DIRECTION ( 'NONE',  ( 0.000000000000000000, 0.000000000000000000, -1.000000000000000000 ) ) ;
#12270 = ORIENTED_EDGE ( 'NONE', *, *, #1477, .T. ) ;
#12271 = CARTESIAN_POINT ( 'NONE',  ( -0.01548846960712763066, 0.4730347584885825629, 0.2341461249029053171 ) ) ;
#12272 = CARTESIAN_POINT ( 'NONE',  ( 0.5860257985473268372, -1.592810714289452312, 0.4182417262808775793 ) ) ;
#12273 = DIRECTION ( 'NONE',  ( -1.000000000000000000, 0.000000000000000000, 0.000000000000000000 ) ) ;
#12274 = CARTESIAN_POINT ( 'NONE',  ( 0.2034338387653989444, -1.249618221326741496, 0.4422361201100588057 ) ) ;
#12275 = CIRCLE ( 'NONE', #35260, 0.08000000000000000167 ) ;
#12276 = CARTESIAN_POINT ( 'NONE',  ( 0.2320929863655918080, -0.6391054805530269611, 0.5101375161162777783 ) ) ;
#12277 = CARTESIAN_POINT ( 'NONE',  ( -0.04574984450155029914, 0.2311445325521691019, 0.4288136795716618876 ) ) ;
#12278 = LOCAL_TIME ( 0, 53, 7.000000000000000000, #7827 ) ;
#12279 = ADVANCED_FACE ( 'NONE', ( #35482 ), #1182, .T. ) ;
#12280 = CARTESIAN_POINT ( 'NONE',  ( 0.6560555959785092650, -1.525593284718363973, -0.4139158794185884838 ) ) ;
#12281 = CARTESIAN_POINT ( 'NONE',  ( 0.03724056042341840345, -1.737240332959331779, -0.6683582582716187659 ) ) ;
#12282 = CARTESIAN_POINT ( 'NONE',  ( -0.02000000000000000042, -1.750394882718339762, -0.1142373872069606250 ) ) ;
#12283 = CARTESIAN_POINT ( 'NONE',  ( 0.3792246514435647642, -1.152363445361852756, 0.4250283846459516623 ) ) ;
#12284 = AXIS2_PLACEMENT_3D ( 'NONE', #38796, #36327, #11236 ) ;
#12285 = CARTESIAN_POINT ( 'NONE',  ( 0.1909286924077255587, -1.257064795538239022, -0.3404777180881179421 ) ) ;
#12286 = ORIENTED_EDGE ( 'NONE', *, *, #33445, .F. ) ;
#12287 = ADVANCED_FACE ( 'NONE', ( #20082 ), #11883, .T. ) ;
#12288 = DIRECTION ( 'NONE',  ( 0.000000000000000000, 0.000000000000000000, -1.000000000000000000 ) ) ;
#12289 = CARTESIAN_POINT ( 'NONE',  ( 0.3825425089729009298, -1.696932111950381294, -0.6182103527988705993 ) ) ;
#12290 = CARTESIAN_POINT ( 'NONE',  ( 0.6609374024770126033, -1.531375946314106562, 0.4235895360073886895 ) ) ;
#12291 = CARTESIAN_POINT ( 'NONE',  ( 0.3775892182204781400, -1.738445149920042843, 0.6053742338740327744 ) ) ;
#12292 = ORIENTED_EDGE ( 'NONE', *, *, #36822, .F. ) ;
#12293 = CARTESIAN_POINT ( 'NONE',  ( 0.5471103864378531467, -1.663420781200640519, -0.5477774273223376955 ) ) ;
#12294 = CARTESIAN_POINT ( 'NONE',  ( 0.3305685589621363274, -1.177413511476334218, 0.5677266399387778106 ) ) ;
#12295 = CARTESIAN_POINT ( 'NONE',  ( 0.3356575430205383515, -1.760770474539644415, 0.4707318425698279740 ) ) ;
#12296 = EDGE_CURVE ( 'NONE', #35002, #4809, #27199, .T. ) ;
#12297 = CARTESIAN_POINT ( 'NONE',  ( 0.4789118146089810790, -1.259265696533273360, 0.6923424817665398967 ) ) ;
#12298 = APPLIED_DATE_AND_TIME_ASSIGNMENT ( #11552, #30466, ( #11608 ) ) ;
#12300 = CARTESIAN_POINT ( 'NONE',  ( 0.4382015218937659884, -1.612541052972227940, -0.6615483979663951963 ) ) ;
#12299 = CARTESIAN_POINT ( 'NONE',  ( -0.1710642717957994163, 0.4986889573705637346, 0.1482573527501111488 ) ) ;
#12301 = CARTESIAN_POINT ( 'NONE',  ( 0.4373890596466497582, -1.046786911024660593, 0.6537231983888873721 ) ) ;
#12302 = VECTOR ( 'NONE', #37461, 39.37007874015748854 ) ;
#12303 = ORIENTED_EDGE ( 'NONE', *, *, #6586, .T. ) ;
#12304 = EDGE_CURVE ( 'NONE', #17350, #11030, #18363, .T. ) ;
#12305 = DATE_AND_TIME ( #21977, #32559 ) ;
#12306 = CARTESIAN_POINT ( 'NONE',  ( 0.1025208718600092855, -1.387521180747156135, 0.6451533902090165196 ) ) ;
#12307 = EDGE_LOOP ( 'NONE', ( #11834, #18249 ) ) ;
#12308 = VERTEX_POINT ( 'NONE', #36710 ) ;
#12309 = EDGE_CURVE ( 'NONE', #4879, #24171, #35555, .T. ) ;
#12310 = CARTESIAN_POINT ( 'NONE',  ( 0.3226986062199907468, -1.438512784532514743, 0.8769455027070669484 ) ) ;
#12312 = CARTESIAN_POINT ( 'NONE',  ( 0.1850717614292713420, -0.8146629789669863619, 0.03779116257895110548 ) ) ;
#12311 = DIRECTION ( 'NONE',  ( 1.000000000000000000, 2.341930812374887555E-31, -1.664003471950578127E-31 ) ) ;
#12313 = DIRECTION ( 'NONE',  ( 0.000000000000000000, -0.4393346272636262095, -0.8983234858819681978 ) ) ;
#12314 = VERTEX_POINT ( 'NONE', #8932 ) ;
#12315 = ORIENTED_EDGE ( 'NONE', *, *, #30679, .T. ) ;
#12316 = ORIENTED_EDGE ( 'NONE', *, *, #1417, .T. ) ;
#12317 = CARTESIAN_POINT ( 'NONE',  ( 0.4278511620221643330, -1.036794873576569742, 0.6363761450469351821 ) ) ;
#12318 = CARTESIAN_POINT ( 'NONE',  ( 0.5529345759058228449, -1.511181546743121329, 0.5724623201282376117 ) ) ;
#12319 = VERTEX_POINT ( 'NONE', #24793 ) ;
#12320 = CARTESIAN_POINT ( 'NONE',  ( 0.2670249539660715654, -1.533299212170818215, -0.3445188814933614063 ) ) ;
#12321 = CARTESIAN_POINT ( 'NONE',  ( -0.2600000000000002309, 0.5182417262804744906, 0.3749999999999995559 ) ) ;
#12322 = CARTESIAN_POINT ( 'NONE',  ( 0.5997830302434702388, -1.482755616589708447, -0.4037571860997516415 ) ) ;
#12323 = FACE_OUTER_BOUND ( 'NONE', #8838, .T. ) ;
#12324 = CARTESIAN_POINT ( 'NONE',  ( 0.1399999999999994582, 4.857225732735056783E-17, 0.1250000000000000000 ) ) ;
#12325 = FACE_OUTER_BOUND ( 'NONE', #28885, .T. ) ;
#12326 = CARTESIAN_POINT ( 'NONE',  ( 0.4250974642402614578, -1.123820390179259832, 0.5291520644862812706 ) ) ;
#12327 = CARTESIAN_POINT ( 'NONE',  ( 0.07208523036626358904, -1.310649742666034401, 0.6665797303350883274 ) ) ;
#12328 = SECURITY_CLASSIFICATION_LEVEL ( 'unclassified' ) ;
#12329 = EDGE_CURVE ( 'NONE', #39928, #25455, #21950, .T. ) ;
#12330 = CARTESIAN_POINT ( 'NONE',  ( 0.4912263342062789806, -1.081771733098906729, 0.5857582446664630904 ) ) ;
#12331 = CARTESIAN_POINT ( 'NONE',  ( 0.4630246609694094739, -1.116058605367935774, 0.5664886635214763100 ) ) ;
#12332 = CARTESIAN_POINT ( 'NONE',  ( 0.4480287403985907524, -1.224062292566040044, 0.5856983068965044836 ) ) ;
#12333 = DIRECTION ( 'NONE',  ( 1.000000000000000000, -2.410886674703095109E-13, 1.702189702233165782E-12 ) ) ;
#12334 = CARTESIAN_POINT ( 'NONE',  ( -0.001163483333746527255, -0.8281092574587937127, 0.3345003353200291518 ) ) ;
#12335 = CARTESIAN_POINT ( 'NONE',  ( 0.3314668577237731006, -1.779294220870033971, 0.5182417262812423209 ) ) ;
#12336 = CARTESIAN_POINT ( 'NONE',  ( 0.1727937833756465480, -1.757125623733488018, -0.6809623346501596508 ) ) ;
#12337 = CARTESIAN_POINT ( 'NONE',  ( 0.1810766014996238460, -1.262752222553217729, -0.2917159793182513838 ) ) ;
#12338 = VERTEX_POINT ( 'NONE', #24371 ) ;
#12339 = ORIENTED_EDGE ( 'NONE', *, *, #21313, .T. ) ;
#12340 = CARTESIAN_POINT ( 'NONE',  ( -0.1204846181304661118, -0.5035940506942929717, 0.1366987775887355816 ) ) ;
#12341 = ORIENTED_EDGE ( 'NONE', *, *, #26320, .F. ) ;
#12342 = CARTESIAN_POINT ( 'NONE',  ( -0.01548846960721204577, 0.07651041855109251555, 0.5222379212565261275 ) ) ;
#12343 = DIRECTION ( 'NONE',  ( 0.000000000000000000, 0.000000000000000000, -1.000000000000000000 ) ) ;
#12344 = CARTESIAN_POINT ( 'NONE',  ( -0.2746410161513776482, -3.811657270145150989, -0.1642545796697100491 ) ) ;
#12346 = ORIENTED_EDGE ( 'NONE', *, *, #27835, .F. ) ;
#12345 = CARTESIAN_POINT ( 'NONE',  ( 0.6048371382129751339, -1.480131487591726192, 0.5922871325631168249 ) ) ;
#12347 = EDGE_LOOP ( 'NONE', ( #39647, #8688, #21988 ) ) ;
#12348 = DIRECTION ( 'NONE',  ( 0.000000000000000000, 0.000000000000000000, 1.000000000000000000 ) ) ;
#12349 = ORIENTED_EDGE ( 'NONE', *, *, #5238, .T. ) ;
#12350 = CARTESIAN_POINT ( 'NONE',  ( 0.2323486294662862328, -1.426838467342053773, 0.9230749924135009943 ) ) ;
#12352 = CARTESIAN_POINT ( 'NONE',  ( 0.08147730132796977831, -1.319048655531604330, 0.5775129287537744682 ) ) ;
#12351 = CARTESIAN_POINT ( 'NONE',  ( 0.3896040541115246003, -1.173367793883531629, 0.7095735600779148333 ) ) ;
#12353 = DIRECTION ( 'NONE',  ( 1.000000000000000000, 0.000000000000000000, 0.000000000000000000 ) ) ;
#12354 = PERSON_AND_ORGANIZATION_ROLE ( 'classification_officer' ) ;
#12355 = EDGE_CURVE ( 'NONE', #36780, #15637, #8520, .T. ) ;
#12356 = CARTESIAN_POINT ( 'NONE',  ( 0.4000099798367661164, -1.704638381955401183, 0.4182417262808776903 ) ) ;
#12358 = ORIENTED_EDGE ( 'NONE', *, *, #28398, .F. ) ;
#12357 = EDGE_LOOP ( 'NONE', ( #39591, #35936, #28263, #6055 ) ) ;
#12359 = CARTESIAN_POINT ( 'NONE',  ( 0.4645951959325665404, -1.068949338851189257, -0.4209103011858858490 ) ) ;
#12360 = CARTESIAN_POINT ( 'NONE',  ( 0.3886765788477002381, -1.754881642227921645, -0.4506904437265726870 ) ) ;
#12361 = CARTESIAN_POINT ( 'NONE',  ( -0.05269191099235791265, -0.4442874273374651239, 0.1490603884548177271 ) ) ;
#12362 = CARTESIAN_POINT ( 'NONE',  ( 0.1885535751052127285, -0.8341734923249479738, 0.6205604111359355191 ) ) ;
#12363 = FACE_OUTER_BOUND ( 'NONE', #31548, .T. ) ;
#12364 = DIRECTION ( 'NONE',  ( 1.000000000000000000, 9.106159978880829274E-15, 1.138269997360103659E-15 ) ) ;
#12365 = CARTESIAN_POINT ( 'NONE',  ( 0.01223674427371603327, -0.4317327575158859121, 0.1899612123909241723 ) ) ;
#12366 = CARTESIAN_POINT ( 'NONE',  ( 0.4228356896103982465, -1.238666721341417754, 0.5481991966187728105 ) ) ;
#12367 = CARTESIAN_POINT ( 'NONE',  ( 0.7471901070607220863, -1.513130089782565468, 0.5197417262808792238 ) ) ;
#12368 = CARTESIAN_POINT ( 'NONE',  ( 0.3619468766189660736, -1.093412635382523090, 0.7620081947267545175 ) ) ;
#12369 = DIRECTION ( 'NONE',  ( 0.000000000000000000, 0.000000000000000000, -1.000000000000000000 ) ) ;
#12370 = CARTESIAN_POINT ( 'NONE',  ( -0.2349999999999999867, -2.183180860297908144, -0.4937760292030871079 ) ) ;
#12371 = CYLINDRICAL_SURFACE ( 'NONE', #21345, 0.1000000000000000194 ) ;
#12372 = CARTESIAN_POINT ( 'NONE',  ( 0.3053298862878815467, -1.679825167650452089, 0.8905181393053133165 ) ) ;
#12373 = CARTESIAN_POINT ( 'NONE',  ( 0.07334890854203197919, -1.206402556078998822, 0.7552868396345799873 ) ) ;
#12374 = DATE_AND_TIME ( #8467, #13481 ) ;
#12375 = CARTESIAN_POINT ( 'NONE',  ( 0.3938123320717736853, -0.9371650893754340794, 0.7866333354397343491 ) ) ;
#12376 = B_SPLINE_CURVE_WITH_KNOTS ( 'NONE', 3,
 ( #5935, #18500, #3084, #6353, #37620, #18925, #22023, #21804, #34545, #12530, #2275, #2871, #39904, #34334, #40300, #31053 ),
 .UNSPECIFIED., .F., .F.,
 ( 4, 2, 2, 2, 2, 2, 2, 4 ),
 ( 0.002977951493358393584, 0.003350111319365625326, 0.003722271145372857068, 0.004094430971380088810, 0.004466590797387320552, 0.004838750623394552294, 0.005210910449401784036, 0.005955230101416240582 ),
 .UNSPECIFIED. ) ;
#12377 = DIRECTION ( 'NONE',  ( 0.000000000000000000, 0.000000000000000000, 1.000000000000000000 ) ) ;
#12378 = DIRECTION ( 'NONE',  ( 0.4999551463232372317, -0.8660512985181135770, 0.000000000000000000 ) ) ;
#12379 = CARTESIAN_POINT ( 'NONE',  ( 0.05283710938261042267, -0.3063690517300490246, 0.3541964274677651403 ) ) ;
#12380 = CARTESIAN_POINT ( 'NONE',  ( -0.2746410161513770931, -3.335205990917129881, -0.4042613180508733972 ) ) ;
#12381 = ORIENTED_EDGE ( 'NONE', *, *, #33838, .F. ) ;
#12382 = DIRECTION ( 'NONE',  ( -1.000000000000000000, -0.000000000000000000, -0.000000000000000000 ) ) ;
#12383 = CARTESIAN_POINT ( 'NONE',  ( 0.2364914840723867095, -1.527680518818696376, 0.9000837182161988137 ) ) ;
#12384 = CARTESIAN_POINT ( 'NONE',  ( 0.5753449303846843721, -1.469417681867138725, 0.7012099257484931680 ) ) ;
#12386 = EDGE_LOOP ( 'NONE', ( #16820, #22233, #20510, #15120 ) ) ;
#12385 = CARTESIAN_POINT ( 'NONE',  ( -0.1443375672974067936, 0.08000000000000023759, 0.000000000000000000 ) ) ;
#12387 = CARTESIAN_POINT ( 'NONE',  ( 0.2195574306699510647, -0.7404155031343288007, 0.4240249586596535059 ) ) ;
#12389 = ORIENTED_EDGE ( 'NONE', *, *, #16792, .T. ) ;
#12388 = ORIENTED_EDGE ( 'NONE', *, *, #10524, .F. ) ;
#12390 = CARTESIAN_POINT ( 'NONE',  ( 0.1736278472308480370, -1.267052248471710829, -0.7067244366091492980 ) ) ;
#12391 = CARTESIAN_POINT ( 'NONE',  ( 0.3646755385473242073, -1.685449887736102603, -0.5938584186312408919 ) ) ;
#12392 = DIRECTION ( 'NONE',  ( 0.000000000000000000, -0.5781348229923760629, 0.8159412518334723252 ) ) ;
#12393 = CARTESIAN_POINT ( 'NONE',  ( 0.3187641638634980401, -1.760284878867077962, 0.5597302103697523457 ) ) ;
#12394 = EDGE_LOOP ( 'NONE', ( #7678, #7114, #14666, #4132 ) ) ;
#12395 = EDGE_CURVE ( 'NONE', #5011, #2842, #2764, .T. ) ;
#12396 = EDGE_CURVE ( 'NONE', #1288, #26954, #19304, .T. ) ;
#12397 = CARTESIAN_POINT ( 'NONE',  ( 0.1440972951654591883, -0.8326116813828831065, 0.5086132051937420906 ) ) ;
#12398 = EDGE_CURVE ( 'NONE', #20386, #16145, #23918, .T. ) ;
#12399 = DIRECTION ( 'NONE',  ( -2.563099466555623676E-12, 0.5877852522924655876, -0.8090169943749527803 ) ) ;
#12400 = CARTESIAN_POINT ( 'NONE',  ( 0.4416766012272996811, -1.379493900532093198, 0.8297147258887590526 ) ) ;
#12402 = DIRECTION ( 'NONE',  ( 1.188678714063518227E-15, -1.000000000000000000, -3.263080277421930985E-16 ) ) ;
#12401 = CARTESIAN_POINT ( 'NONE',  ( -2.567390744445674500E-16, -0.05999999999999978961, -0.1849999999999994982 ) ) ;
#12403 = CARTESIAN_POINT ( 'NONE',  ( -0.1552002433785900914, 0.4812687096812806598, 0.09697487758648998257 ) ) ;
#12404 = ORIENTED_EDGE ( 'NONE', *, *, #14224, .F. ) ;
#12405 = ADVANCED_FACE ( 'NONE', ( #2563 ), #28721, .T. ) ;
#12406 = CARTESIAN_POINT ( 'NONE',  ( 0.4192448355688633832, -1.702263579849587760, 0.6182028396105488932 ) ) ;
#12407 = CARTESIAN_POINT ( 'NONE',  ( 0.6672510479475136647, -1.560290543660546092, 0.6093665759723777553 ) ) ;
#12408 = EDGE_CURVE ( 'NONE', #2424, #4246, #16397, .T. ) ;
#12409 = CARTESIAN_POINT ( 'NONE',  ( 0.1186103394390872201, -1.414144848331978510, 0.5683298932114988489 ) ) ;
#12410 = FACE_OUTER_BOUND ( 'NONE', #28802, .T. ) ;
#12411 =( CONVERSION_BASED_UNIT ( 'INCH', #21072 ) LENGTH_UNIT ( ) NAMED_UNIT ( #19419 ) );
#12412 = CARTESIAN_POINT ( 'NONE',  ( -0.1167294259372886750, -0.5331983348239501819, 0.3032895567580813356 ) ) ;
#12413 = DIRECTION ( 'NONE',  ( 1.000000000000000000, 0.000000000000000000, 0.000000000000000000 ) ) ;
#12414 = CARTESIAN_POINT ( 'NONE',  ( 0.003421962176364201202, -0.9701471101739370662, 0.4009549150280219965 ) ) ;
#12415 = CARTESIAN_POINT ( 'NONE',  ( 0.5484966004669556972, -1.177603726185705080, 0.6257892858931851654 ) ) ;
#12416 = DATE_AND_TIME ( #31151, #33866 ) ;
#12417 = CARTESIAN_POINT ( 'NONE',  ( 0.5919221460426853376, -1.604281172822828783, 0.6022512693985722088 ) ) ;
#12418 = ADVANCED_FACE ( 'NONE', ( #38531 ), #16936, .F. ) ;
#12419 = APPLIED_DATE_AND_TIME_ASSIGNMENT ( #15810, #34323, ( #1177 ) ) ;
#12420 = CARTESIAN_POINT ( 'NONE',  ( 0.3967672410070270383, -1.715978560527550378, 0.4221337113864314095 ) ) ;
#12421 = CARTESIAN_POINT ( 'NONE',  ( -0.04211471441534238996, -0.008601378579327368865, 0.4689528935642813812 ) ) ;
#12422 = ORIENTED_EDGE ( 'NONE', *, *, #31269, .T. ) ;
#12423 = CARTESIAN_POINT ( 'NONE',  ( 0.4341915061220629757, -1.587206619470876268, 0.5182417262812423209 ) ) ;
#12424 = DIRECTION ( 'NONE',  ( 0.000000000000000000, 0.000000000000000000, -1.000000000000000000 ) ) ;
#12425 = CARTESIAN_POINT ( 'NONE',  ( 0.1442713433645926024, -0.8486712127012279172, 0.5110818735405668889 ) ) ;
#12426 = ORIENTED_EDGE ( 'NONE', *, *, #15258, .F. ) ;
#12427 = CARTESIAN_POINT ( 'NONE',  ( -0.03674260963082680992, -0.04074834683009077863, -0.4790483961530569990 ) ) ;
#12428 = CARTESIAN_POINT ( 'NONE',  ( -0.01502126383153270378, -0.8492948373293983666, 0.1816685507761301444 ) ) ;
#12430 = ORIENTED_EDGE ( 'NONE', *, *, #14188, .F. ) ;
#12429 = EDGE_LOOP ( 'NONE', ( #39762, #10026, #28730, #30448 ) ) ;
#12431 = CARTESIAN_POINT ( 'NONE',  ( 0.01548846960707511190, -0.3772621329472763962, -0.3651003739303386730 ) ) ;
#12432 = CARTESIAN_POINT ( 'NONE',  ( 0.03113248654051816583, -0.3458405862425447119, -0.1052451372150005060 ) ) ;
#12433 = CARTESIAN_POINT ( 'NONE',  ( 0.2215211694921853935, -1.611350768318245974, -0.3261362320128111669 ) ) ;
#12434 = CARTESIAN_POINT ( 'NONE',  ( 0.3625960434667531151, -1.762758894398492204, -0.5926935080085831142 ) ) ;
#12436 = CARTESIAN_POINT ( 'NONE',  ( 0.1731685197160121870, -1.267101063757091861, 0.4261332338546713339 ) ) ;
#12435 = PLANE ( 'NONE',  #31197 ) ;
#12437 = CARTESIAN_POINT ( 'NONE',  ( 0.04760578872586663374, -0.3171112559587725976, -0.3633058139840105172 ) ) ;
#12438 = ORIENTED_EDGE ( 'NONE', *, *, #7133, .T. ) ;
#12439 = CARTESIAN_POINT ( 'NONE',  ( 0.1625622452632755621, -0.7569282882511942923, 0.5806955612166369018 ) ) ;
#12440 = EDGE_LOOP ( 'NONE', ( #32024, #40601, #34033, #24006 ) ) ;
#12441 = EDGE_CURVE ( 'NONE', #2376, #13090, #20625, .T. ) ;
#12442 = CARTESIAN_POINT ( 'NONE',  ( 0.6672263256168233791, -1.559577713309469038, 0.6159734170043378310 ) ) ;
#12443 = CARTESIAN_POINT ( 'NONE',  ( 0.3944496393030803016, -1.402754858333492338, 0.8483264674520886173 ) ) ;
#12445 = CARTESIAN_POINT ( 'NONE',  ( 0.07500000000000131561, -0.2899999999999966493, -1.126887297386508504E-15 ) ) ;
#12444 = LINE ( 'NONE', #40217, #2675 ) ;
#12446 = LINE ( 'NONE', #15734, #14569 ) ;
#12447 = DIRECTION ( 'NONE',  ( -7.771561172376107616E-16, 7.170354002788761615E-17, -1.000000000000000000 ) ) ;
#12448 = EDGE_CURVE ( 'NONE', #23678, #10838, #31130, .T. ) ;
#12449 = PRODUCT_DEFINITION_CONTEXT ( 'detailed design', #36864, 'design' ) ;
#12450 = CARTESIAN_POINT ( 'NONE',  ( 0.3999999999999783729, -2.120664306612643824, -0.5256090310107810470 ) ) ;
#12451 = CARTESIAN_POINT ( 'NONE',  ( 0.1153471661799269632, -0.4465907051537382211, 0.1385946963835902879 ) ) ;
#12452 = EDGE_CURVE ( 'NONE', #19176, #8492, #33581, .T. ) ;
#12453 = CARTESIAN_POINT ( 'NONE',  ( 0.1266980462273043506, -0.5766536709655731840, 0.2577630623947261834 ) ) ;
#12454 = CARTESIAN_POINT ( 'NONE',  ( 0.4655920101359526941, -1.672100886989639656, 0.4503321976353596989 ) ) ;
#12455 = CARTESIAN_POINT ( 'NONE',  ( -0.04582889109739283345, 0.3361233334070998779, 0.3523147457849521436 ) ) ;
#12456 = LINE ( 'NONE', #2597, #27745 ) ;
#12457 = CARTESIAN_POINT ( 'NONE',  ( -0.1212602504878780296, -0.5073146173917506552, 0.1528658435936999238 ) ) ;
#12458 = FACE_BOUND ( 'NONE', #31551, .T. ) ;
#12459 = CARTESIAN_POINT ( 'NONE',  ( 0.2198287030041630452, -1.240152648543706881, 0.4626484354544510569 ) ) ;
#12460 = CARTESIAN_POINT ( 'NONE',  ( 0.5405998635167484911, -1.177347015163466182, 0.8538091603066587654 ) ) ;
#12461 = CARTESIAN_POINT ( 'NONE',  ( -0.04308745346420277816, 0.3346348984074301591, 0.3638093623074960536 ) ) ;
#12462 = EDGE_CURVE ( 'NONE', #37622, #10331, #10100, .T. ) ;
#12463 = CARTESIAN_POINT ( 'NONE',  ( 0.05294255105929539240, -1.287813536604528686, 0.6347874768812761248 ) ) ;
#12464 = CARTESIAN_POINT ( 'NONE',  ( 0.03113248654051816583, -0.02383748379410547888, -0.1985743547550029575 ) ) ;
#12465 = CARTESIAN_POINT ( 'NONE',  ( 0.3939451924134707017, -1.988462716268693864, -0.4923357761437431313 ) ) ;
#12466 = DIRECTION ( 'NONE',  ( 0.000000000000000000, 0.3420201433257253898, 0.9396926207858877778 ) ) ;
#12467 = CARTESIAN_POINT ( 'NONE',  ( 0.07811717810578562571, 0.05441343863104618900, 0.1146970785768719608 ) ) ;
#12468 = CARTESIAN_POINT ( 'NONE',  ( -0.02000000000000000042, -2.626773565144302935, -0.2726934094652516127 ) ) ;
#12469 = EDGE_LOOP ( 'NONE', ( #20554, #8857 ) ) ;
#12470 = CARTESIAN_POINT ( 'NONE',  ( 0.3216048373150969253, -1.652200788492672823, 0.5182417262812423209 ) ) ;
#12471 = CARTESIAN_POINT ( 'NONE',  ( 0.5709871546789997421, -1.412948679733850410, 0.7285269761084822715 ) ) ;
#12472 = CARTESIAN_POINT ( 'NONE',  ( 0.3623460565293080693, -1.967939423356526829, -0.4915828919187142931 ) ) ;
#12473 = CYLINDRICAL_SURFACE ( 'NONE', #38867, 0.1033070866141734129 ) ;
#12474 = CARTESIAN_POINT ( 'NONE',  ( -0.1603938765018562418, 0.4636889572247986369, 0.3382895567582878127 ) ) ;
#12475 = ORIENTED_EDGE ( 'NONE', *, *, #3848, .T. ) ;
#12476 = LINE ( 'NONE', #21753, #15178 ) ;
#12477 =( BOUNDED_SURFACE ( )  B_SPLINE_SURFACE ( 3, 2, ( 
 ( #24879, #14997, #25066 ),
 ( #37401, #24463, #2461 ),
 ( #31033, #30636, #220 ),
 ( #27746, #18478, #2853 ),
 ( #3252, #21590, #12714 ),
 ( #37819, #21395, #27550 ),
 ( #36996, #9635, #40073 ),
 ( #37599, #6127, #15402 ) ),
 .UNSPECIFIED., .F., .F., .T. ) 
 B_SPLINE_SURFACE_WITH_KNOTS ( ( 4, 2, 2, 4 ),
 ( 3, 3 ),
 ( 0.001363486440777415343, 0.002314916752335400337, 0.002790631908114392726, 0.003266347063893385548 ),
 ( 0.000000000000000000, 1.000000000000000000 ),
 .UNSPECIFIED. ) 
 GEOMETRIC_REPRESENTATION_ITEM ( )  RATIONAL_B_SPLINE_SURFACE ( (
 ( 1.000000000000000000, 0.9128709291753024369, 1.000000000000000000),
 ( 1.000000000000000000, 0.9128773865076781346, 1.000000000000000000),
 ( 1.000000000000000000, 0.9126892044518930547, 1.000000000000000000),
 ( 1.000000000000000000, 0.9123262075132244631, 1.000000000000000000),
 ( 1.000000000000000000, 0.9121926916490802340, 1.000000000000000000),
 ( 1.000000000000000000, 0.9119580040442082369, 1.000000000000000000),
 ( 1.000000000000000000, 0.9118544196726630080, 1.000000000000000000),
 ( 1.000000000000000000, 0.9117915798252037574, 1.000000000000000000) ) ) 
 REPRESENTATION_ITEM ( '' )  SURFACE ( )  );
#12478 = LINE ( 'NONE', #10220, #24973 ) ;
#12479 = DIRECTION ( 'NONE',  ( -1.000000000000000000, -2.280301054154495132E-31, 1.664003471950577689E-31 ) ) ;
#12480 = CARTESIAN_POINT ( 'NONE',  ( 0.05201840200954559873, 0.2617120493658921521, -0.3909676859878664090 ) ) ;
#12481 = CARTESIAN_POINT ( 'NONE',  ( 0.4936674894353650922, -1.281362546945149505, 0.6421980442539246825 ) ) ;
#12483 = CARTESIAN_POINT ( 'NONE',  ( 0.07006815180908280982, -1.315301596572416631, 0.5080907171456734428 ) ) ;
#12482 = DIRECTION ( 'NONE',  ( 0.3981087504120406351, -0.9173382270707808317, 0.000000000000000000 ) ) ;
#12484 = CARTESIAN_POINT ( 'NONE',  ( 0.4434061351937851336, -1.055534433944394390, 0.6333734109485414931 ) ) ;
#12485 = EDGE_LOOP ( 'NONE', ( #34503, #28051, #16894, #6639 ) ) ;
#12486 = PERSON_AND_ORGANIZATION ( #28500, #32463 ) ;
#12487 = B_SPLINE_CURVE_WITH_KNOTS ( 'NONE', 3,
 ( #35529, #35951, #26111, #17027, #10860, #29169 ),
 .UNSPECIFIED., .F., .F.,
 ( 4, 2, 4 ),
 ( 0.000000000000000000, 0.5000000000000000000, 1.000000000000000000 ),
 .UNSPECIFIED. ) ;
#12488 = CARTESIAN_POINT ( 'NONE',  ( 0.1048591973540500683, -1.410537849644770025, 0.5682417262808777680 ) ) ;
#12489 = EDGE_LOOP ( 'NONE', ( #27484, #15497, #29800, #12750 ) ) ;
#12490 = EDGE_CURVE ( 'NONE', #32251, #15168, #16678, .T. ) ;
#12491 = ORIENTED_EDGE ( 'NONE', *, *, #34164, .T. ) ;
#12492 = CARTESIAN_POINT ( 'NONE',  ( 0.3850832117555434420, -1.605563056493195750, 0.5719009434103851097 ) ) ;
#12494 = CARTESIAN_POINT ( 'NONE',  ( 0.1868996193594879007, -0.6130910221644165770, -0.004499342026776794248 ) ) ;
#12493 = CARTESIAN_POINT ( 'NONE',  ( 0.06660359447752162154, -0.7066512958380626319, -0.0009978780739624637606 ) ) ;
#12495 = CARTESIAN_POINT ( 'NONE',  ( 0.06870814706323993826, -0.5548752703722420465, 0.08030761319108148388 ) ) ;
#12496 = ORIENTED_EDGE ( 'NONE', *, *, #25745, .F. ) ;
#12497 = ADVANCED_FACE ( 'NONE', ( #20236 ), #9442, .T. ) ;
#12498 = AXIS2_PLACEMENT_3D ( 'NONE', #21418, #18716, #30659 ) ;
#12499 = ORIENTED_EDGE ( 'NONE', *, *, #30840, .T. ) ;
#12500 = EDGE_LOOP ( 'NONE', ( #30613, #14124, #1145, #13099 ) ) ;
#12501 = CARTESIAN_POINT ( 'NONE',  ( 0.4649110479086845382, -1.060769885487067965, 0.6308327102990411994 ) ) ;
#12502 = AXIS2_PLACEMENT_3D ( 'NONE', #39557, #11391, #23963 ) ;
#12503 = CARTESIAN_POINT ( 'NONE',  ( 0.2053702793495189582, -0.8326540434915299382, 0.6524417661613786112 ) ) ;
#12504 = ORIENTED_EDGE ( 'NONE', *, *, #14200, .F. ) ;
#12505 = CARTESIAN_POINT ( 'NONE',  ( 0.01128677947712186484, -0.9461986806730106059, 0.1457185332388702959 ) ) ;
#12506 = CARTESIAN_POINT ( 'NONE',  ( 0.1487712572053581650, -1.705599614157317534, -0.3615038741254806287 ) ) ;
#12507 = PLANE ( 'NONE',  #13228 ) ;
#12508 = VECTOR ( 'NONE', #8429, 39.37007874015748854 ) ;
#12509 = CARTESIAN_POINT ( 'NONE',  ( 0.02317555983421318300, -1.616538932131220241, -0.3753236664589540972 ) ) ;
#12510 = EDGE_CURVE ( 'NONE', #5283, #13008, #7854, .T. ) ;
#12511 = CARTESIAN_POINT ( 'NONE',  ( 0.3999999999999786504, -1.971318270955308982, -0.3048432623593835822 ) ) ;
#12512 = CARTESIAN_POINT ( 'NONE',  ( 0.4271456124369221174, -1.696040845303949940, 0.4245472146382419654 ) ) ;
#12513 = DIRECTION ( 'NONE',  ( -0.8660512985181135770, -0.4999551463232371207, 0.000000000000000000 ) ) ;
#12514 = CARTESIAN_POINT ( 'NONE',  ( 0.1014370313544829955, -1.288984516341279196, 0.6101567855675421592 ) ) ;
#12515 = ADVANCED_FACE ( 'NONE', ( #29287 ), #36643, .T. ) ;
#12516 = CARTESIAN_POINT ( 'NONE',  ( 0.3520925652409914175, -1.512544934550680287, -0.7187326247832951376 ) ) ;
#12517 = DIRECTION ( 'NONE',  ( 1.000000000000000000, 2.280301054154495132E-31, -1.664003471950577689E-31 ) ) ;
#12518 = DATE_AND_TIME ( #28165, #27265 ) ;
#12519 = ADVANCED_FACE ( 'NONE', ( #36664 ), #19814, .T. ) ;
#12520 = CARTESIAN_POINT ( 'NONE',  ( 0.4897881687547872565, -1.080982661159355818, 0.5914788577480112330 ) ) ;
#12521 = EDGE_CURVE ( 'NONE', #30458, #394, #39749, .T. ) ;
#12522 = CARTESIAN_POINT ( 'NONE',  ( 0.3504057387187116679, -1.153664717295437070, 0.4422128889498895266 ) ) ;
#12523 = CARTESIAN_POINT ( 'NONE',  ( 0.06486471661944531730, -1.341257090703712240, 0.5604528108220497851 ) ) ;
#12524 = B_SPLINE_CURVE_WITH_KNOTS ( 'NONE', 3,
 ( #24477, #6748, #34737, #19326, #38031, #31867, #25497, #3683, #31459, #13129, #638, #4066, #7146, #38226, #25693, #15817, #28370, #25298, #236, #19713, #10054, #22624, #32243, #10272, #25912, #9651, #16242, #12732, #3871, #22021, #22834, #28780, #37838, #6542, #16631, #22219, #35160, #16032, #19118, #6959, #13339, #29177, #38432 ),
 .UNSPECIFIED., .F., .F.,
 ( 4, 2, 2, 2, 2, 2, 2, 2, 2, 2, 2, 2, 2, 1, 2, 2, 2, 2, 2, 2, 2, 4 ),
 ( 0.000000000000000000, 0.001251999155498175918, 0.002503998310996351836, 0.003129997888745439036, 0.003755997466494526670, 0.005007996621992698467, 0.006259995777490869398, 0.006885995355239957899, 0.007511994932989045533, 0.008763994088487214729, 0.01001599324398538479, 0.01126799239948355659, 0.01189399197723264162, 0.01251999155498172665, 0.01314599113273081515, 0.01377199071047990019, 0.01502398986597806851, 0.01627598902147623858, 0.01752798817697440517, 0.01815398775472349194, 0.01877998733247257523, 0.02003198648797073489 ),
 .UNSPECIFIED. ) ;
#12525 = CARTESIAN_POINT ( 'NONE',  ( 0.5616682974235900350, -1.585511599874633193, -0.5166151207188732775 ) ) ;
#12526 = CARTESIAN_POINT ( 'NONE',  ( 0.1877024697326355740, -1.541847387273544756, 0.6461194557730155497 ) ) ;
#12527 = CARTESIAN_POINT ( 'NONE',  ( 0.3453377680719361131, -1.749458763706787545, 0.4498113177181523037 ) ) ;
#12528 = CARTESIAN_POINT ( 'NONE',  ( 0.6522089892707538805, -1.452491178199303956, 0.4224083929475448973 ) ) ;
#12529 = AXIS2_PLACEMENT_3D ( 'NONE', #7467, #20046, #4393 ) ;
#12530 = CARTESIAN_POINT ( 'NONE',  ( 0.3545136070857681787, -1.624373116762336755, 0.4807375746916207615 ) ) ;
#12531 = ORIENTED_EDGE ( 'NONE', *, *, #23159, .F. ) ;
#12532 = VERTEX_POINT ( 'NONE', #8885 ) ;
#12533 = DIRECTION ( 'NONE',  ( -1.416619696839557898E-11, 0.000000000000000000, 1.000000000000000000 ) ) ;
#12534 = ORIENTED_EDGE ( 'NONE', *, *, #8679, .T. ) ;
#12535 = FACE_OUTER_BOUND ( 'NONE', #3883, .T. ) ;
#12536 = CARTESIAN_POINT ( 'NONE',  ( -0.05283102792148778454, -0.4315398646667463756, -0.1819478359276366641 ) ) ;
#12537 = AXIS2_PLACEMENT_3D ( 'NONE', #17961, #39775, #11605 ) ;
#12538 = CARTESIAN_POINT ( 'NONE',  ( 0.5762847659421821422, -1.421719372835159589, 0.7207317226011845657 ) ) ;
#12540 = VERTEX_POINT ( 'NONE', #33985 ) ;
#12539 = DIRECTION ( 'NONE',  ( 0.000000000000000000, 0.5877852522924701395, -0.8090169943749495607 ) ) ;
#12541 = ORIENTED_EDGE ( 'NONE', *, *, #19080, .T. ) ;
#12542 = CYLINDRICAL_SURFACE ( 'NONE', #26462, 0.03749999999977554621 ) ;
#12543 = VERTEX_POINT ( 'NONE', #15260 ) ;
#12544 = CARTESIAN_POINT ( 'NONE',  ( 0.01152972583212505224, -0.5524291824619802505, 0.2505810646121844343 ) ) ;
#12545 = DIRECTION ( 'NONE',  ( 0.8660512985181134660, 0.4999551463232371762, 0.000000000000000000 ) ) ;
#12546 = CARTESIAN_POINT ( 'NONE',  ( 0.3945306638533003230, -1.754969121428254342, -0.4915120835733784999 ) ) ;
#12547 = EDGE_CURVE ( 'NONE', #20195, #10465, #17549, .T. ) ;
#12548 = CARTESIAN_POINT ( 'NONE',  ( 0.4103187208584767043, -1.720663819739514100, -0.4253394185160298546 ) ) ;
#12550 = ORIENTED_EDGE ( 'NONE', *, *, #18803, .F. ) ;
#12549 = ORIENTED_EDGE ( 'NONE', *, *, #38433, .T. ) ;
#12551 = EDGE_CURVE ( 'NONE', #22278, #27442, #5467, .T. ) ;
#12552 = CARTESIAN_POINT ( 'NONE',  ( 0.1850410792612997846, -0.8547936666690651997, 0.1477569985384105389 ) ) ;
#12553 = CARTESIAN_POINT ( 'NONE',  ( 0.3505769137777456912, -1.738054031222972862, 0.4360220170068370704 ) ) ;
#12554 = CARTESIAN_POINT ( 'NONE',  ( -0.02000000000000000042, -2.626773565144302935, -0.2526934094652523721 ) ) ;
#12555 = CARTESIAN_POINT ( 'NONE',  ( 0.2867526321560044944, -0.9860951448986656764, 0.7283370995064215592 ) ) ;
#12556 = LINE ( 'NONE', #19150, #38255 ) ;
#12557 = CARTESIAN_POINT ( 'NONE',  ( 0.2735777270575741604, -1.648034364121254036, 0.7523254439293706186 ) ) ;
#12558 = CARTESIAN_POINT ( 'NONE',  ( 0.3224542088160151643, -1.759949008389460223, 0.6236646122038994600 ) ) ;
#12559 = AXIS2_PLACEMENT_3D ( 'NONE', #2849, #5729, #34110 ) ;
#12560 = DIRECTION ( 'NONE',  ( 0.4999999999999963918, -0.6509737717187614736, 0.5711682313769329555 ) ) ;
#12561 = VECTOR ( 'NONE', #32413, 39.37007874015748854 ) ;
#12562 = DIRECTION ( 'NONE',  ( -1.000000000000000000, -2.280301054154495132E-31, 1.664003471950577689E-31 ) ) ;
#12563 = DIRECTION ( 'NONE',  ( -0.4999551463232377313, 0.8660512985181132439, -0.000000000000000000 ) ) ;
#12564 = DIRECTION ( 'NONE',  ( -1.000000000000000000, -2.403560570595279103E-31, 1.725633230170969455E-31 ) ) ;
#12565 = DIRECTION ( 'NONE',  ( 1.000000000000000000, 0.000000000000000000, -2.374158975444574710E-12 ) ) ;
#12566 = CIRCLE ( 'NONE', #35551, 0.08830708661417320526 ) ;
#12567 = VECTOR ( 'NONE', #15270, 39.37007874015748143 ) ;
#12568 = FACE_OUTER_BOUND ( 'NONE', #6567, .T. ) ;
#12569 = DIRECTION ( 'NONE',  ( 1.000000000000000000, 2.341930812374887555E-31, -1.664003471950578127E-31 ) ) ;
#12570 = CARTESIAN_POINT ( 'NONE',  ( 0.09482598954113068135, -1.341677941020415377, 0.6974875476592315993 ) ) ;
#12571 = APPROVAL_STATUS ( 'not_yet_approved' ) ;
#12572 = CARTESIAN_POINT ( 'NONE',  ( 0.6712941330769894854, -1.387165532388958678, 0.7909734157804186871 ) ) ;
#12573 = CARTESIAN_POINT ( 'NONE',  ( -0.04575106512774497480, 0.4390484599015530565, 0.2110503898921227695 ) ) ;
#12574 = CARTESIAN_POINT ( 'NONE',  ( 0.6803383295583191881, -1.562882757458972982, 0.6028934748675488509 ) ) ;
#12575 = CARTESIAN_POINT ( 'NONE',  ( 0.02953079040095704308, -0.3810518745593846068, 0.3687679460475796756 ) ) ;
#12576 = CARTESIAN_POINT ( 'NONE',  ( -0.05464101615137786222, -2.196538720661423749, -0.6552417777791260667 ) ) ;
#12577 = ORIENTED_EDGE ( 'NONE', *, *, #23579, .T. ) ;
#12578 = CARTESIAN_POINT ( 'NONE',  ( -0.07999999999999998779, -2.180132361182266720, -0.6941833704005058170 ) ) ;
#12579 = CARTESIAN_POINT ( 'NONE',  ( 0.2649388293739690647, -1.647471256193353994, 0.7673347028883034104 ) ) ;
#12580 = CIRCLE ( 'NONE', #4025, 0.1700000000000000400 ) ;
#12581 = CARTESIAN_POINT ( 'NONE',  ( 0.5948448836580337851, -1.487180068494697860, 0.5714582431182474442 ) ) ;
#12583 = ORIENTED_EDGE ( 'NONE', *, *, #14510, .T. ) ;
#12582 = FACE_OUTER_BOUND ( 'NONE', #1633, .T. ) ;
#12584 = CARTESIAN_POINT ( 'NONE',  ( 0.5555567715531690709, -1.190973094708358992, 0.5709149340790615756 ) ) ;
#12586 = VERTEX_POINT ( 'NONE', #37462 ) ;
#12585 = EDGE_LOOP ( 'NONE', ( #35546, #14941, #9240, #15760 ) ) ;
#12587 = CARTESIAN_POINT ( 'NONE',  ( 0.3155498261607609933, -0.8427994992563406784, 0.6561175494744075909 ) ) ;
#12588 = AXIS2_PLACEMENT_3D ( 'NONE', #29041, #38702, #909 ) ;
#12589 = AXIS2_PLACEMENT_3D ( 'NONE', #24666, #11881, #14782 ) ;
#12590 = CARTESIAN_POINT ( 'NONE',  ( 0.3601834888757650122, -1.721134795303484788, -0.5614851183221652997 ) ) ;
#12591 = CARTESIAN_POINT ( 'NONE',  ( 0.6104845410980109799, -1.615235805367044808, -0.5028569573147162464 ) ) ;
#12592 = CALENDAR_DATE ( 2026, 13, 10 ) ;
#12593 = CIRCLE ( 'NONE', #8650, 0.01000000000000002970 ) ;
#12594 = CARTESIAN_POINT ( 'NONE',  ( -0.2399999999999999079, -2.511040369707300268, -0.5948468226404902692 ) ) ;
#12595 = ORIENTED_EDGE ( 'NONE', *, *, #28253, .F. ) ;
#12596 = CARTESIAN_POINT ( 'NONE',  ( 0.08944029709302749043, -0.7717967997121178980, 0.2508382323318106844 ) ) ;
#12597 = B_SPLINE_CURVE_WITH_KNOTS ( 'NONE', 3,
 ( #31806, #13080, #25445, #38168, #9375, #34881 ),
 .UNSPECIFIED., .F., .F.,
 ( 4, 2, 4 ),
 ( 0.000000000000000000, 0.0007264914290232497678, 0.001452982858046499536 ),
 .UNSPECIFIED. ) ;
#12598 = CARTESIAN_POINT ( 'NONE',  ( 0.4115766028365042128, -1.733048369835246794, 0.5182417262812423209 ) ) ;
#12599 = CARTESIAN_POINT ( 'NONE',  ( 0.5251744434789910043, -1.526859942859090324, 0.5727264815542076892 ) ) ;
#12600 = CARTESIAN_POINT ( 'NONE',  ( 0.3926032618789407347, -1.756026311479913948, -0.5284552501753293496 ) ) ;
#12601 = CARTESIAN_POINT ( 'NONE',  ( -0.1612862774928120191, 0.5009394326984835111, 0.1071084547149960403 ) ) ;
#12602 = ORIENTED_EDGE ( 'NONE', *, *, #31760, .F. ) ;
#12603 = CARTESIAN_POINT ( 'NONE',  ( 0.4581770189839536878, -1.680087630256094755, 0.5962093605133977903 ) ) ;
#12604 = CARTESIAN_POINT ( 'NONE',  ( 0.6989095468901158625, -1.435512049448604444, 0.6261787951156853049 ) ) ;
#12605 = DIRECTION ( 'NONE',  ( 0.8660512985181126888, 0.4999551463232384529, 0.000000000000000000 ) ) ;
#12606 = CARTESIAN_POINT ( 'NONE',  ( 0.5750439247535107379, -1.432704706222420521, 0.7403086931740429089 ) ) ;
#12607 = CARTESIAN_POINT ( 'NONE',  ( 0.000000000000000000, 0.000000000000000000, 0.000000000000000000 ) ) ;
#12608 = LINE ( 'NONE', #3770, #30627 ) ;
#12609 = CARTESIAN_POINT ( 'NONE',  ( 0.2679554415261233280, -1.674078903935640517, 0.5221304914950548604 ) ) ;
#12610 = FACE_OUTER_BOUND ( 'NONE', #32459, .T. ) ;
#12611 = CARTESIAN_POINT ( 'NONE',  ( 0.2467813525974754951, -0.8519813862200177335, 0.4954293255957377684 ) ) ;
#12612 = APPROVAL_DATE_TIME ( #115, #33271 ) ;
#12613 = AXIS2_PLACEMENT_3D ( 'NONE', #7383, #17069, #16276 ) ;
#12614 = CARTESIAN_POINT ( 'NONE',  ( -0.1669433606228599432, 0.5138636982738132852, 0.3032895567580801144 ) ) ;
#12615 = VECTOR ( 'NONE', #7724, 39.37007874015748854 ) ;
#12616 = LINE ( 'NONE', #19010, #1142 ) ;
#12617 = CARTESIAN_POINT ( 'NONE',  ( -0.05281452789367579309, 0.03978571835447197030, 0.4666805157975088547 ) ) ;
#12618 = ORIENTED_EDGE ( 'NONE', *, *, #1471, .T. ) ;
#12619 = CARTESIAN_POINT ( 'NONE',  ( -0.3000000000000000999, -3.840189043187996809, -0.1239867222638698224 ) ) ;
#12620 = CARTESIAN_POINT ( 'NONE',  ( -0.2399999999999999079, -3.941790907013290823, -0.4709369376873030477 ) ) ;
#12621 = CARTESIAN_POINT ( 'NONE',  ( 0.08510361377861434817, -0.8106636051554854117, 0.1454306519311501233 ) ) ;
#12622 = ORIENTED_EDGE ( 'NONE', *, *, #33570, .F. ) ;
#12623 = CARTESIAN_POINT ( 'NONE',  ( 0.4970758107849645446, -1.079867600816170059, 0.3667417262808778666 ) ) ;
#12624 = CARTESIAN_POINT ( 'NONE',  ( -0.007649408449226275004, -0.8869281924019897234, 0.4775367515392046069 ) ) ;
#12626 = ORIENTED_EDGE ( 'NONE', *, *, #11986, .T. ) ;
#12625 = ORIENTED_EDGE ( 'NONE', *, *, #38566, .T. ) ;
#12627 = CARTESIAN_POINT ( 'NONE',  ( -0.2399999999999999079, -3.941790907013290823, -0.4709369376873030477 ) ) ;
#12628 = ORIENTED_EDGE ( 'NONE', *, *, #26817, .T. ) ;
#12629 = CARTESIAN_POINT ( 'NONE',  ( 0.3259879919982042185, -1.767950897709266611, 0.5312986935552648227 ) ) ;
#12630 = CARTESIAN_POINT ( 'NONE',  ( 0.3699999999999789568, -2.050772785069567838, -0.3050017341552425654 ) ) ;
#12632 = DIRECTION ( 'NONE',  ( -0.4709550870498624975, 0.000000000000000000, 0.8821571889305536152 ) ) ;
#12631 = CARTESIAN_POINT ( 'NONE',  ( 0.05544444631433361609, 0.4320262549500614169, 0.1617187101067886490 ) ) ;
#12633 = CARTESIAN_POINT ( 'NONE',  ( 0.04230170315644249390, -0.2684795119051844869, -0.3841679273482348500 ) ) ;
#12634 = ORIENTED_EDGE ( 'NONE', *, *, #28363, .F. ) ;
#12635 = CARTESIAN_POINT ( 'NONE',  ( 0.09015709819048388363, -0.5643440796219489908, 0.1782129044586291677 ) ) ;
#12636 = ORIENTED_EDGE ( 'NONE', *, *, #1033, .F. ) ;
#12637 = VERTEX_POINT ( 'NONE', #31319 ) ;
#12638 = VECTOR ( 'NONE', #36229, 39.37007874015748143 ) ;
#12639 = CARTESIAN_POINT ( 'NONE',  ( -0.07999999999999998779, -2.367354784411275670, -0.3586747285825516718 ) ) ;
#12640 = CARTESIAN_POINT ( 'NONE',  ( 0.07460218941637257462, -0.5676562956907557078, 0.2601178745213920673 ) ) ;
#12641 = ADVANCED_FACE ( 'NONE', ( #6961 ), #2923, .T. ) ;
#12643 = CARTESIAN_POINT ( 'NONE',  ( 0.5558855420699814198, -1.622948660481935423, 0.5440994406646009196 ) ) ;
#12642 = CARTESIAN_POINT ( 'NONE',  ( 0.4346145078518607874, -1.592046523758374077, -0.4178586084682519575 ) ) ;
#12644 = CARTESIAN_POINT ( 'NONE',  ( 0.006145725594649042133, -0.8471966322199038224, 0.2388777800840232446 ) ) ;
#12645 = CARTESIAN_POINT ( 'NONE',  ( 0.3349327071708561587, -0.9960187932710996561, 0.5970633004496839202 ) ) ;
#12646 = APPLIED_DATE_AND_TIME_ASSIGNMENT ( #24342, #11786, ( #24074 ) ) ;
#12647 = AXIS2_PLACEMENT_3D ( 'NONE', #19937, #35772, #4298 ) ;
#12648 = DIRECTION ( 'NONE',  ( 1.000000000000000000, 6.779273404243070203E-32, 4.314083075427408311E-32 ) ) ;
#12649 = CARTESIAN_POINT ( 'NONE',  ( 0.1897125635009227207, -0.5340696856102284951, 0.1480337217182641774 ) ) ;
#12650 = CARTESIAN_POINT ( 'NONE',  ( 0.5808183205011048234, -1.495242300261638402, 0.5715967477096820515 ) ) ;
#12651 = CARTESIAN_POINT ( 'NONE',  ( -0.05186792262756997896, 0.2910804482542271310, -0.3700673534428220446 ) ) ;
#12652 = TOROIDAL_SURFACE ( 'NONE', #9363, 0.9237847906030132172, 0.01499999999999999944 ) ;
#12653 = FACE_OUTER_BOUND ( 'NONE', #36417, .T. ) ;
#12654 = DIRECTION ( 'NONE',  ( 0.000000000000000000, 0.5877852522924830181, 0.8090169943749403458 ) ) ;
#12655 = CARTESIAN_POINT ( 'NONE',  ( 0.4937576479559093179, -1.320126057825392607, 0.8099836062144650795 ) ) ;
#12656 = FACE_OUTER_BOUND ( 'NONE', #36630, .T. ) ;
#12657 = CARTESIAN_POINT ( 'NONE',  ( 0.4077406957728484382, -0.9605384586880818532, 0.7982698588713066368 ) ) ;
#12658 = CARTESIAN_POINT ( 'NONE',  ( -0.05252359774140260423, 0.2829835766811606979, 0.3741004571325340922 ) ) ;
#12659 = CARTESIAN_POINT ( 'NONE',  ( 0.04514759861635499888, -1.211207050343567238, 0.6773524313334282621 ) ) ;
#12660 = AXIS2_PLACEMENT_3D ( 'NONE', #16020, #32049, #23213 ) ;
#12661 = CARTESIAN_POINT ( 'NONE',  ( 0.6299088991424890427, -1.603889269770004233, -0.4524234554939136621 ) ) ;
#12662 = CARTESIAN_POINT ( 'NONE',  ( -0.02000000000000000042, -2.626773565144302935, -0.2726934094652516127 ) ) ;
#12663 = EDGE_CURVE ( 'NONE', #17796, #3309, #6543, .T. ) ;
#12664 = CARTESIAN_POINT ( 'NONE',  ( 0.06443582809897516195, -0.8352844082134175396, 0.1913173570483421015 ) ) ;
#12665 = DIRECTION ( 'NONE',  ( 7.000205099780314469E-17, 1.000000000000000000, -6.590151126658399604E-16 ) ) ;
#12666 = DIRECTION ( 'NONE',  ( 0.000000000000000000, 0.000000000000000000, -1.000000000000000000 ) ) ;
#12667 = EDGE_CURVE ( 'NONE', #23137, #26169, #22765, .T. ) ;
#12668 = CONICAL_SURFACE ( 'NONE', #5406, 0.1400000000000010403, 1.047197551196600962 ) ;
#12669 = VECTOR ( 'NONE', #34383, 39.37007874015748854 ) ;
#12670 = ORIENTED_EDGE ( 'NONE', *, *, #18217, .T. ) ;
#12671 = CARTESIAN_POINT ( 'NONE',  ( -0.01548846960707517956, -0.3772621329472692908, -0.3651003739303438911 ) ) ;
#12672 = CARTESIAN_POINT ( 'NONE',  ( 0.3988135775770819680, -1.610682515506242751, -0.3616878989671591382 ) ) ;
#12673 = CIRCLE ( 'NONE', #159, 0.03000000000000003358 ) ;
#12674 = ADVANCED_FACE ( 'NONE', ( #32457 ), #38336, .F. ) ;
#12675 = CARTESIAN_POINT ( 'NONE',  ( 0.6521185033023405575, -1.542907011849279364, 0.4182417262808776348 ) ) ;
#12676 = CARTESIAN_POINT ( 'NONE',  ( 0.5375949106523618681, -1.667153108916268334, -0.4581832398558707831 ) ) ;
#12677 = ADVANCED_FACE ( 'NONE', ( #3127 ), #29181, .F. ) ;
#12678 = LINE ( 'NONE', #13503, #34431 ) ;
#12679 = EDGE_CURVE ( 'NONE', #34509, #28442, #15666, .T. ) ;
#12680 = CIRCLE ( 'NONE', #35686, 0.7043128707267513056 ) ;
#12681 = VERTEX_POINT ( 'NONE', #35358 ) ;
#12682 = CARTESIAN_POINT ( 'NONE',  ( 0.3590659390023258624, -1.625695363421262973, -0.6613478498294523833 ) ) ;
#12683 =( GEOMETRIC_REPRESENTATION_CONTEXT ( 3 ) GLOBAL_UNCERTAINTY_ASSIGNED_CONTEXT ( ( #30969 ) ) GLOBAL_UNIT_ASSIGNED_CONTEXT ( ( #14030, #29274, #19800 ) ) REPRESENTATION_CONTEXT ( 'NONE', 'WORKASPACE' ) );
#12684 = CARTESIAN_POINT ( 'NONE',  ( 0.2594029906281075104, -1.332806731452343962, 0.4172623082385037430 ) ) ;
#12685 = CARTESIAN_POINT ( 'NONE',  ( 0.4469231120930088896, -1.683251538248273338, 0.4316885541138326121 ) ) ;
#12686 = CARTESIAN_POINT ( 'NONE',  ( 0.04760578872586526678, 0.2475315945985601951, -0.4138583970464100315 ) ) ;
#12687 = CARTESIAN_POINT ( 'NONE',  ( 0.5110404537384164447, -1.311648276678567093, 0.6104441183122480963 ) ) ;
#12689 = CYLINDRICAL_SURFACE ( 'NONE', #8265, 0.4488493849861021623 ) ;
#12688 = DIRECTION ( 'NONE',  ( 0.000000000000000000, -0.5781348229923758408, 0.8159412518334724362 ) ) ;
#12690 = CARTESIAN_POINT ( 'NONE',  ( 0.4929465528686921005, -1.082715557938388029, 0.5682417262808779901 ) ) ;
#12691 = VERTEX_POINT ( 'NONE', #28215 ) ;
#12692 = APPROVAL_STATUS ( 'not_yet_approved' ) ;
#12693 = DIRECTION ( 'NONE',  ( -1.000000000000000000, -0.000000000000000000, -0.000000000000000000 ) ) ;
#12694 = EDGE_LOOP ( 'NONE', ( #15597, #7900, #11531, #16479 ) ) ;
#12695 = CARTESIAN_POINT ( 'NONE',  ( 0.05229530933811773336, -0.6522472549805439224, 0.4589227677422883511 ) ) ;
#12696 = ADVANCED_FACE ( 'NONE', ( #7148 ), #19967, .T. ) ;
#12698 = CARTESIAN_POINT ( 'NONE',  ( 0.1754198919089409725, -0.8045108718813741566, -0.05231893310831398081 ) ) ;
#12697 = CARTESIAN_POINT ( 'NONE',  ( 0.06525845452225115251, -0.8048554632036153400, 0.05552589205823528495 ) ) ;
#12699 = CARTESIAN_POINT ( 'NONE',  ( 0.06897536523928704533, -0.5446676224100435171, 0.1075395329137426442 ) ) ;
#12700 = ORIENTED_EDGE ( 'NONE', *, *, #13484, .F. ) ;
#12701 = AXIS2_PLACEMENT_3D ( 'NONE', #9374, #21954, #34481 ) ;
#12702 = VERTEX_POINT ( 'NONE', #4069 ) ;
#12703 = EDGE_LOOP ( 'NONE', ( #43, #15218, #35484, #17799 ) ) ;
#12704 = CARTESIAN_POINT ( 'NONE',  ( 0.4933397991863339715, -1.083186959060361332, 0.5723784735904143828 ) ) ;
#12705 = CARTESIAN_POINT ( 'NONE',  ( 0.5679494682189658583, -1.502316997319172565, 0.6067939519441243323 ) ) ;
#12706 = ORIENTED_EDGE ( 'NONE', *, *, #10189, .F. ) ;
#12707 = CARTESIAN_POINT ( 'NONE',  ( 0.1873953661158407891, -0.6938363853788876989, 0.03552928613571013777 ) ) ;
#12708 = CARTESIAN_POINT ( 'NONE',  ( 0.5432513433150938376, -1.169106661975274353, 0.5798782747789370529 ) ) ;
#12709 = CARTESIAN_POINT ( 'NONE',  ( -0.2399999999999999079, -2.599675038826658735, -0.8213992999509311943 ) ) ;
#12710 = TOROIDAL_SURFACE ( 'NONE', #34379, 1.986674066779348768, 0.01499999999999999944 ) ;
#12711 = CIRCLE ( 'NONE', #1571, 0.6114999999999938263 ) ;
#12712 = DIRECTION ( 'NONE',  ( 0.000000000000000000, 6.829619984160658243E-15, -1.000000000000000000 ) ) ;
#12713 = SPHERICAL_SURFACE ( 'NONE', #13337, 0.01499999999999999944 ) ;
#12714 = CARTESIAN_POINT ( 'NONE',  ( -0.1196127869351430451, -0.4993621520964603988, 0.3258261256381426718 ) ) ;
#12715 = CARTESIAN_POINT ( 'NONE',  ( 0.08535460625685879765, -0.8121872720543428237, 0.1030692480275667428 ) ) ;
#12716 = EDGE_CURVE ( 'NONE', #31436, #10881, #2243, .T. ) ;
#12717 = VECTOR ( 'NONE', #5931, 39.37007874015748143 ) ;
#12718 = CARTESIAN_POINT ( 'NONE',  ( -0.2746410161513776482, -3.730063144961804245, -0.1064410973704723457 ) ) ;
#12719 = FACE_OUTER_BOUND ( 'NONE', #16427, .T. ) ;
#12720 = CARTESIAN_POINT ( 'NONE',  ( 0.09485889511719647338, -1.298679434850192216, 0.6031548665757355820 ) ) ;
#12721 = CARTESIAN_POINT ( 'NONE',  ( 0.2414668910093294429, -2.107936428766274073, -0.7005084057759867200 ) ) ;
#12722 = CARTESIAN_POINT ( 'NONE',  ( 0.09402968441108132402, -1.354797296243051008, 0.6996042430478996987 ) ) ;
#12723 = PERSON_AND_ORGANIZATION ( #28500, #32463 ) ;
#12724 = CARTESIAN_POINT ( 'NONE',  ( 0.5941217087312797851, -1.459610275592444273, 0.5526975506195443977 ) ) ;
#12725 = CARTESIAN_POINT ( 'NONE',  ( 0.2043866115177667420, -1.364383961788701249, 0.4807399974250947117 ) ) ;
#12726 = CARTESIAN_POINT ( 'NONE',  ( 0.06581764578086118922, -1.340728352476674212, 0.5449258910593480776 ) ) ;
#12727 = CARTESIAN_POINT ( 'NONE',  ( 0.2637142753222213587, -1.685688650057170390, 0.5655586431828601990 ) ) ;
#12728 = ADVANCED_FACE ( 'NONE', ( #5273 ), #35324, .T. ) ;
#12729 =( BOUNDED_SURFACE ( )  B_SPLINE_SURFACE ( 3, 2, ( 
 ( #17246, #29796, #1639 ),
 ( #23640, #14353, #26728 ),
 ( #39257, #31422, #12089 ),
 ( #24439, #193, #22183 ),
 ( #21369, #28135, #27721 ),
 ( #15987, #12686, #27934 ),
 ( #36972, #15588, #34291 ),
 ( #34696, #12480, #40257 ),
 ( #9187, #8791, #19074 ),
 ( #5892, #40647, #37186 ),
 ( #33907, #40474, #31612 ),
 ( #5704, #3428, #37788 ),
 ( #30806, #15773, #37571 ),
 ( #9004, #21756, #28319 ),
 ( #18261, #24855, #28532 ),
 ( #25246, #31005, #37375 ),
 ( #18883, #34500, #6503 ),
 ( #21566, #2627, #15162 ) ),
 .UNSPECIFIED., .F., .F., .T. ) 
 B_SPLINE_SURFACE_WITH_KNOTS ( ( 4, 2, 2, 2, 2, 2, 2, 2, 4 ),
 ( 3, 3 ),
 ( -0.001532620576208849244, -0.0007637936630077626476, 5.033250193323839973E-06, 0.0007738601633944103275, 0.001542687076595496923, 0.002311513989796583519, 0.003080340902997669682, 0.003849167816198756278, 0.004617994729399842874 ),
 ( 0.000000000000000000, 1.000000000000000000 ),
 .UNSPECIFIED. ) 
 GEOMETRIC_REPRESENTATION_ITEM ( )  RATIONAL_B_SPLINE_SURFACE ( (
 ( 1.000000000000000000, 0.7283825911960446486, 1.000000000000000000),
 ( 1.000000000000000000, 0.7404385082112820982, 1.000000000000000000),
 ( 1.000000000000000000, 0.7521504257740054822, 1.000000000000000000),
 ( 1.000000000000000000, 0.7744497410759803024, 1.000000000000000000),
 ( 1.000000000000000000, 0.7845654757373869970, 1.000000000000000000),
 ( 1.000000000000000000, 0.8022083990892319161, 1.000000000000000000),
 ( 1.000000000000000000, 0.8094167424698467395, 1.000000000000000000),
 ( 1.000000000000000000, 0.8194491993617468717, 1.000000000000000000),
 ( 1.000000000000000000, 0.8220634900780513510, 1.000000000000000000),
 ( 1.000000000000000000, 0.8220705070823443039, 1.000000000000000000),
 ( 1.000000000000000000, 0.8194468812481126019, 1.000000000000000000),
 ( 1.000000000000000000, 0.8094220769839290952, 1.000000000000000000),
 ( 1.000000000000000000, 0.8022659121984873076, 1.000000000000000000),
 ( 1.000000000000000000, 0.7845681159036136387, 1.000000000000000000),
 ( 1.000000000000000000, 0.7744426415186176360, 1.000000000000000000),
 ( 1.000000000000000000, 0.7522890290927783941, 1.000000000000000000),
 ( 1.000000000000000000, 0.7403540167216061674, 1.000000000000000000),
 ( 1.000000000000000000, 0.7283825911960206678, 1.000000000000000000) ) ) 
 REPRESENTATION_ITEM ( '' )  SURFACE ( )  );
#12730 = B_SPLINE_CURVE_WITH_KNOTS ( 'NONE', 3,
 ( #39677, #35992, #7798, #24079, #36788, #26751, #32889, #14373, #23868, #20975, #26939, #18087, #29824, #27365, #36392, #2260, #4701, #7995, #1667, #36603, #23661, #33307, #39279, #20573, #20783, #8408, #30432, #2045, #14799, #11103 ),
 .UNSPECIFIED., .F., .F.,
 ( 4, 2, 2, 2, 2, 2, 2, 2, 2, 2, 2, 2, 2, 2, 4 ),
 ( -5.999999999967792359E-08, 0.002163189985905394474, 0.004326439971810788591, 0.006489689957716177938, 0.007571314950668870010, 0.008652939943621561214, 0.01081618992952694709, 0.01189781492247964263, 0.01297943991543233817, 0.01406106490838503545, 0.01514268990133772926, 0.01568350239781407876, 0.01622431489429042653, 0.01676512739076677430, 0.01730593988724312207 ),
 .UNSPECIFIED. ) ;
#12731 = CARTESIAN_POINT ( 'NONE',  ( 0.1227332031174801358, -1.426450801877330088, 0.6430247681006037164 ) ) ;
#12732 = CARTESIAN_POINT ( 'NONE',  ( -0.0001212384970512573110, -0.7977683222466966928, -0.07773302012097864366 ) ) ;
#12733 = AXIS2_PLACEMENT_3D ( 'NONE', #20345, #33680, #5490 ) ;
#12734 = EDGE_CURVE ( 'NONE', #35767, #35465, #10872, .T. ) ;
#12735 = DIRECTION ( 'NONE',  ( 0.4999999999999984457, 3.389636702121524701E-32, -0.8660254037844394848 ) ) ;
#12736 = DIRECTION ( 'NONE',  ( -7.771561172376107616E-16, 7.170354002788761615E-17, -1.000000000000000000 ) ) ;
#12737 = EDGE_CURVE ( 'NONE', #33509, #5941, #39644, .T. ) ;
#12738 = ORIENTED_EDGE ( 'NONE', *, *, #1723, .T. ) ;
#12739 = TOROIDAL_SURFACE ( 'NONE', #35731, 0.5250000000000000222, 0.01499999999999999944 ) ;
#12740 = VERTEX_POINT ( 'NONE', #23445 ) ;
#12741 = VECTOR ( 'NONE', #30404, 39.37007874015748143 ) ;
#12742 = CARTESIAN_POINT ( 'NONE',  ( 0.04293317454820601980, -0.2295413494973341795, -0.4381202835071938417 ) ) ;
#12743 = ORIENTED_EDGE ( 'NONE', *, *, #6408, .T. ) ;
#12744 = CARTESIAN_POINT ( 'NONE',  ( 0.0004750592482352814579, -0.4386115460793976739, 0.1457185332388683252 ) ) ;
#12745 = CARTESIAN_POINT ( 'NONE',  ( 0.02235124290213170994, 0.2417860359143765847, 0.4518977707513289754 ) ) ;
#12746 = CARTESIAN_POINT ( 'NONE',  ( 0.4483952930911858648, -1.219233892752134230, 0.8146593353750180011 ) ) ;
#12748 = VERTEX_POINT ( 'NONE', #5081 ) ;
#12747 = CYLINDRICAL_SURFACE ( 'NONE', #9444, 0.9087847906030156464 ) ;
#12749 = AXIS2_PLACEMENT_3D ( 'NONE', #23393, #35910, #4227 ) ;
#12750 = ORIENTED_EDGE ( 'NONE', *, *, #8917, .F. ) ;
#12751 = CARTESIAN_POINT ( 'NONE',  ( 0.000000000000000000, -0.01499999999999997689, 0.000000000000000000 ) ) ;
#12752 = ORIENTED_EDGE ( 'NONE', *, *, #2958, .T. ) ;
#12753 = CARTESIAN_POINT ( 'NONE',  ( 0.01112738939452267463, -0.5460437306624825737, 0.2315852079017418352 ) ) ;
#12754 = ADVANCED_FACE ( 'NONE', ( #10658 ), #1628, .T. ) ;
#12756 = CARTESIAN_POINT ( 'NONE',  ( 0.1026681637763624949, -1.278312822899872581, 0.5960544170339612258 ) ) ;
#12755 = CARTESIAN_POINT ( 'NONE',  ( 0.5213450412171337645, -1.664948425110202246, -0.4412658265323602946 ) ) ;
#12757 = CARTESIAN_POINT ( 'NONE',  ( 0.3093710864688895557, -1.763897289999589280, 0.5510299488878679375 ) ) ;
#12758 = CARTESIAN_POINT ( 'NONE',  ( 0.1889626679396633202, -0.9196856789278203825, 0.008518417185872219008 ) ) ;
#12759 = ADVANCED_FACE ( 'NONE', ( #20752 ), #12739, .T. ) ;
#12760 = DIRECTION ( 'NONE',  ( 0.8660512985181133550, 0.4999551463232371207, 0.000000000000000000 ) ) ;
#12762 = ORIENTED_EDGE ( 'NONE', *, *, #2607, .F. ) ;
#12761 = ORIENTED_EDGE ( 'NONE', *, *, #30064, .F. ) ;
#12763 = EDGE_CURVE ( 'NONE', #4342, #30110, #6031, .T. ) ;
#12764 = FACE_OUTER_BOUND ( 'NONE', #35364, .T. ) ;
#12765 = PERSON ( 'NAUO-PER4', 'UNSPECIFIED', 'UNSPECIFIED', ('UNSPECIFIED'), ('UNSPECIFIED'), ('UNSPECIFIED') ) ;
#12766 = CARTESIAN_POINT ( 'NONE',  ( -0.04308745346419785849, -0.4494111352305510398, 0.2058334250444107671 ) ) ;
#12767 = PLANE ( 'NONE',  #24032 ) ;
#12768 = CARTESIAN_POINT ( 'NONE',  ( 0.2076380708292103194, -0.9071444418369396523, 0.6111425315318238516 ) ) ;
#12769 = CARTESIAN_POINT ( 'NONE',  ( 0.2715177313894526767, -1.674232447558412495, 0.6134098869104458451 ) ) ;
#12770 = AXIS2_PLACEMENT_3D ( 'NONE', #27833, #21261, #24341 ) ;
#12771 = CARTESIAN_POINT ( 'NONE',  ( 0.2863795044656264888, -1.560883083107998059, 0.9807757954863742800 ) ) ;
#12772 = AXIS2_PLACEMENT_3D ( 'NONE', #39885, #5914, #24459 ) ;
#12773 = AXIS2_PLACEMENT_3D ( 'NONE', #1140, #23724, #4176 ) ;
#12774 = LINE ( 'NONE', #34769, #18580 ) ;
#12775 = CARTESIAN_POINT ( 'NONE',  ( -0.1669433606228570843, 0.5138636982738132852, 0.3750000000000001110 ) ) ;
#12776 = AXIS2_PLACEMENT_3D ( 'NONE', #8131, #1585, #11222 ) ;
#12777 = DIRECTION ( 'NONE',  ( 1.000000000000000000, 0.000000000000000000, 0.000000000000000000 ) ) ;
#12778 = FACE_OUTER_BOUND ( 'NONE', #11372, .T. ) ;
#12779 = DIRECTION ( 'NONE',  ( 0.8660512985181133550, 0.4999551463232373427, 1.217559039701221479E-16 ) ) ;
#12780 = AXIS2_PLACEMENT_3D ( 'NONE', #6392, #15861, #19962 ) ;
#12781 = FACE_OUTER_BOUND ( 'NONE', #5727, .T. ) ;
#12782 = CARTESIAN_POINT ( 'NONE',  ( -0.02000000000000000042, -1.712002775963388235, -0.1631032362481502906 ) ) ;
#12783 = AXIS2_PLACEMENT_3D ( 'NONE', #8206, #23866, #1858 ) ;
#12784 = CARTESIAN_POINT ( 'NONE',  ( 0.2829942045735191480, -1.550042413449979062, -0.6886752251949420645 ) ) ;
#12785 = PERSON_AND_ORGANIZATION ( #28500, #32463 ) ;
#12786 = AXIS2_PLACEMENT_3D ( 'NONE', #1913, #2097, #29472 ) ;
#12787 = ADVANCED_FACE ( 'NONE', ( #17642 ), #17323, .F. ) ;
#12788 = CARTESIAN_POINT ( 'NONE',  ( -0.05279905671745363516, 0.4561941007107723212, 0.1063003320160429144 ) ) ;
#12789 = DIRECTION ( 'NONE',  ( 7.771561172376107616E-16, -7.170354002788761615E-17, 1.000000000000000000 ) ) ;
#12790 = ADVANCED_FACE ( 'NONE', ( #39441 ), #35754, .F. ) ;
#12791 = ORIENTED_EDGE ( 'NONE', *, *, #35182, .F. ) ;
#12792 = CARTESIAN_POINT ( 'NONE',  ( 0.1973196604133208854, -0.5903291263510783704, 0.3099102803838563180 ) ) ;
#12793 = EDGE_LOOP ( 'NONE', ( #32532, #4561, #27687, #33683 ) ) ;
#12794 = LINE ( 'NONE', #28637, #38804 ) ;
#12795 = CARTESIAN_POINT ( 'NONE',  ( 0.2025468388808826514, -1.402172900482729911, 0.9469506584777290792 ) ) ;
#12796 = AXIS2_PLACEMENT_3D ( 'NONE', #21624, #24911, #5957 ) ;
#12797 = CARTESIAN_POINT ( 'NONE',  ( 0.1313385724593379156, -0.5561286514583599905, 0.1878675228657155638 ) ) ;
#12799 = VERTEX_POINT ( 'NONE', #20142 ) ;
#12798 = DIRECTION ( 'NONE',  ( 0.01455087615875007116, 0.9998941303973200023, 0.000000000000000000 ) ) ;
#12800 = AXIS2_PLACEMENT_3D ( 'NONE', #1773, #7701, #33209 ) ;
#12802 = VERTEX_POINT ( 'NONE', #17040 ) ;
#12801 = ORIENTED_EDGE ( 'NONE', *, *, #34263, .T. ) ;
#12803 = DIRECTION ( 'NONE',  ( -1.000000000000000000, 0.000000000000000000, 0.000000000000000000 ) ) ;
#12804 = AXIS2_PLACEMENT_3D ( 'NONE', #9791, #38376, #3627 ) ;
#12805 = ORIENTED_EDGE ( 'NONE', *, *, #37119, .T. ) ;
#12806 = TOROIDAL_SURFACE ( 'NONE', #9511, 0.1333070866141734256, 0.02999999999999999889 ) ;
#12807 = APPLIED_SECURITY_CLASSIFICATION_ASSIGNMENT ( #25296, ( #22018 ) ) ;
#12808 = CARTESIAN_POINT ( 'NONE',  ( 0.6358220093450094312, -1.612209227696623115, -0.5779622822862300335 ) ) ;
#12809 = EDGE_CURVE ( 'NONE', #37238, #24651, #38984, .T. ) ;
#12810 = ITEM_DEFINED_TRANSFORMATION ( 'NONE', 'NONE', #24629,  #27819 ) ;
#12811 = APPLIED_PERSON_AND_ORGANIZATION_ASSIGNMENT ( #19597, #1106, ( #31348 ) ) ;
#12812 = CARTESIAN_POINT ( 'NONE',  ( -0.02000000000000000042, -1.727585455013649351, 0.002733164971117934498 ) ) ;
#12813 = B_SPLINE_CURVE_WITH_KNOTS ( 'NONE', 3,
 ( #22125, #2370, #8935, #40408 ),
 .UNSPECIFIED., .F., .F.,
 ( 4, 4 ),
 ( 0.000000000000000000, 0.001713671539103278673 ),
 .UNSPECIFIED. ) ;
#12814 = ORIENTED_EDGE ( 'NONE', *, *, #22553, .T. ) ;
#12815 = EDGE_CURVE ( 'NONE', #2281, #24994, #30095, .T. ) ;
#12816 = CARTESIAN_POINT ( 'NONE',  ( 0.08538299691383845202, -0.7671892257780283941, 0.1589107908280385228 ) ) ;
#12817 = VECTOR ( 'NONE', #28562, 39.37007874015748143 ) ;
#12818 = CARTESIAN_POINT ( 'NONE',  ( 0.1052052648158661730, -0.5678973627517217571, 0.2443419843495847621 ) ) ;
#12819 = DIRECTION ( 'NONE',  ( 1.000000000000000000, 1.113825344428167933E-31, -7.771561172376107616E-16 ) ) ;
#12820 = CARTESIAN_POINT ( 'NONE',  ( -0.1707856549140137903, 0.4978063840003604246, 0.1437995925080443882 ) ) ;
#12821 = ORIENTED_EDGE ( 'NONE', *, *, #28653, .T. ) ;
#12822 = CARTESIAN_POINT ( 'NONE',  ( 0.4068922648389373120, -1.709694718896766163, 0.6105211896656776993 ) ) ;
#12823 = CARTESIAN_POINT ( 'NONE',  ( 0.7282435738944056380, -1.482681635168590084, 0.7278836751128088256 ) ) ;
#12824 = EDGE_LOOP ( 'NONE', ( #8847, #27449, #32714, #910, #20969, #25707, #34443, #36055, #10847, #13753, #11555, #29488, #11593, #39103, #28636, #40277, #15211, #38787, #24677, #18969, #18654, #39271, #21658, #23682, #18694, #1258, #11497 ) ) ;
#12825 = CARTESIAN_POINT ( 'NONE',  ( 0.01548846960707582834, 0.4638115001430508921, 0.2459753896938730033 ) ) ;
#12826 = CARTESIAN_POINT ( 'NONE',  ( 0.6087833944362014416, -1.478973828311692884, 0.5678978172759817644 ) ) ;
#12827 = CARTESIAN_POINT ( 'NONE',  ( 0.04293317454820586021, -0.4876093284570336417, 0.08292018301452548645 ) ) ;
#12828 = CIRCLE ( 'NONE', #33852, 0.01499999999999998036 ) ;
#12829 = CARTESIAN_POINT ( 'NONE',  ( 0.1434010736994648927, -1.283284918233685623, 0.5707417262808780478 ) ) ;
#12830 = CIRCLE ( 'NONE', #22046, 0.07999999999999996003 ) ;
#12831 = CARTESIAN_POINT ( 'NONE',  ( 0.4686710939017081357, -1.131369304810952325, -0.3726880373738259977 ) ) ;
#12832 = CARTESIAN_POINT ( 'NONE',  ( 0.05447883519600660307, -1.297772118441766542, 0.6273051521731305424 ) ) ;
#12833 = CARTESIAN_POINT ( 'NONE',  ( 0.3071794164948500327, -0.9095699098325729093, 0.5987596725107463547 ) ) ;
#12834 = PERSON_AND_ORGANIZATION ( #28500, #32463 ) ;
#12835 = DIRECTION ( 'NONE',  ( -1.000000000000000000, 0.000000000000000000, 0.000000000000000000 ) ) ;
#12836 = LOCAL_TIME ( 0, 53, 7.000000000000000000, #35031 ) ;
#12837 = EDGE_CURVE ( 'NONE', #31681, #23240, #4813, .T. ) ;
#12838 = EDGE_CURVE ( 'NONE', #23955, #1103, #31159, .T. ) ;
#12839 = CARTESIAN_POINT ( 'NONE',  ( 0.5845432865795784361, -1.492259592395753121, 0.5476657707439447353 ) ) ;
#12840 = CARTESIAN_POINT ( 'NONE',  ( -0.04285561529640979223, 0.07198636226547958095, 0.4895514295879622169 ) ) ;
#12841 = ORIENTED_EDGE ( 'NONE', *, *, #20060, .T. ) ;
#12842 = CARTESIAN_POINT ( 'NONE',  ( 0.4200748011392089198, -1.654004974025707897, -0.7462941026102624109 ) ) ;
#12843 = DIRECTION ( 'NONE',  ( 0.000000000000000000, 0.000000000000000000, -1.000000000000000000 ) ) ;
#12844 = CARTESIAN_POINT ( 'NONE',  ( 0.08906878592800504535, -0.5893343340316107293, 0.07116080034756296080 ) ) ;
#12845 = ORIENTED_EDGE ( 'NONE', *, *, #39807, .T. ) ;
#12846 = CARTESIAN_POINT ( 'NONE',  ( 0.4092450614235220163, -1.131740385117829817, 0.4687417262808780127 ) ) ;
#12847 = CARTESIAN_POINT ( 'NONE',  ( -0.01502126383153619404, -0.8492948373293993658, 0.1457185332388695187 ) ) ;
#12849 = ORIENTED_EDGE ( 'NONE', *, *, #27890, .F. ) ;
#12848 = ORIENTED_EDGE ( 'NONE', *, *, #21002, .T. ) ;
#12850 = DIRECTION ( 'NONE',  ( -1.000000000000000000, -0.000000000000000000, -0.000000000000000000 ) ) ;
#12851 = CARTESIAN_POINT ( 'NONE',  ( -0.02000000000000000042, -1.598492537578166672, -0.1971380022280825872 ) ) ;
#12852 = CARTESIAN_POINT ( 'NONE',  ( 0.4218037824360915677, -1.666477969087174493, -0.5029009060039884016 ) ) ;
#12854 = DIRECTION ( 'NONE',  ( 0.000000000000000000, 0.000000000000000000, 1.000000000000000000 ) ) ;
#12853 = CARTESIAN_POINT ( 'NONE',  ( 0.04575334816097070129, 0.4390433668671658296, 0.2110480141057521908 ) ) ;
#12855 = VECTOR ( 'NONE', #13301, 39.37007874015748854 ) ;
#12856 = CARTESIAN_POINT ( 'NONE',  ( 0.03672447062657707012, -0.3146083306767501475, -0.3636032511890223695 ) ) ;
#12857 = EDGE_LOOP ( 'NONE', ( #28123, #6366, #2450, #39005 ) ) ;
#12858 = CARTESIAN_POINT ( 'NONE',  ( 0.01048552245699511248, -0.5296434293125212855, 0.1353013932409117825 ) ) ;
#12859 = CIRCLE ( 'NONE', #437, 0.01500000000000004975 ) ;
#12860 = VERTEX_POINT ( 'NONE', #39858 ) ;
#12861 = ORIENTED_EDGE ( 'NONE', *, *, #14962, .F. ) ;
#12862 = CARTESIAN_POINT ( 'NONE',  ( 0.1074308231225710453, -0.6537910774608231002, 0.3828935582149098904 ) ) ;
#12863 = EDGE_LOOP ( 'NONE', ( #30292, #17610, #37070, #28176 ) ) ;
#12864 = ORIENTED_EDGE ( 'NONE', *, *, #24109, .F. ) ;
#12865 = PLANE ( 'NONE',  #26615 ) ;
#12866 = CARTESIAN_POINT ( 'NONE',  ( 0.4416260615216031638, -1.573751756256522860, 0.5728199209250995905 ) ) ;
#12868 = CARTESIAN_POINT ( 'NONE',  ( -0.1044436713285736007, -0.4741860147766045475, 0.3472338286680813901 ) ) ;
#12867 = CARTESIAN_POINT ( 'NONE',  ( 0.002594981386083806962, -0.5384102241734924910, 0.2402617689866153317 ) ) ;
#12869 = DIRECTION ( 'NONE',  ( 0.000000000000000000, 3.885780586188049371E-16, 1.000000000000000000 ) ) ;
#12870 = CARTESIAN_POINT ( 'NONE',  ( 0.4073273336764455244, -1.035739235929862723, 0.6333991914734626860 ) ) ;
#12871 = CARTESIAN_POINT ( 'NONE',  ( 0.3711011835697567429, -1.742358524620057914, 0.6021863986438362737 ) ) ;
#12872 = VERTEX_POINT ( 'NONE', #36757 ) ;
#12873 = EDGE_CURVE ( 'NONE', #20339, #27374, #19327, .T. ) ;
#12874 = FACE_OUTER_BOUND ( 'NONE', #29843, .T. ) ;
#12875 = CARTESIAN_POINT ( 'NONE',  ( 0.1887425661959986067, -0.4595475489851841844, 0.1484827297904532939 ) ) ;
#12876 = CARTESIAN_POINT ( 'NONE',  ( 0.1257895988989382596, -0.5688825542510129729, 0.2354356649681056124 ) ) ;
#12877 = CARTESIAN_POINT ( 'NONE',  ( -0.03874953289575409909, 0.3062954455724236635, -0.3649061716334326411 ) ) ;
#12878 = DIRECTION ( 'NONE',  ( -0.8660512985181135770, -0.4999551463232371207, 0.000000000000000000 ) ) ;
#12879 = DIRECTION ( 'NONE',  ( -7.771561172376107616E-16, 7.170354002788761615E-17, -1.000000000000000000 ) ) ;
#12880 = CARTESIAN_POINT ( 'NONE',  ( 0.5546478408217279110, -1.425212702037291113, 0.7586032485602538511 ) ) ;
#12881 = CARTESIAN_POINT ( 'NONE',  ( 0.3047936848243344432, -1.756875962071034580, 0.5682417262361116883 ) ) ;
#12882 = CARTESIAN_POINT ( 'NONE',  ( 0.2196261443710258443, -0.6607888217372858142, 0.4354189310569229754 ) ) ;
#12883 = DIRECTION ( 'NONE',  ( -1.000000000000000000, -0.000000000000000000, -0.000000000000000000 ) ) ;
#12884 = CARTESIAN_POINT ( 'NONE',  ( 0.06285925416399532062, -1.277715309600261806, 0.6373717965182834622 ) ) ;
#12885 = B_SPLINE_CURVE_WITH_KNOTS ( 'NONE', 3,
 ( #26207, #23342, #38730, #14441, #39156, #8069, #20644, #35656 ),
 .UNSPECIFIED., .F., .F.,
 ( 4, 2, 2, 4 ),
 ( 3.469446951953614189E-18, 0.0002979885802634740506, 0.0005959771605269446318, 0.001191954321053884710 ),
 .UNSPECIFIED. ) ;
#12886 = DIRECTION ( 'NONE',  ( -1.000000000000000000, -1.448788479720435680E-15, 8.315531510821436104E-16 ) ) ;
#12887 = AXIS2_PLACEMENT_3D ( 'NONE', #4553, #29670, #23114 ) ;
#12888 = DIRECTION ( 'NONE',  ( 0.000000000000000000, 0.000000000000000000, -1.000000000000000000 ) ) ;
#12889 = CARTESIAN_POINT ( 'NONE',  ( 0.1465276397530375918, -0.8893464018661847437, 0.5571063954901773752 ) ) ;
#12890 = CARTESIAN_POINT ( 'NONE',  ( 0.1809966328114128720, -1.222385076516254054, -0.5155029497116575543 ) ) ;
#12891 = CARTESIAN_POINT ( 'NONE',  ( 0.6528116166078939964, -1.560548874428574262, 0.4255554162163330822 ) ) ;
#12892 = APPLIED_APPROVAL_ASSIGNMENT ( #32756, ( #25389 ) ) ;
#12893 = ORIENTED_EDGE ( 'NONE', *, *, #1664, .T. ) ;
#12894 = FACE_BOUND ( 'NONE', #38850, .T. ) ;
#12895 = CARTESIAN_POINT ( 'NONE',  ( 0.3638636590137022120, -1.622755819691197754, -0.3680121727053636826 ) ) ;
#12896 = CARTESIAN_POINT ( 'NONE',  ( 0.3675394818443805112, -2.037853795900605114, -0.4718837028662131172 ) ) ;
#12897 = LINE ( 'NONE', #28524, #35588 ) ;
#12898 = DIRECTION ( 'NONE',  ( 1.000000000000000000, 0.000000000000000000, 0.000000000000000000 ) ) ;
#12899 = AXIS2_PLACEMENT_3D ( 'NONE', #35252, #22720, #22509 ) ;
#12900 = ORIENTED_EDGE ( 'NONE', *, *, #21821, .F. ) ;
#12901 = DIRECTION ( 'NONE',  ( 4.503376743791639448E-15, 0.9613939893712163398, -0.2751755752258865373 ) ) ;
#12902 = CARTESIAN_POINT ( 'NONE',  ( 0.2230281810701175149, -1.353330874913282855, 0.5685393872860169395 ) ) ;
#12903 = CARTESIAN_POINT ( 'NONE',  ( -0.08000000000000000167, -2.039246558356380135, -0.5681570558249129377 ) ) ;
#12904 = CARTESIAN_POINT ( 'NONE',  ( -0.01548846960707524721, 0.3772621329472709006, 0.3651003739303413931 ) ) ;
#12905 = CARTESIAN_POINT ( 'NONE',  ( 0.3779407171956395972, -1.119494477781395103, 0.7341046588790626215 ) ) ;
#12907 = DIRECTION ( 'NONE',  ( 0.4999999999999981681, 0.7918451760093985214, 0.3506867793781887621 ) ) ;
#12906 = CARTESIAN_POINT ( 'NONE',  ( -0.2399999999999999079, -3.220869926774937664, -0.5656276768926112863 ) ) ;
#12908 = CARTESIAN_POINT ( 'NONE',  ( 0.4929039159923706559, -1.082692164550193237, 0.5711674032880966756 ) ) ;
#12909 = VERTEX_POINT ( 'NONE', #40250 ) ;
#12910 = PERSON_AND_ORGANIZATION ( #29446, #29988 ) ;
#12911 = CARTESIAN_POINT ( 'NONE',  ( 0.000000000000000000, -0.02999999999999995379, 0.000000000000000000 ) ) ;
#12912 = ORIENTED_EDGE ( 'NONE', *, *, #138, .T. ) ;
#12913 = CARTESIAN_POINT ( 'NONE',  ( 0.3881114196206040812, -1.604032130030556447, 0.6335681399033196159 ) ) ;
#12915 = CARTESIAN_POINT ( 'NONE',  ( 0.1746425353517715717, -0.9069533527181683485, 0.07551361239408968529 ) ) ;
#12914 = CARTESIAN_POINT ( 'NONE',  ( 0.08535229771277842714, -0.8275964096657028035, 0.1106497307489484189 ) ) ;
#12916 = CARTESIAN_POINT ( 'NONE',  ( 0.08510361377861434817, -0.8106636051554854117, 0.1454306519311501233 ) ) ;
#12917 = ORIENTED_EDGE ( 'NONE', *, *, #26536, .F. ) ;
#12918 = VERTEX_POINT ( 'NONE', #12474 ) ;
#12919 = CONICAL_SURFACE ( 'NONE', #8939, 0.1600000000000015854, 1.047197551196600296 ) ;
#12920 = CARTESIAN_POINT ( 'NONE',  ( 0.4913580909694157950, -1.080994014340969311, 0.5908918996469622043 ) ) ;
#12921 = ADVANCED_FACE ( 'NONE', ( #31416 ), #21142, .T. ) ;
#12922 = EDGE_CURVE ( 'NONE', #17955, #13190, #33762, .T. ) ;
#12923 = CARTESIAN_POINT ( 'NONE',  ( 0.5673951979382229061, -1.499929312403656123, 0.6329649192270386804 ) ) ;
#12924 = EDGE_LOOP ( 'NONE', ( #25576, #18892, #27737 ) ) ;
#12925 = CARTESIAN_POINT ( 'NONE',  ( 0.5546656019160204343, -1.624250834075737560, -0.4654251787435473298 ) ) ;
#12926 = CARTESIAN_POINT ( 'NONE',  ( 0.1981231351721541856, -1.245830158587560410, -0.3144976166544465324 ) ) ;
#12927 = EDGE_CURVE ( 'NONE', #20390, #27640, #30800, .T. ) ;
#12928 = CARTESIAN_POINT ( 'NONE',  ( 0.05999999999999990757, 0.4357424459509064985, 0.2678820090948821342 ) ) ;
#12929 = SECURITY_CLASSIFICATION ( '', '', #37436 ) ;
#12930 = CARTESIAN_POINT ( 'NONE',  ( 0.3702591405535748947, -1.654865263428320077, -0.7284099060135055259 ) ) ;
#12931 = ORIENTED_EDGE ( 'NONE', *, *, #22847, .T. ) ;
#12932 = ADVANCED_FACE ( 'NONE', ( #21359 ), #21410, .F. ) ;
#12933 = CARTESIAN_POINT ( 'NONE',  ( -0.2399999999999999079, -1.835749455202394298, -0.3938319975228649072 ) ) ;
#12934 = DIRECTION ( 'NONE',  ( -2.563099466555618426E-12, 0.9510565162951575280, 0.3090169943749354053 ) ) ;
#12935 = EDGE_CURVE ( 'NONE', #10115, #17094, #40337, .T. ) ;
#12936 = AXIS2_PLACEMENT_3D ( 'NONE', #15130, #14737, #33446 ) ;
#12937 = CARTESIAN_POINT ( 'NONE',  ( 0.6872158423035881203, -1.414036026188038031, 0.8114895833460221697 ) ) ;
#12938 = CARTESIAN_POINT ( 'NONE',  ( 0.3997069619151109032, -2.078179102625506314, -0.5163588566289569748 ) ) ;
#12939 = CARTESIAN_POINT ( 'NONE',  ( 0.01548846960707292615, 0.09061086148586355860, -0.5171215251570915328 ) ) ;
#12940 = CARTESIAN_POINT ( 'NONE',  ( -0.2300000000000005651, 0.5182417262804733804, 0.08500000000000004774 ) ) ;
#12941 = CARTESIAN_POINT ( 'NONE',  ( 0.1909286924077254199, -1.257064795538238577, -0.7137147910238503812 ) ) ;
#12942 = COORDINATED_UNIVERSAL_TIME_OFFSET ( 0, 0, .AHEAD. ) ;
#12943 = CARTESIAN_POINT ( 'NONE',  ( 0.4579382962256918765, -1.063507731091402952, 0.6287285752299462960 ) ) ;
#12944 = DIRECTION ( 'NONE',  ( -7.000205099780314469E-17, -1.000000000000000000, 6.590151126658399604E-16 ) ) ;
#12945 = CARTESIAN_POINT ( 'NONE',  ( 0.2637479789745994507, -0.6009450727723176788, 0.1023043458361303365 ) ) ;
#12946 = CARTESIAN_POINT ( 'NONE',  ( 0.2638409115276085237, -1.685919794262354499, 0.5661884833608360479 ) ) ;
#12947 = EDGE_CURVE ( 'NONE', #14789, #30962, #3037, .T. ) ;
#12948 = APPLIED_PERSON_AND_ORGANIZATION_ASSIGNMENT ( #35346, #818, ( #10846 ) ) ;
#12949 = CARTESIAN_POINT ( 'NONE',  ( 0.1209218709639075517, -1.413449759333152755, 0.6688053819537839173 ) ) ;
#12950 = CARTESIAN_POINT ( 'NONE',  ( 0.6040377325928559804, -1.527126331885624522, -0.4341809412190014705 ) ) ;
#12951 = CARTESIAN_POINT ( 'NONE',  ( 0.2079683456743255388, -1.627305492656140551, -0.6921328867639651161 ) ) ;
#12952 = AXIS2_PLACEMENT_3D ( 'NONE', #3411, #15967, #28119 ) ;
#12953 = CARTESIAN_POINT ( 'NONE',  ( -0.02000000000000000042, -1.669835911085076674, -0.2333336242928227000 ) ) ;
#12954 = ORIENTED_EDGE ( 'NONE', *, *, #24940, .T. ) ;
#12955 = CIRCLE ( 'NONE', #6357, 0.1000000000000000194 ) ;
#12956 = EDGE_LOOP ( 'NONE', ( #29507, #30118, #9347, #35411 ) ) ;
#12957 = LINE ( 'NONE', #37624, #9204 ) ;
#12958 = VERTEX_POINT ( 'NONE', #15766 ) ;
#12959 = CARTESIAN_POINT ( 'NONE',  ( 0.3593346688482154661, -1.735925422213635549, -0.5010936962835144115 ) ) ;
#12960 = CARTESIAN_POINT ( 'NONE',  ( 0.03159140494780116742, 0.3316214887069901529, 0.3635694333040935811 ) ) ;
#12961 = CARTESIAN_POINT ( 'NONE',  ( 0.5692153087590623439, -1.410103658342158894, 0.7339724487708582101 ) ) ;
#12963 = ORIENTED_EDGE ( 'NONE', *, *, #5739, .T. ) ;
#12962 = CARTESIAN_POINT ( 'NONE',  ( 0.5988734330629296165, -1.608409508104120089, 0.4438041697090711057 ) ) ;
#12964 = VERTEX_POINT ( 'NONE', #595 ) ;
#12965 = CARTESIAN_POINT ( 'NONE',  ( 0.5593576702765247211, -1.619265888493739869, 0.4800288912735870550 ) ) ;
#12966 = ORIENTED_EDGE ( 'NONE', *, *, #23876, .T. ) ;
#12967 = CARTESIAN_POINT ( 'NONE',  ( 0.01188774847410361928, -0.5569381300819099545, 0.2634111891979500353 ) ) ;
#12969 = LINE ( 'NONE', #37857, #39262 ) ;
#12968 = CARTESIAN_POINT ( 'NONE',  ( 0.5389700850957479528, -1.668120024254199141, -0.4887752422164399757 ) ) ;
#12970 = CARTESIAN_POINT ( 'NONE',  ( 0.3116392842230086835, -1.763036623927715763, 0.5305946302528526948 ) ) ;
#12971 = CARTESIAN_POINT ( 'NONE',  ( 0.3946727801157763893, -1.754662960969486818, -0.5213263030586290370 ) ) ;
#12972 = CARTESIAN_POINT ( 'NONE',  ( 0.4125049716505733155, -1.702587279938547082, 0.4182417262808258984 ) ) ;
#12974 = ORIENTED_EDGE ( 'NONE', *, *, #11715, .F. ) ;
#12973 = VERTEX_POINT ( 'NONE', #16581 ) ;
#12975 = DIRECTION ( 'NONE',  ( 0.4999551463232373427, -0.8660512985181134660, 0.000000000000000000 ) ) ;
#12976 = CARTESIAN_POINT ( 'NONE',  ( 0.2120302040687593315, -0.9292546879809068239, 0.3755713860025718942 ) ) ;
#12977 = CARTESIAN_POINT ( 'NONE',  ( -0.04047161733260044858, -0.4536038223829735871, 0.2133268955647525666 ) ) ;
#12978 = ADVANCED_FACE ( 'NONE', ( #25454 ), #38585, .T. ) ;
#12979 = CARTESIAN_POINT ( 'NONE',  ( 0.5744677579470482964, -1.463377169234544084, 0.7112240420332721635 ) ) ;
#12980 = CARTESIAN_POINT ( 'NONE',  ( 0.3215791306822571305, -1.068485763701718438, 0.7392398419832824086 ) ) ;
#12981 = DIRECTION ( 'NONE',  ( 0.000000000000000000, 0.000000000000000000, 1.000000000000000000 ) ) ;
#12982 = EDGE_CURVE ( 'NONE', #243, #34712, #20790, .T. ) ;
#12983 = DIRECTION ( 'NONE',  ( 1.000000000000000000, 2.280301054154495132E-31, -1.664003471950577689E-31 ) ) ;
#12984 = EDGE_CURVE ( 'NONE', #29116, #25808, #12678, .T. ) ;
#12985 = APPLICATION_CONTEXT ( 'configuration controlled 3d designs of mechanical parts and assemblies' ) ;
#12986 = CARTESIAN_POINT ( 'NONE',  ( 1.024442997624098658E-15, -0.3059742766594579222, -1.570812596356951301E-15 ) ) ;
#12987 = CARTESIAN_POINT ( 'NONE',  ( 0.3251018894956911320, -1.768268453779731519, 0.5225951996439848202 ) ) ;
#12988 =( BOUNDED_SURFACE ( )  B_SPLINE_SURFACE ( 3, 2, ( 
 ( #13151, #39070, #7170 ),
 ( #19944, #38247, #13365 ),
 ( #16264, #38657, #26142 ),
 ( #6985, #20164, #16657 ),
 ( #25715, #28991, #38462 ),
 ( #32271, #10895, #22651 ),
 ( #29411, #10476, #1447 ),
 ( #23468, #13759, #6773 ),
 ( #19352, #7369, #35568 ),
 ( #29206, #35183, #19557 ),
 ( #32479, #32087, #13960 ),
 ( #31890, #10678, #10077 ),
 ( #7588, #22861, #3894 ),
 ( #16450, #4304, #1257 ),
 ( #35380, #856, #26325 ),
 ( #10297, #16870, #38849 ),
 ( #23253, #3709, #35778 ),
 ( #32691, #4089, #28801 ),
 ( #1067, #4496, #17059 ),
 ( #29604, #18224, #4689 ),
 ( #20358, #3005, #33294 ),
 ( #26741, #18631, #2794 ),
 ( #39462, #34056, #8198 ),
 ( #12055, #15342, #7789 ) ),
 .UNSPECIFIED., .F., .F., .T. ) 
 B_SPLINE_SURFACE_WITH_KNOTS ( ( 4, 2, 2, 2, 2, 2, 2, 2, 2, 2, 2, 4 ),
 ( 3, 3 ),
 ( 0.005360940551000458604, 0.008137707959848014538, 0.01091447536869557221, 0.01369124277754312988, 0.01646801018639068581, 0.01924477759523824175, 0.02202154500408579768, 0.02340992870850957391, 0.02479831241293335362, 0.02549250426514524520, 0.02618669611735713332, 0.02757507982178090955 ),
 ( 0.000000000000000000, 1.000000000000000000 ),
 .UNSPECIFIED. ) 
 GEOMETRIC_REPRESENTATION_ITEM ( )  RATIONAL_B_SPLINE_SURFACE ( (
 ( 1.000000000000000000, 0.7071328584466060052, 1.000000000000000000),
 ( 1.000000000000000000, 0.7072620464649821415, 1.000000000000000000),
 ( 1.000000000000000000, 0.7085185872330661550, 1.000000000000000000),
 ( 1.000000000000000000, 0.7116993494293128997, 1.000000000000000000),
 ( 1.000000000000000000, 0.7136510046383820471, 1.000000000000000000),
 ( 1.000000000000000000, 0.7179400475017202465, 1.000000000000000000),
 ( 1.000000000000000000, 0.7202921658712200248, 1.000000000000000000),
 ( 1.000000000000000000, 0.7253987115934981134, 1.000000000000000000),
 ( 1.000000000000000000, 0.7281595695102663912, 1.000000000000000000),
 ( 1.000000000000000000, 0.7341325496256051464, 1.000000000000000000),
 ( 1.000000000000000000, 0.7373714411113219125, 1.000000000000000000),
 ( 1.000000000000000000, 0.7439769103193287769, 1.000000000000000000),
 ( 1.000000000000000000, 0.7474422512830740661, 1.000000000000000000),
 ( 1.000000000000000000, 0.7514310957412383418, 1.000000000000000000),
 ( 1.000000000000000000, 0.7525427382793115072, 1.000000000000000000),
 ( 1.000000000000000000, 0.7534397546842908078, 1.000000000000000000),
 ( 1.000000000000000000, 0.7532682500171895557, 1.000000000000000000),
 ( 1.000000000000000000, 0.7505746427157311551, 1.000000000000000000),
 ( 1.000000000000000000, 0.7492519672572479639, 1.000000000000000000),
 ( 1.000000000000000000, 0.7453945544990168148, 1.000000000000000000),
 ( 1.000000000000000000, 0.7428563216680332815, 1.000000000000000000),
 ( 1.000000000000000000, 0.7326522287684954504, 1.000000000000000000),
 ( 1.000000000000000000, 0.7220899002612864992, 1.000000000000000000),
 ( 1.000000000000000000, 0.7071496063340624305, 1.000000000000000000) ) ) 
 REPRESENTATION_ITEM ( '' )  SURFACE ( )  );
#12989 = CARTESIAN_POINT ( 'NONE',  ( 0.4553705988804589988, -1.219712494940672132, 0.6659395549564459671 ) ) ;
#12990 = CARTESIAN_POINT ( 'NONE',  ( 0.3968784764610951976, -1.684996356591544231, -0.4053910425699968068 ) ) ;
#12991 = SHAPE_REPRESENTATION_RELATIONSHIP ( 'NONE' , 'NONE' ,  #35919, #37306 ) ;
#12992 = CARTESIAN_POINT ( 'NONE',  ( -0.0004431470427073231017, -0.9367128829938298207, 0.1457185332388704069 ) ) ;
#12993 = DIRECTION ( 'NONE',  ( -1.000000000000000000, 0.000000000000000000, -5.691349986800505477E-16 ) ) ;
#12994 = CARTESIAN_POINT ( 'NONE',  ( 0.1143055500903454591, -1.383430755858714445, 0.6590833788586937247 ) ) ;
#12995 = DATE_TIME_ROLE ( 'classification_date' ) ;
#12996 = EDGE_CURVE ( 'NONE', #23581, #16603, #17342, .T. ) ;
#12997 = CARTESIAN_POINT ( 'NONE',  ( 0.3718881020994557751, -1.717634997487592630, -0.6861734131539279913 ) ) ;
#12998 = CARTESIAN_POINT ( 'NONE',  ( -0.04308611741967801473, 0.4845711164928901971, 0.09763251765261002357 ) ) ;
#12999 = B_SPLINE_CURVE_WITH_KNOTS ( 'NONE', 3,
 ( #5697, #11264, #40248, #29996 ),
 .UNSPECIFIED., .F., .F.,
 ( 4, 4 ),
 ( 0.000000000000000000, 0.002406601043976852941 ),
 .UNSPECIFIED. ) ;
#13000 = ORIENTED_EDGE ( 'NONE', *, *, #29019, .T. ) ;
#13001 = CARTESIAN_POINT ( 'NONE',  ( 0.4239279940938358027, -1.134057330594810509, 0.4357807031462634928 ) ) ;
#13002 = EDGE_LOOP ( 'NONE', ( #16299, #39353, #18073, #28225 ) ) ;
#13003 = DIRECTION ( 'NONE',  ( 1.060606950627616897E-16, 6.122684696619992497E-17, 1.000000000000000000 ) ) ;
#13004 = CARTESIAN_POINT ( 'NONE',  ( 0.2648844005684549696, -1.672583955634053599, 0.5258809023128611093 ) ) ;
#13005 = CARTESIAN_POINT ( 'NONE',  ( 0.1316748077902114011, -0.5679410235953537001, 0.2289183786684796940 ) ) ;
#13007 = ORIENTED_EDGE ( 'NONE', *, *, #13158, .T. ) ;
#13006 = CARTESIAN_POINT ( 'NONE',  ( 0.5089656749515859557, -1.649654440091849139, -0.4396827738775478944 ) ) ;
#13009 = VERTEX_POINT ( 'NONE', #9601 ) ;
#13008 = VERTEX_POINT ( 'NONE', #26067 ) ;
#13010 = CARTESIAN_POINT ( 'NONE',  ( 0.6408424734368098896, -1.484124584333256447, 0.7996275517132238608 ) ) ;
#13011 = VERTEX_POINT ( 'NONE', #3218 ) ;
#13012 = CARTESIAN_POINT ( 'NONE',  ( 0.6147040457557710891, -1.612300127778828251, -0.5493327930725481201 ) ) ;
#13013 = APPROVAL_DATE_TIME ( #3323, #30647 ) ;
#13014 = CARTESIAN_POINT ( 'NONE',  ( -0.3000000000000000999, -3.609310082097819894, -0.4498340178114252352 ) ) ;
#13015 = VERTEX_POINT ( 'NONE', #34889 ) ;
#13016 = CARTESIAN_POINT ( 'NONE',  ( 0.08709445727914670587, -0.7690269056237728496, 0.2131905848466921494 ) ) ;
#13017 = CIRCLE ( 'NONE', #40603, 0.1620173459747806799 ) ;
#13018 = ADVANCED_FACE ( 'NONE', ( #22178 ), #29836, .F. ) ;
#13019 = CARTESIAN_POINT ( 'NONE',  ( 0.08990936761270149069, -0.5436479961250832993, 0.1437216542238700934 ) ) ;
#13020 = CARTESIAN_POINT ( 'NONE',  ( 0.5390789672074006722, -1.519044896617570473, 0.5730556844385706894 ) ) ;
#13021 = DIRECTION ( 'NONE',  ( 0.000000000000000000, 0.000000000000000000, -1.000000000000000000 ) ) ;
#13022 = CARTESIAN_POINT ( 'NONE',  ( -0.1673869564144415956, 0.4868872877193617943, 0.1265580611896311158 ) ) ;
#13023 = CARTESIAN_POINT ( 'NONE',  ( -0.1684323895664708859, 0.5231977504175450155, 0.1471384328909202122 ) ) ;
#13024 = ORIENTED_EDGE ( 'NONE', *, *, #29537, .T. ) ;
#13025 = EDGE_CURVE ( 'NONE', #20653, #12637, #24727, .T. ) ;
#13026 = CARTESIAN_POINT ( 'NONE',  ( 0.2209260011871197471, -1.309027873449325918, -0.6184399470714002645 ) ) ;
#13027 = CARTESIAN_POINT ( 'NONE',  ( 0.6567493722867359107, -1.524089082616542745, 0.7420751960461151597 ) ) ;
#13028 = ORIENTED_EDGE ( 'NONE', *, *, #9641, .T. ) ;
#13029 = CARTESIAN_POINT ( 'NONE',  ( 0.4455220531189463262, -1.593574230686272131, -0.6096253356284021541 ) ) ;
#13030 = CARTESIAN_POINT ( 'NONE',  ( 0.6084588361978461313, -1.478885940474569782, 0.5610653007198931341 ) ) ;
#13031 = DIRECTION ( 'NONE',  ( -1.000000000000000000, -2.280301054154495132E-31, 1.664003471950577689E-31 ) ) ;
#13032 = CARTESIAN_POINT ( 'NONE',  ( 0.1438070510857625550, -1.283988175806205723, 0.3667417262808778111 ) ) ;
#13033 = DIRECTION ( 'NONE',  ( 1.000000000000000000, 1.188678714063518030E-15, -6.695352868347822093E-17 ) ) ;
#13034 = CARTESIAN_POINT ( 'NONE',  ( 0.07959189571600921997, -1.355556588927695927, 0.6171934786799392336 ) ) ;
#13035 = CARTESIAN_POINT ( 'NONE',  ( 0.3637128952805344095, -0.9645059733743139851, 0.6550525653421633843 ) ) ;
#13036 = COORDINATED_UNIVERSAL_TIME_OFFSET ( 0, 0, .AHEAD. ) ;
#13037 = EDGE_CURVE ( 'NONE', #16750, #1246, #15377, .T. ) ;
#13038 = B_SPLINE_CURVE_WITH_KNOTS ( 'NONE', 3,
 ( #13514, #6506, #26077, #38596, #22186, #34701 ),
 .UNSPECIFIED., .F., .F.,
 ( 4, 2, 4 ),
 ( 1.734723475976807094E-18, 0.0003588387877355910536, 0.0007176775754711803724 ),
 .UNSPECIFIED. ) ;
#13039 = EDGE_CURVE ( 'NONE', #34047, #3165, #38379, .T. ) ;
#13040 = CARTESIAN_POINT ( 'NONE',  ( 0.6931363209573969675, -1.429025764147124677, 0.5740297270470278157 ) ) ;
#13041 = CARTESIAN_POINT ( 'NONE',  ( -0.01548846960707442669, 0.07651041855119183888, 0.5222379212568223350 ) ) ;
#13042 = EDGE_LOOP ( 'NONE', ( #19647, #10419, #7920, #24483 ) ) ;
#13043 = CARTESIAN_POINT ( 'NONE',  ( 0.4326363521158365644, -1.579581225308487324, 0.5961853866131431312 ) ) ;
#13044 = CARTESIAN_POINT ( 'NONE',  ( -0.05464101615137768181, -2.367354784411275670, -0.3586747285825516718 ) ) ;
#13045 = CARTESIAN_POINT ( 'NONE',  ( -0.2399999999999999079, -2.778907721888695281, -0.2599079779360263798 ) ) ;
#13046 = ORIENTED_EDGE ( 'NONE', *, *, #22888, .F. ) ;
#13047 = CARTESIAN_POINT ( 'NONE',  ( 0.05583995664670776682, -1.335624775257321817, 0.3157417262808777658 ) ) ;
#13048 = CARTESIAN_POINT ( 'NONE',  ( 0.07107056164821387578, -1.264508437377509065, 0.7522515875062320001 ) ) ;
#13050 = ORIENTED_EDGE ( 'NONE', *, *, #31276, .T. ) ;
#13049 = ORIENTED_EDGE ( 'NONE', *, *, #23072, .F. ) ;
#13051 = DIRECTION ( 'NONE',  ( -0.8660512985181135770, -0.4999551463232368431, 0.000000000000000000 ) ) ;
#13052 = DIRECTION ( 'NONE',  ( 1.702140497302367265E-12, -0.9510565162951545304, -0.3090169943749443426 ) ) ;
#13053 = DIRECTION ( 'NONE',  ( 1.000000000000000000, -0.000000000000000000, -0.000000000000000000 ) ) ;
#13055 = DIRECTION ( 'NONE',  ( 5.551115123125673617E-17, 3.263080277421931478E-16, -1.000000000000000000 ) ) ;
#13054 = CARTESIAN_POINT ( 'NONE',  ( 0.05138886601527578590, 0.4416142869301781793, 0.1669109982970058137 ) ) ;
#13056 = FACE_OUTER_BOUND ( 'NONE', #22779, .T. ) ;
#13057 = VERTEX_POINT ( 'NONE', #4017 ) ;
#13058 = CYLINDRICAL_SURFACE ( 'NONE', #5438, 0.1762268159172277748 ) ;
#13059 = VERTEX_POINT ( 'NONE', #1187 ) ;
#13060 = CARTESIAN_POINT ( 'NONE',  ( 0.1833618000930513636, -0.7929100317814798959, 0.6245802647066135416 ) ) ;
#13061 = VERTEX_POINT ( 'NONE', #39206 ) ;
#13062 = ORIENTED_EDGE ( 'NONE', *, *, #8755, .F. ) ;
#13063 = CARTESIAN_POINT ( 'NONE',  ( 0.02241053216763305364, -0.5389090406332393002, 0.4746621284997309398 ) ) ;
#13064 = CARTESIAN_POINT ( 'NONE',  ( 0.2558668472228415869, -1.097573035806539643, 0.8345594848954058786 ) ) ;
#13065 = CARTESIAN_POINT ( 'NONE',  ( 0.5164231089728142932, -1.603420859054122349, -0.4174082106076965060 ) ) ;
#13066 = CARTESIAN_POINT ( 'NONE',  ( 0.5747203984579013492, -1.612743926285909346, -0.5166151207188712791 ) ) ;
#13067 = CARTESIAN_POINT ( 'NONE',  ( 0.4916863479492353806, -1.686802518800459616, 0.5182417262812423209 ) ) ;
#13068 = ADVANCED_FACE ( 'NONE', ( #8120 ), #28542, .T. ) ;
#13069 = CARTESIAN_POINT ( 'NONE',  ( 0.4000000000017098767, -2.081908495022728900, -0.7229603458646237657 ) ) ;
#13070 = CARTESIAN_POINT ( 'NONE',  ( 0.1153471661800104520, -0.4465907051537530426, 0.1436109887884166880 ) ) ;
#13071 = ADVANCED_FACE ( 'NONE', ( #32619 ), #20074, .T. ) ;
#13072 = CARTESIAN_POINT ( 'NONE',  ( 0.1252465029946501218, -0.5602642337835891384, 0.2083474642613161176 ) ) ;
#13073 = CARTESIAN_POINT ( 'NONE',  ( -0.03309060444528674066, 0.2303206394830028259, 0.4671006372792929073 ) ) ;
#13074 = DIRECTION ( 'NONE',  ( 1.000000000000000000, 2.341930812374887555E-31, -1.664003471950578127E-31 ) ) ;
#13075 = CARTESIAN_POINT ( 'NONE',  ( -0.2746410161513776482, -4.233163482269810096, -0.5148221395285308422 ) ) ;
#13076 = CARTESIAN_POINT ( 'NONE',  ( 0.6448460108028967186, -1.341977515531164844, 0.7437914968157772755 ) ) ;
#13077 = DIRECTION ( 'NONE',  ( 0.000000000000000000, 1.951319995474463078E-15, -1.000000000000000000 ) ) ;
#13078 = CARTESIAN_POINT ( 'NONE',  ( 0.02569018704401261968, -1.113496988582522773, 0.6482248533806770352 ) ) ;
#13079 = CARTESIAN_POINT ( 'NONE',  ( 0.04157078424165153163, 0.4522175634759060814, -0.1290209392671970434 ) ) ;
#13080 = CARTESIAN_POINT ( 'NONE',  ( 0.4795034887773614307, -1.112758664428941557, -0.4039987388423294523 ) ) ;
#13081 = B_SPLINE_CURVE_WITH_KNOTS ( 'NONE', 3,
 ( #20907, #35921, #39212, #8338, #23998, #17191, #11033, #17604 ),
 .UNSPECIFIED., .F., .F.,
 ( 4, 2, 2, 4 ),
 ( 1.734723475976807094E-18, 0.0003750355950782678746, 0.0005625533926174032485, 0.0007500711901565386766 ),
 .UNSPECIFIED. ) ;
#13082 = CARTESIAN_POINT ( 'NONE',  ( 0.3720999503424056720, -1.111552407429487133, 0.7356505582348251693 ) ) ;
#13083 = CARTESIAN_POINT ( 'NONE',  ( 0.4264202721361137760, -1.467519734074644200, -0.5166151207188711680 ) ) ;
#13084 = CARTESIAN_POINT ( 'NONE',  ( 0.6995787265782542619, -1.495850124575206275, 0.4894661681568200362 ) ) ;
#13085 = ORIENTED_EDGE ( 'NONE', *, *, #31848, .F. ) ;
#13086 = CARTESIAN_POINT ( 'NONE',  ( 0.4632309505043279430, -1.114013528690801280, 0.5645935559310804042 ) ) ;
#13087 = CARTESIAN_POINT ( 'NONE',  ( 0.3706793757908085074, -1.615012852715396408, -0.4172838525897037409 ) ) ;
#13088 = CARTESIAN_POINT ( 'NONE',  ( 0.1909286924077254199, -1.257064795538238577, -0.7137147910238503812 ) ) ;
#13089 = CARTESIAN_POINT ( 'NONE',  ( 0.08222542156927918622, -1.327483614382551913, 0.4683366274853996702 ) ) ;
#13090 = VERTEX_POINT ( 'NONE', #23585 ) ;
#13091 = LINE ( 'NONE', #38381, #12615 ) ;
#13092 = CARTESIAN_POINT ( 'NONE',  ( 0.1514761298305456472, -1.395251342086818447, 0.4173550238117827438 ) ) ;
#13093 = CARTESIAN_POINT ( 'NONE',  ( 0.4419048264408250715, -1.686280600454902245, 0.4284299735159858291 ) ) ;
#13094 = CARTESIAN_POINT ( 'NONE',  ( 0.4003286060160837767, -1.748155145820723622, -0.5147095092263663796 ) ) ;
#13095 = CARTESIAN_POINT ( 'NONE',  ( 0.4460384620557638624, -1.210965027603213562, 0.7166821082092738049 ) ) ;
#13097 = CARTESIAN_POINT ( 'NONE',  ( 0.2709623010280027278, -1.672610760848568967, 0.4891849873696615392 ) ) ;
#13096 = DIRECTION ( 'NONE',  ( 0.000000000000000000, 0.000000000000000000, -1.000000000000000000 ) ) ;
#13098 = CARTESIAN_POINT ( 'NONE',  ( 0.4929465528686918230, -1.082715557938388029, 0.5668025781570900090 ) ) ;
#13099 = ORIENTED_EDGE ( 'NONE', *, *, #37671, .F. ) ;
#13100 = CARTESIAN_POINT ( 'NONE',  ( 0.07891471443405570496, -1.242007717308747816, 0.7479880969011341030 ) ) ;
#13101 = ORIENTED_EDGE ( 'NONE', *, *, #28599, .F. ) ;
#13102 = CARTESIAN_POINT ( 'NONE',  ( 0.3881903648927482742, -1.602336578643832166, 0.6494100698158274954 ) ) ;
#13104 = CARTESIAN_POINT ( 'NONE',  ( 0.1973196604133173049, -0.5903291263510807019, 0.3099102803838534315 ) ) ;
#13103 = CARTESIAN_POINT ( 'NONE',  ( 0.08627532403026182128, -0.7836850491146717390, 0.03808575201433064827 ) ) ;
#13105 = DIRECTION ( 'NONE',  ( -1.000000000000000000, -0.000000000000000000, -0.000000000000000000 ) ) ;
#13106 = ORIENTED_EDGE ( 'NONE', *, *, #1880, .F. ) ;
#13107 = ORIENTED_EDGE ( 'NONE', *, *, #10931, .F. ) ;
#13108 = VERTEX_POINT ( 'NONE', #1575 ) ;
#13109 = FACE_OUTER_BOUND ( 'NONE', #13457, .T. ) ;
#13110 = CARTESIAN_POINT ( 'NONE',  ( 0.5669110650657969153, -1.503232105430957866, 0.5727642746916661309 ) ) ;
#13111 = ORIENTED_EDGE ( 'NONE', *, *, #24547, .T. ) ;
#13112 = FACE_BOUND ( 'NONE', #33487, .T. ) ;
#13113 = CARTESIAN_POINT ( 'NONE',  ( -2.112273405726188513E-14, -2.183180860297921466, -0.4937760292030871079 ) ) ;
#13114 = PLANE ( 'NONE',  #36222 ) ;
#13115 = CARTESIAN_POINT ( 'NONE',  ( 0.1854670398194577796, -0.8253301720469685687, 0.1740524287424448091 ) ) ;
#13116 = CARTESIAN_POINT ( 'NONE',  ( 0.08058916068514349051, -1.309220013881624789, 0.4727703015479322590 ) ) ;
#13117 = DIRECTION ( 'NONE',  ( -1.000000000000000000, -2.341930812374887555E-31, 1.664003471950578127E-31 ) ) ;
#13118 = DIRECTION ( 'NONE',  ( -0.8339988114203499281, 0.000000000000000000, -0.5517662390446189669 ) ) ;
#13119 = CARTESIAN_POINT ( 'NONE',  ( -0.2399999999999999079, -2.163125352510477661, -0.3606189578686002095 ) ) ;
#13120 = CARTESIAN_POINT ( 'NONE',  ( 0.1989976604547391836, -2.047409678865565574, -0.7132172901365276818 ) ) ;
#13121 = CARTESIAN_POINT ( 'NONE',  ( 0.3214803987143096675, -1.758709516440660092, 0.5682417262808786562 ) ) ;
#13122 = CARTESIAN_POINT ( 'NONE',  ( 0.1977770146402836882, -1.253111387755460271, -0.7170389573829240026 ) ) ;
#13123 = APPROVAL_STATUS ( 'not_yet_approved' ) ;
#13124 = CARTESIAN_POINT ( 'NONE',  ( -0.06980746140711623082, 0.000000000000000000, 0.000000000000000000 ) ) ;
#13125 = DIRECTION ( 'NONE',  ( -1.000000000000000000, -0.000000000000000000, -0.000000000000000000 ) ) ;
#13126 = CARTESIAN_POINT ( 'NONE',  ( 0.4712007327250372080, -1.210758550387179389, 0.4993402092387030367 ) ) ;
#13127 = DIRECTION ( 'NONE',  ( 1.000000000000000000, 0.000000000000000000, 1.517693329813472072E-15 ) ) ;
#13128 = CARTESIAN_POINT ( 'NONE',  ( 0.2322327485446251394, -1.539891620887370749, 0.8667544471685157959 ) ) ;
#13129 = CARTESIAN_POINT ( 'NONE',  ( 0.0002740986199341223918, -0.4896253918872909283, -0.006330435234190400287 ) ) ;
#13130 = DIRECTION ( 'NONE',  ( 1.000000000000000000, 6.779273404243070203E-32, 4.314083075427408311E-32 ) ) ;
#13131 = CARTESIAN_POINT ( 'NONE',  ( -0.2399999999999999079, -3.757033409510397881, -0.3216434158294207424 ) ) ;
#13132 = VERTEX_POINT ( 'NONE', #8332 ) ;
#13133 = EDGE_LOOP ( 'NONE', ( #37472, #22894, #4120, #35725, #4071, #14211, #15027, #22281, #13292, #4201, #38286, #4190 ) ) ;
#13134 = DIRECTION ( 'NONE',  ( -1.188678714063518227E-15, 1.000000000000000000, 3.263080277421930985E-16 ) ) ;
#13135 = ORIENTED_EDGE ( 'NONE', *, *, #31928, .F. ) ;
#13136 = CARTESIAN_POINT ( 'NONE',  ( -0.3000000000000000999, -3.723902497147952406, 0.1004495357399106253 ) ) ;
#13137 = CARTESIAN_POINT ( 'NONE',  ( 0.3584357512826374936, -1.733078788867854936, -0.4965168443801308285 ) ) ;
#13138 = CARTESIAN_POINT ( 'NONE',  ( 0.6055916563817613785, -1.479479184092913790, 0.5526975506195442867 ) ) ;
#13140 = ORIENTED_EDGE ( 'NONE', *, *, #23407, .F. ) ;
#13139 = CYLINDRICAL_SURFACE ( 'NONE', #11418, 0.08139150547213655496 ) ;
#13141 = EDGE_CURVE ( 'NONE', #30856, #33568, #1371, .T. ) ;
#13142 = ORIENTED_EDGE ( 'NONE', *, *, #4625, .F. ) ;
#13143 = LINE ( 'NONE', #16439, #3470 ) ;
#13144 = VERTEX_POINT ( 'NONE', #23177 ) ;
#13145 = AXIS2_PLACEMENT_3D ( 'NONE', #12620, #31755, #25183 ) ;
#13146 = CARTESIAN_POINT ( 'NONE',  ( 0.06022557703969336207, -0.7946678218323519616, 0.6553662645558616662 ) ) ;
#13148 = CARTESIAN_POINT ( 'NONE',  ( 0.1109092093543055241, -0.9286325583098424818, 0.1457252011008478843 ) ) ;
#13147 = CARTESIAN_POINT ( 'NONE',  ( 0.6241407479001672698, -1.577349794062394173, 0.4194501188810796921 ) ) ;
#13149 = DIRECTION ( 'NONE',  ( 1.000000000000000000, 0.000000000000000000, 0.000000000000000000 ) ) ;
#13150 = DIRECTION ( 'NONE',  ( -7.000205099780314469E-17, -1.000000000000000000, 6.590151126658399604E-16 ) ) ;
#13151 = CARTESIAN_POINT ( 'NONE',  ( 0.02999778723028687782, -2.087755359801442445, -0.2623954751430960242 ) ) ;
#13153 = ORIENTED_EDGE ( 'NONE', *, *, #25631, .T. ) ;
#13152 = EDGE_LOOP ( 'NONE', ( #18395, #38240, #36694, #33444 ) ) ;
#13154 = DIRECTION ( 'NONE',  ( 0.000000000000000000, 0.000000000000000000, -1.000000000000000000 ) ) ;
#13155 = CARTESIAN_POINT ( 'NONE',  ( 0.1130167353402539848, -0.9297503534748314813, 0.2195922346210762433 ) ) ;
#13156 = CARTESIAN_POINT ( 'NONE',  ( -0.04762200653275133755, -0.4434980416368527467, 0.1892582844414182897 ) ) ;
#13157 = DIRECTION ( 'NONE',  ( 0.4999999999999991118, -0.6509737717187596973, 0.5711682313769322894 ) ) ;
#13158 = EDGE_CURVE ( 'NONE', #14891, #8015, #10777, .T. ) ;
#13159 = SPHERICAL_SURFACE ( 'NONE', #4731, 0.01499999999999999944 ) ;
#13160 = CARTESIAN_POINT ( 'NONE',  ( 0.01055999984691518775, -0.5296565616858172065, 0.1504712070062352303 ) ) ;
#13161 = APPLIED_PERSON_AND_ORGANIZATION_ASSIGNMENT ( #34172, #12177, ( #24016 ) ) ;
#13162 = CARTESIAN_POINT ( 'NONE',  ( 0.4732168309031719033, -1.158657407058850231, 0.4227107324326277449 ) ) ;
#13163 = DIRECTION ( 'NONE',  ( 0.7783639739848380312, 0.6278132875326314366, -1.203114244385168678E-15 ) ) ;
#13164 = CARTESIAN_POINT ( 'NONE',  ( 0.7483483892508734359, -1.515136533364971339, 0.3157417262808776548 ) ) ;
#13165 = CARTESIAN_POINT ( 'NONE',  ( 0.02953079040095687308, 0.5250338024619264354, 0.07436286310882474215 ) ) ;
#13166 = CARTESIAN_POINT ( 'NONE',  ( 0.03113248654051816583, -0.1960639381401260983, -0.03948331496955503200 ) ) ;
#13167 = CIRCLE ( 'NONE', #15788, 0.01499999999999999424 ) ;
#13168 = CARTESIAN_POINT ( 'NONE',  ( 0.05268932808079999225, -0.2680477706051425102, 0.3844863582443106553 ) ) ;
#13169 = DIRECTION ( 'NONE',  ( 1.060606950627616897E-16, 6.122684696619992497E-17, 1.000000000000000000 ) ) ;
#13170 = CARTESIAN_POINT ( 'NONE',  ( 0.1051933607849167424, -1.410369882047322054, 0.5802930348479838907 ) ) ;
#13171 = CALENDAR_DATE ( 2026, 13, 10 ) ;
#13172 = AXIS2_PLACEMENT_3D ( 'NONE', #40309, #9235, #12139 ) ;
#13173 = CARTESIAN_POINT ( 'NONE',  ( 0.3683624102916023269, -1.734627145252658709, 0.4304674844703075265 ) ) ;
#13174 = CARTESIAN_POINT ( 'NONE',  ( 0.2280783781436956370, -1.602091971434898232, -0.6679261136964330658 ) ) ;
#13175 = CIRCLE ( 'NONE', #8590, 0.1946589359789743512 ) ;
#13176 = CARTESIAN_POINT ( 'NONE',  ( -0.01899496522503853549, 0.4667215747137464787, 0.2292237458735913169 ) ) ;
#13177 = FACE_OUTER_BOUND ( 'NONE', #13183, .T. ) ;
#13178 = EDGE_CURVE ( 'NONE', #17240, #7215, #4849, .T. ) ;
#13179 = B_SPLINE_CURVE_WITH_KNOTS ( 'NONE', 3,
 ( #30955, #13196, #12249, #40205 ),
 .UNSPECIFIED., .F., .F.,
 ( 4, 4 ),
 ( 0.000000000000000000, 0.001130163152920550789 ),
 .UNSPECIFIED. ) ;
#13180 = EDGE_CURVE ( 'NONE', #13785, #2772, #8150, .T. ) ;
#13181 = ORIENTED_EDGE ( 'NONE', *, *, #15256, .T. ) ;
#13182 = DIRECTION ( 'NONE',  ( -0.4999551463232372317, 0.8660512985181135770, -0.000000000000000000 ) ) ;
#13183 = EDGE_LOOP ( 'NONE', ( #23940, #24353, #467, #28140 ) ) ;
#13184 = CARTESIAN_POINT ( 'NONE',  ( 0.1169788285577439829, -1.415237608940837388, 0.5049415650359101448 ) ) ;
#13185 = CARTESIAN_POINT ( 'NONE',  ( 0.2675012769506449617, -1.687995237057803743, 0.6051696940006884295 ) ) ;
#13186 = EDGE_CURVE ( 'NONE', #9415, #5797, #13412, .T. ) ;
#13187 = CARTESIAN_POINT ( 'NONE',  ( 0.5539760576047348950, -1.429473381317945213, 0.7575193456964278704 ) ) ;
#13188 = ADVANCED_FACE ( 'NONE', ( #33014 ), #4818, .T. ) ;
#13190 = VERTEX_POINT ( 'NONE', #29950 ) ;
#13189 = CARTESIAN_POINT ( 'NONE',  ( -2.070754768975509474, -0.09959325338431662678, 0.3750000000000004996 ) ) ;
#13191 = EDGE_CURVE ( 'NONE', #19020, #17902, #36519, .T. ) ;
#13193 = ORIENTED_EDGE ( 'NONE', *, *, #16097, .F. ) ;
#13192 = ORIENTED_EDGE ( 'NONE', *, *, #29792, .F. ) ;
#13194 = CARTESIAN_POINT ( 'NONE',  ( 0.4957543717786337956, -1.693067643768066288, -0.5958955378105396106 ) ) ;
#13195 = ORIENTED_EDGE ( 'NONE', *, *, #6197, .F. ) ;
#13196 = CARTESIAN_POINT ( 'NONE',  ( 0.3827312705878086474, -1.762287005346949709, -0.5557439487639747044 ) ) ;
#13197 = CARTESIAN_POINT ( 'NONE',  ( -0.1630577892338991308, 0.4726628520879619377, 0.1187338422647633285 ) ) ;
#13198 = DATE_AND_TIME ( #19401, #3067 ) ;
#13199 = CARTESIAN_POINT ( 'NONE',  ( -0.004042975624358886508, -0.7404579356088993869, 0.09509064842808988283 ) ) ;
#13200 = VERTEX_POINT ( 'NONE', #26864 ) ;
#13201 = CARTESIAN_POINT ( 'NONE',  ( 0.09112929967733415793, -0.7529705612394925751, 0.2647947205566859585 ) ) ;
#13202 = APPLICATION_CONTEXT ( 'configuration controlled 3d designs of mechanical parts and assemblies' ) ;
#13203 = CARTESIAN_POINT ( 'NONE',  ( 0.5640895105453352931, -1.503407492374277510, 0.5358556994421860287 ) ) ;
#13204 = AXIS2_PLACEMENT_3D ( 'NONE', #32464, #4074, #1052 ) ;
#13205 =( BOUNDED_SURFACE ( )  B_SPLINE_SURFACE ( 3, 2, ( 
 ( #4275, #26500, #29385 ),
 ( #30184, #11259, #26716 ),
 ( #24038, #26295, #1416 ),
 ( #17035, #20527, #13930 ),
 ( #23828, #7562, #10649 ),
 ( #26905, #23224, #20136 ),
 ( #32664, #16845, #17637 ),
 ( #7337, #4468, #29782 ),
 ( #35956, #19916, #29575 ),
 ( #2014, #32452, #39034 ) ),
 .UNSPECIFIED., .F., .F., .T. ) 
 B_SPLINE_SURFACE_WITH_KNOTS ( ( 4, 2, 2, 2, 4 ),
 ( 3, 3 ),
 ( -5.681219383824043234E-17, 0.0005968317653288563113, 0.001193663530657769435, 0.001790495295986682667, 0.002387327061315595682 ),
 ( 0.000000000000000000, 1.000000000000000000 ),
 .UNSPECIFIED. ) 
 GEOMETRIC_REPRESENTATION_ITEM ( )  RATIONAL_B_SPLINE_SURFACE ( (
 ( 1.000000000000000000, 0.8817574585067788906, 1.000000000000000000),
 ( 1.000000000000000000, 0.8790203634614224271, 1.000000000000000000),
 ( 1.000000000000000000, 0.8757315292216423241, 1.000000000000000000),
 ( 1.000000000000000000, 0.8680526864388360408, 1.000000000000000000),
 ( 1.000000000000000000, 0.8636649569025933726, 1.000000000000000000),
 ( 1.000000000000000000, 0.8542598775336711636, 1.000000000000000000),
 ( 1.000000000000000000, 0.8491049259533275384, 1.000000000000000000),
 ( 1.000000000000000000, 0.8385672512564581460, 1.000000000000000000),
 ( 1.000000000000000000, 0.8331525095424542338, 1.000000000000000000),
 ( 1.000000000000000000, 0.8275829691081207917, 1.000000000000000000) ) ) 
 REPRESENTATION_ITEM ( '' )  SURFACE ( )  );
#13206 = CARTESIAN_POINT ( 'NONE',  ( 0.5402709567952270753, -1.518608341991216193, 0.6013252739479361120 ) ) ;
#13207 = ORIENTED_EDGE ( 'NONE', *, *, #28629, .T. ) ;
#13208 = CARTESIAN_POINT ( 'NONE',  ( 0.6470677939190155881, -1.605717247508275713, -0.4588775121292724690 ) ) ;
#13209 = EDGE_CURVE ( 'NONE', #7985, #37937, #23779, .T. ) ;
#13210 = CARTESIAN_POINT ( 'NONE',  ( -0.02953079040095693900, -0.2329676531120430660, 0.4763574306556350169 ) ) ;
#13211 = AXIS2_PLACEMENT_3D ( 'NONE', #3531, #13003, #893 ) ;
#13212 = CARTESIAN_POINT ( 'NONE',  ( 0.6726929394684000307, -1.451800111398652282, 0.4506308943308222625 ) ) ;
#13213 = APPROVAL ( #11306, 'UNSPECIFIED' ) ;
#13214 = CIRCLE ( 'NONE', #36199, 0.1500000000000009659 ) ;
#13215 = CARTESIAN_POINT ( 'NONE',  ( 0.3684487530574376835, -1.732198733335989838, 0.6142793637999888201 ) ) ;
#13216 = CARTESIAN_POINT ( 'NONE',  ( 0.6658408180046718750, -1.561543279147396213, 0.5677753029035824683 ) ) ;
#13217 = CARTESIAN_POINT ( 'NONE',  ( 0.4382015218937535539, -1.612541052972219502, -0.6615483979664104064 ) ) ;
#13218 = CARTESIAN_POINT ( 'NONE',  ( 0.6097373418327217687, -1.478078193704709387, 0.6043344841116261579 ) ) ;
#13219 = CARTESIAN_POINT ( 'NONE',  ( -0.2746410161513776482, -4.134278792318540674, -0.4999285807449073693 ) ) ;
#13220 = CARTESIAN_POINT ( 'NONE',  ( 0.1438681892407857876, -1.284094082863941111, 0.3157417262808777658 ) ) ;
#13221 = DIRECTION ( 'NONE',  ( 0.000000000000000000, 3.330669073875470114E-16, 1.000000000000000000 ) ) ;
#13222 = CARTESIAN_POINT ( 'NONE',  ( 0.004725042054567132541, -0.9785087964782590575, 0.4373990939698282343 ) ) ;
#13223 = CARTESIAN_POINT ( 'NONE',  ( 0.4955945803445692133, -1.095919195860131534, 0.6270439991606266972 ) ) ;
#13224 = DATE_AND_TIME ( #6840, #14805 ) ;
#13225 = CARTESIAN_POINT ( 'NONE',  ( -0.2746410161513779258, -2.183180860297908144, -0.4937760292030871079 ) ) ;
#13226 = CIRCLE ( 'NONE', #7272, 1.986674066779348102 ) ;
#13227 = LINE ( 'NONE', #16935, #26733 ) ;
#13228 = AXIS2_PLACEMENT_3D ( 'NONE', #16404, #15797, #34923 ) ;
#13229 = CARTESIAN_POINT ( 'NONE',  ( 0.4619339661384890272, -1.161483764442722277, 0.4182417262808779124 ) ) ;
#13230 = ADVANCED_FACE ( 'NONE', ( #17599 ), #1972, .F. ) ;
#13231 = AXIS2_PLACEMENT_3D ( 'NONE', #30718, #2539, #5196 ) ;
#13232 = ORIENTED_EDGE ( 'NONE', *, *, #32577, .T. ) ;
#13233 = DIRECTION ( 'NONE',  ( 0.000000000000000000, 0.000000000000000000, -1.000000000000000000 ) ) ;
#13234 = VECTOR ( 'NONE', #9329, 39.37007874015748143 ) ;
#13235 = B_SPLINE_CURVE_WITH_KNOTS ( 'NONE', 3,
 ( #22665, #4316, #9875, #38478, #34978, #28815 ),
 .UNSPECIFIED., .F., .F.,
 ( 4, 2, 4 ),
 ( 0.000000000000000000, 0.5000000000000000000, 1.000000000000000000 ),
 .UNSPECIFIED. ) ;
#13236 = CARTESIAN_POINT ( 'NONE',  ( 0.01057244653857888211, -0.5314355501429048889, 0.1721360658708845914 ) ) ;
#13237 = TOROIDAL_SURFACE ( 'NONE', #27049, 1.971674066779348866, 0.02999999999999999889 ) ;
#13238 = ADVANCED_FACE ( 'NONE', ( #16796 ), #33424, .T. ) ;
#13239 = CARTESIAN_POINT ( 'NONE',  ( -0.2399999999999999079, -3.838583118162426810, -0.3058907208964237734 ) ) ;
#13240 = ORIENTED_EDGE ( 'NONE', *, *, #21805, .T. ) ;
#13241 = CARTESIAN_POINT ( 'NONE',  ( 0.4093611158985690501, -1.131941421409890403, 0.5197417262808780025 ) ) ;
#13242 = EDGE_CURVE ( 'NONE', #31075, #35002, #2907, .T. ) ;
#13243 = CARTESIAN_POINT ( 'NONE',  ( 0.6810725650087121608, -1.407094454800211558, 0.5876998678990568159 ) ) ;
#13245 = ORIENTED_EDGE ( 'NONE', *, *, #6363, .F. ) ;
#13244 = ORIENTED_EDGE ( 'NONE', *, *, #31776, .F. ) ;
#13246 = LINE ( 'NONE', #35048, #7343 ) ;
#13247 = ORIENTED_EDGE ( 'NONE', *, *, #6965, .F. ) ;
#13248 = LINE ( 'NONE', #31173, #18454 ) ;
#13249 = EDGE_CURVE ( 'NONE', #15800, #31618, #40609, .T. ) ;
#13250 = CARTESIAN_POINT ( 'NONE',  ( 0.5982840689033031012, -1.484634935760666297, 0.5555640900495016909 ) ) ;
#13251 = CYLINDRICAL_SURFACE ( 'NONE', #6637, 0.1000000000000000056 ) ;
#13252 = ORIENTED_EDGE ( 'NONE', *, *, #20219, .F. ) ;
#13253 = CARTESIAN_POINT ( 'NONE',  ( 0.3373010429313745284, -1.775523145178461659, 0.9104836108820145713 ) ) ;
#13254 = CARTESIAN_POINT ( 'NONE',  ( 0.2327882622295160964, -0.8773484716388458837, 0.7033211034437524267 ) ) ;
#13255 = CARTESIAN_POINT ( 'NONE',  ( 0.08609365838014089445, -0.5574749707375634689, 0.2233878406577052278 ) ) ;
#13256 = EDGE_CURVE ( 'NONE', #1703, #3174, #22234, .T. ) ;
#13258 = CARTESIAN_POINT ( 'NONE',  ( 0.1581650021276240492, -1.285700486175305635, 0.4182417262808778013 ) ) ;
#13257 = CARTESIAN_POINT ( 'NONE',  ( 0.4268980379306124284, -1.643599345667950518, -0.4092648393969006704 ) ) ;
#13259 = CARTESIAN_POINT ( 'NONE',  ( 0.6012242321195756523, -1.481952306731540103, 0.4817067625245349261 ) ) ;
#13260 = CARTESIAN_POINT ( 'NONE',  ( 0.2384528902787253490, -0.9430836346886342092, 0.4549805665859378845 ) ) ;
#13261 = ORIENTED_EDGE ( 'NONE', *, *, #24487, .F. ) ;
#13262 = EDGE_CURVE ( 'NONE', #32636, #8912, #30747, .T. ) ;
#13263 = EDGE_LOOP ( 'NONE', ( #6039, #36988, #5607, #32591 ) ) ;
#13264 = CIRCLE ( 'NONE', #19173, 0.03000000000000006134 ) ;
#13265 = UNCERTAINTY_MEASURE_WITH_UNIT (LENGTH_MEASURE( 1.000000000000000082E-05 ), #925, 'distance_accuracy_value', 'NONE');
#13266 = CARTESIAN_POINT ( 'NONE',  ( 0.3545313261651519277, -1.624420226475606688, 0.5557399904385574851 ) ) ;
#13267 = EDGE_CURVE ( 'NONE', #25189, #38684, #971, .T. ) ;
#13268 = CARTESIAN_POINT ( 'NONE',  ( 0.4032708983214592924, -1.733579849462775657, -0.3059104399065430968 ) ) ;
#13269 = CIRCLE ( 'NONE', #27717, 0.1000000000000000194 ) ;
#13270 = EDGE_CURVE ( 'NONE', #17150, #7093, #21091, .T. ) ;
#13271 = AXIS2_PLACEMENT_3D ( 'NONE', #39573, #23765, #38974 ) ;
#13272 = CARTESIAN_POINT ( 'NONE',  ( -0.02872242845530464245, -0.4768947642620179339, -0.2371557650701917319 ) ) ;
#13273 = VECTOR ( 'NONE', #40571, 39.37007874015748143 ) ;
#13274 = DIRECTION ( 'NONE',  ( -1.000000000000000000, -7.857794173099924470E-32, -8.628166150854818811E-32 ) ) ;
#13275 = CARTESIAN_POINT ( 'NONE',  ( 0.3740232550247291066, -0.9210422728154799010, 0.7367171417286558777 ) ) ;
#13276 = CARTESIAN_POINT ( 'NONE',  ( 0.4482386148825789340, -1.121187352528194348, 0.5033830347951704365 ) ) ;
#13277 = CARTESIAN_POINT ( 'NONE',  ( 0.03938209889053093798, -1.119348185605193224, 0.6511811422115141301 ) ) ;
#13278 = DIRECTION ( 'NONE',  ( -1.000000000000000000, -1.188678714063518030E-15, -5.551115123125745108E-17 ) ) ;
#13279 = CARTESIAN_POINT ( 'NONE',  ( 0.1906988285079815049, -0.7702759449875168363, 0.3037686268896108710 ) ) ;
#13280 = EDGE_LOOP ( 'NONE', ( #8846, #18505, #6014, #35403 ) ) ;
#13281 = CARTESIAN_POINT ( 'NONE',  ( 0.3011262021662038935, -1.003312458126826012, 0.7429693187443193736 ) ) ;
#13282 = DIRECTION ( 'NONE',  ( 0.8660512985181134660, 0.4999551463232371762, 0.000000000000000000 ) ) ;
#13283 = PLANE ( 'NONE',  #27840 ) ;
#13284 = ORIENTED_EDGE ( 'NONE', *, *, #11959, .F. ) ;
#13285 = FACE_OUTER_BOUND ( 'NONE', #24377, .T. ) ;
#13286 = CARTESIAN_POINT ( 'NONE',  ( 0.4681011950856142634, -1.249373052585525334, 0.7957081402449762697 ) ) ;
#13287 = CIRCLE ( 'NONE', #25105, 0.01499999999999999424 ) ;
#13288 = EDGE_CURVE ( 'NONE', #12319, #11781, #14709, .T. ) ;
#13289 = CYLINDRICAL_SURFACE ( 'NONE', #28371, 0.4615209409081865166 ) ;
#13290 = CARTESIAN_POINT ( 'NONE',  ( 0.1504520142239714753, -1.289994444693127296, 0.4182417262808776903 ) ) ;
#13291 = ADVANCED_FACE ( 'NONE', ( #34228 ), #2979, .T. ) ;
#13292 = ORIENTED_EDGE ( 'NONE', *, *, #34083, .T. ) ;
#13293 = CARTESIAN_POINT ( 'NONE',  ( -0.04230188431063468257, -0.2683773510969740261, -0.3842417364743036523 ) ) ;
#13294 = CIRCLE ( 'NONE', #18550, 0.1762268159172233339 ) ;
#13295 = VECTOR ( 'NONE', #31455, 39.37007874015748854 ) ;
#13296 = CARTESIAN_POINT ( 'NONE',  ( 0.1889603646001475068, -0.5843802352234823694, 0.2966845687057266812 ) ) ;
#13297 = CARTESIAN_POINT ( 'NONE',  ( -0.3000000000000000999, -3.941790907013290823, -0.4709369376873030477 ) ) ;
#13298 = DIRECTION ( 'NONE',  ( 1.000000000000000000, 6.779273404243070203E-32, 4.314083075427408311E-32 ) ) ;
#13299 = CARTESIAN_POINT ( 'NONE',  ( 0.4905433154531526063, -1.277135180857473795, 0.5917710136670832899 ) ) ;
#13301 = DIRECTION ( 'NONE',  ( 0.4999999999999971134, 0.000000000000000000, -0.8660254037844402619 ) ) ;
#13300 = DIRECTION ( 'NONE',  ( 0.000000000000000000, -0.4393346272634560679, -0.8983234858820514646 ) ) ;
#13302 = CARTESIAN_POINT ( 'NONE',  ( 0.4919302148474398173, -1.082157928207513331, 0.5818935738131040258 ) ) ;
#13303 = ORIENTED_EDGE ( 'NONE', *, *, #38831, .T. ) ;
#13304 = DATE_AND_TIME ( #9807, #7596 ) ;
#13305 = CARTESIAN_POINT ( 'NONE',  ( 0.08883185798063782113, -1.305096067312203401, 0.7226060327209433698 ) ) ;
#13306 = ORIENTED_EDGE ( 'NONE', *, *, #32828, .F. ) ;
#13307 = CARTESIAN_POINT ( 'NONE',  ( 0.4134850239672457350, -1.589496775099021653, 0.5717027448869763662 ) ) ;
#13309 = CARTESIAN_POINT ( 'NONE',  ( 0.1923864837526514660, -0.6113152005538800005, 0.3150246423246629290 ) ) ;
#13308 = DIRECTION ( 'NONE',  ( -1.000000000000000000, -0.000000000000000000, -0.000000000000000000 ) ) ;
#13310 = CARTESIAN_POINT ( 'NONE',  ( 0.3397077535880359545, -1.654685348432989089, -0.3858274525146626055 ) ) ;
#13311 = VERTEX_POINT ( 'NONE', #40195 ) ;
#13312 = ADVANCED_FACE ( 'NONE', ( #6038 ), #14057, .F. ) ;
#13313 = CARTESIAN_POINT ( 'NONE',  ( 0.3603245586327842864, -1.274710059600435486, 0.5779767968998822392 ) ) ;
#13314 = CARTESIAN_POINT ( 'NONE',  ( 0.1231242327260526209, -0.6037900324288171250, 0.3295969312879552526 ) ) ;
#13315 = EDGE_LOOP ( 'NONE', ( #26519, #36105, #36220, #38941 ) ) ;
#13316 = CARTESIAN_POINT ( 'NONE',  ( 0.3923243630925510872, -1.966611948492501316, -0.4968729097670202544 ) ) ;
#13317 = CARTESIAN_POINT ( 'NONE',  ( 5.473410438793996596E-16, -0.2899999999999993694, -0.01750000000000073372 ) ) ;
#13318 = B_SPLINE_CURVE_WITH_KNOTS ( 'NONE', 3,
 ( #22221, #456, #34739, #32066, #25916, #9845, #31869, #6545, #22839, #35542 ),
 .UNSPECIFIED., .F., .F.,
 ( 4, 3, 3, 4 ),
 ( 3.193936382936243481E-15, 0.0005080000155662609419, 0.002540000352560990542, 0.004712884098096298095 ),
 .UNSPECIFIED. ) ;
#13319 = CARTESIAN_POINT ( 'NONE',  ( 0.1853834160488257721, -0.8311217846528596853, 0.1678811282091721702 ) ) ;
#13320 = DIRECTION ( 'NONE',  ( 1.664003471950577032E-31, 3.330669073875470114E-16, 1.000000000000000000 ) ) ;
#13321 = AXIS2_PLACEMENT_3D ( 'NONE', #28407, #21639, #25534 ) ;
#13322 = CARTESIAN_POINT ( 'NONE',  ( -0.002218965743620939825, -1.368565310413371705, -0.3828039145932563558 ) ) ;
#13323 = DIRECTION ( 'NONE',  ( -1.000000000000000000, -7.857794173099924470E-32, -8.628166150854818811E-32 ) ) ;
#13324 = DIRECTION ( 'NONE',  ( 0.4999551463232373427, -0.8660512985181134660, 0.000000000000000000 ) ) ;
#13325 = AXIS2_PLACEMENT_3D ( 'NONE', #10703, #29835, #1275 ) ;
#13326 = CARTESIAN_POINT ( 'NONE',  ( 0.3860871553693445701, -1.736163695054018241, -0.7193333307755221950 ) ) ;
#13327 = CIRCLE ( 'NONE', #255, 0.07999999999999996003 ) ;
#13328 = FACE_OUTER_BOUND ( 'NONE', #39860, .T. ) ;
#13329 = CARTESIAN_POINT ( 'NONE',  ( -0.3000000000000000999, -2.511040369707300268, -0.4948468226404901804 ) ) ;
#13330 = APPROVAL_DATE_TIME ( #32054, #14192 ) ;
#13331 = AXIS2_PLACEMENT_3D ( 'NONE', #11600, #20445, #33584 ) ;
#13332 = CARTESIAN_POINT ( 'NONE',  ( 0.6492251849256891472, -1.449833129731838977, -0.6190067879899118219 ) ) ;
#13333 = CARTESIAN_POINT ( 'NONE',  ( 0.01548846960707511190, 0.09061086148576739940, 0.5171215251571016358 ) ) ;
#13334 = CARTESIAN_POINT ( 'NONE',  ( 0.1848746338969347036, -0.6872459287048060528, -0.02854997582304983142 ) ) ;
#13335 = DIRECTION ( 'NONE',  ( -1.000000000000000000, -0.000000000000000000, -0.000000000000000000 ) ) ;
#13336 = DIRECTION ( 'NONE',  ( 7.771561172376107616E-16, -7.170354002788761615E-17, 1.000000000000000000 ) ) ;
#13337 = AXIS2_PLACEMENT_3D ( 'NONE', #30077, #30258, #39731 ) ;
#13338 = CARTESIAN_POINT ( 'NONE',  ( 0.2912354967743938094, -1.730409171686111414, 0.5958501190287942562 ) ) ;
#13339 = CARTESIAN_POINT ( 'NONE',  ( -0.0003982523508731287097, -0.9350673170737405782, 0.1130908737492680588 ) ) ;
#13340 = CARTESIAN_POINT ( 'NONE',  ( 0.4173053972040562387, -1.590420842066649465, -0.4142378684116532761 ) ) ;
#13341 = CARTESIAN_POINT ( 'NONE',  ( 0.03654364704248871248, -0.3642884434512947966, 0.3592365245254307560 ) ) ;
#13342 = LINE ( 'NONE', #13131, #7876 ) ;
#13343 = EDGE_LOOP ( 'NONE', ( #746, #900, #29915, #4665, #32067 ) ) ;
#13344 = ORIENTED_EDGE ( 'NONE', *, *, #387, .F. ) ;
#13345 = CARTESIAN_POINT ( 'NONE',  ( 0.05634301242525747294, -0.2614060064472272793, -0.3772872482281126039 ) ) ;
#13346 = VERTEX_POINT ( 'NONE', #8937 ) ;
#13347 = CARTESIAN_POINT ( 'NONE',  ( -0.04154009738085497061, -0.01731731106881116700, 0.4700109389422703066 ) ) ;
#13348 = CARTESIAN_POINT ( 'NONE',  ( 0.5838497309001715596, -1.602250078375488274, -0.4543158100596352833 ) ) ;
#13349 = CIRCLE ( 'NONE', #29113, 0.08749999999977554899 ) ;
#13350 = CARTESIAN_POINT ( 'NONE',  ( 0.4258289169993133561, -1.184892057508847296, 0.7715538982757290665 ) ) ;
#13352 = ORIENTED_EDGE ( 'NONE', *, *, #21530, .F. ) ;
#13351 = CARTESIAN_POINT ( 'NONE',  ( -0.1088121136105147380, -0.4964308608213456875, 0.09999999999999989453 ) ) ;
#13353 = CARTESIAN_POINT ( 'NONE',  ( 0.4594195809631357874, -1.060066247262113182, 0.7450334795338161564 ) ) ;
#13354 = CARTESIAN_POINT ( 'NONE',  ( 0.3536427585406661245, -1.745782643693225777, -0.5548824076054205134 ) ) ;
#13355 = ORIENTED_EDGE ( 'NONE', *, *, #16039, .T. ) ;
#13356 = CARTESIAN_POINT ( 'NONE',  ( 0.1976682978929888146, -0.7785829950231940577, 0.3156600736487931713 ) ) ;
#13357 = CIRCLE ( 'NONE', #25854, 0.1600000000000015854 ) ;
#13358 = ORIENTED_EDGE ( 'NONE', *, *, #37133, .T. ) ;
#13359 = AXIS2_PLACEMENT_3D ( 'NONE', #27163, #8614, #27764 ) ;
#13360 = CARTESIAN_POINT ( 'NONE',  ( 0.3013866175335212505, -1.646058783738227005, 0.7062181652641160712 ) ) ;
#13362 = CARTESIAN_POINT ( 'NONE',  ( 0.1130275343130942994, -0.7030560519982989032, -0.09532014130486921033 ) ) ;
#13361 = DIRECTION ( 'NONE',  ( 0.000000000000000000, 0.000000000000000000, -1.000000000000000000 ) ) ;
#13363 = CARTESIAN_POINT ( 'NONE',  ( 0.3051775095946583360, -1.756515733326251105, 0.5493018342092053086 ) ) ;
#13364 = CARTESIAN_POINT ( 'NONE',  ( -0.1969433606228599420, 0.5138636982738206127, 0.1528658435937004789 ) ) ;
#13365 = CARTESIAN_POINT ( 'NONE',  ( -2.097120186386331940E-14, -2.063349513125158463, -0.3027437064113706056 ) ) ;
#13366 = ORIENTED_EDGE ( 'NONE', *, *, #31776, .T. ) ;
#13367 = DIRECTION ( 'NONE',  ( 1.000000000000000000, 0.000000000000000000, 0.000000000000000000 ) ) ;
#13368 = CARTESIAN_POINT ( 'NONE',  ( 0.1859972922984850507, -0.8393112992344217149, 0.1889479090597321054 ) ) ;
#13369 = VECTOR ( 'NONE', #32710, 39.37007874015748143 ) ;
#13370 = LINE ( 'NONE', #31896, #15411 ) ;
#13371 = CARTESIAN_POINT ( 'NONE',  ( 0.5951727137181233029, -1.456125169982292800, 0.6236106044506557478 ) ) ;
#13372 = CARTESIAN_POINT ( 'NONE',  ( 0.1068110449628701525, -0.8327494205295853380, 0.2803338686668198076 ) ) ;
#13373 = CARTESIAN_POINT ( 'NONE',  ( 0.1241306338573257562, -1.117108204751295686, 0.8885289527623265737 ) ) ;
#13374 = EDGE_CURVE ( 'NONE', #20247, #24904, #21980, .T. ) ;
#13375 = CARTESIAN_POINT ( 'NONE',  ( 0.4062230848227129099, -1.145582794160925788, 0.4248905050063985778 ) ) ;
#13376 = CARTESIAN_POINT ( 'NONE',  ( -0.1613941814439381617, 0.5013693833954199208, 0.3301047373962386899 ) ) ;
#13377 = DIRECTION ( 'NONE',  ( 1.000000000000000000, 8.054771744420843492E-13, 1.518808759990554105E-12 ) ) ;
#13378 = DIRECTION ( 'NONE',  ( -1.540743955509782771E-31, -0.9849933812515921927, -0.1725921171159214562 ) ) ;
#13379 = DIRECTION ( 'NONE',  ( -1.000000000000000000, -0.000000000000000000, -0.000000000000000000 ) ) ;
#13380 = CIRCLE ( 'NONE', #18640, 0.01000000000000003490 ) ;
#13381 = CARTESIAN_POINT ( 'NONE',  ( 0.05078310099560401358, -0.3164655623698865439, 0.3525377550955086092 ) ) ;
#13382 = CARTESIAN_POINT ( 'NONE',  ( 0.1808993972631122160, -0.4988400884274764024, 0.1169007445746203938 ) ) ;
#13383 = CARTESIAN_POINT ( 'NONE',  ( 0.1183428582170880927, -1.407360454669288385, 0.6103212893459412092 ) ) ;
#13384 = AXIS2_PLACEMENT_3D ( 'NONE', #37314, #21295, #21509 ) ;
#13385 = CIRCLE ( 'NONE', #31132, 0.1749999999999999889 ) ;
#13386 = PRODUCT ( 'Outer shift plate', 'Outer shift plate', '', ( #17126 ) ) ;
#13387 = DIRECTION ( 'NONE',  ( 1.000000000000000000, 0.000000000000000000, 0.000000000000000000 ) ) ;
#13388 = CARTESIAN_POINT ( 'NONE',  ( -0.3000000000000000999, -2.909786385774835171, -0.3705357231075771529 ) ) ;
#13389 = CYLINDRICAL_SURFACE ( 'NONE', #29735, 0.01499999999999999424 ) ;
#13390 = B_SPLINE_CURVE_WITH_KNOTS ( 'NONE', 3,
 ( #16395, #37803, #38401, #19294, #28750, #9622, #612, #10237, #35934, #26694, #26275, #20110, #26087, #35722, #38791, #1204, #1390, #7928, #38606, #13707, #10623, #29973 ),
 .UNSPECIFIED., .F., .F.,
 ( 4, 2, 2, 2, 2, 2, 2, 2, 2, 2, 4 ),
 ( 0.000000000000000000, 0.0007781589143522405546, 0.001556317828704481109, 0.003112635657408943570, 0.006225271314817849844, 0.007781589143522303631, 0.008559748057874530525, 0.009337906972226757418, 0.01089422480093120947, 0.01167238371528343463, 0.01245054262963566152 ),
 .UNSPECIFIED. ) ;
#13391 = DIRECTION ( 'NONE',  ( 0.4999551463232372317, -0.8660512985181135770, 0.000000000000000000 ) ) ;
#13392 = CIRCLE ( 'NONE', #35095, 0.1000000000000000194 ) ;
#13393 = CIRCLE ( 'NONE', #8126, 0.1333070866141732591 ) ;
#13394 = ORIENTED_EDGE ( 'NONE', *, *, #15935, .T. ) ;
#13395 = CARTESIAN_POINT ( 'NONE',  ( 0.4087622015559044253, -1.136016260234564701, 0.4319160579129420752 ) ) ;
#13396 = ORIENTED_EDGE ( 'NONE', *, *, #20966, .F. ) ;
#13397 = CARTESIAN_POINT ( 'NONE',  ( 0.6511295279640838540, -1.603372484741562243, -0.5770581850489380216 ) ) ;
#13398 = CARTESIAN_POINT ( 'NONE',  ( 0.3387696793961558761, -1.066620522076481947, 0.7898564859712591257 ) ) ;
#13400 = ORIENTED_EDGE ( 'NONE', *, *, #40185, .T. ) ;
#13399 = DIRECTION ( 'NONE',  ( -3.406373435249024214E-19, -1.000000000000000000, -7.170354002788761615E-17 ) ) ;
#13402 = EDGE_LOOP ( 'NONE', ( #19333, #10019, #9441, #37393, #20649, #1833, #9 ) ) ;
#13401 = VERTEX_POINT ( 'NONE', #15528 ) ;
#13403 = CARTESIAN_POINT ( 'NONE',  ( 0.6649543069449874721, -1.548310422546823606, 0.6796974753901866562 ) ) ;
#13404 = ORIENTED_EDGE ( 'NONE', *, *, #11986, .F. ) ;
#13405 = CARTESIAN_POINT ( 'NONE',  ( 0.3264244126186546802, -1.294301107126978767, -0.5166151207188711680 ) ) ;
#13406 = DIRECTION ( 'NONE',  ( -0.4999551463232372317, 0.8660512985181134660, 0.000000000000000000 ) ) ;
#13407 = APPROVAL_STATUS ( 'not_yet_approved' ) ;
#13408 = AXIS2_PLACEMENT_3D ( 'NONE', #10829, #27281, #17791 ) ;
#13409 = CARTESIAN_POINT ( 'NONE',  ( -0.001051960901064252297, -0.8469330747986114627, -0.06462206035643724977 ) ) ;
#13410 = EDGE_LOOP ( 'NONE', ( #554, #37270, #29022, #3060, #28144, #12805 ) ) ;
#13411 = CARTESIAN_POINT ( 'NONE',  ( 0.2704459367631082412, -0.9896522447148606849, 0.6916254092597398095 ) ) ;
#13412 = CIRCLE ( 'NONE', #11456, 0.1400000000000013456 ) ;
#13413 = CARTESIAN_POINT ( 'NONE',  ( 0.4241308954920427476, -1.602590692387141136, -0.3549062565033732630 ) ) ;
#13414 = CIRCLE ( 'NONE', #16712, 0.01500000000000005669 ) ;
#13415 = CARTESIAN_POINT ( 'NONE',  ( 0.5399440942408553212, -1.515719783342790228, 0.6355856557526133876 ) ) ;
#13416 = ORIENTED_EDGE ( 'NONE', *, *, #31898, .F. ) ;
#13417 = EDGE_CURVE ( 'NONE', #20195, #2786, #18391, .T. ) ;
#13418 = CARTESIAN_POINT ( 'NONE',  ( -2.070754768975505034, -0.09959325338431362917, 0.09550516381870004234 ) ) ;
#13419 = DIRECTION ( 'NONE',  ( -0.4999999999999971134, 0.000000000000000000, 0.8660254037844402619 ) ) ;
#13420 = AXIS2_PLACEMENT_3D ( 'NONE', #2913, #6189, #37453 ) ;
#13421 = CARTESIAN_POINT ( 'NONE',  ( 0.6686281500267547973, -1.536646776530108838, 0.4440777536512748314 ) ) ;
#13422 = CARTESIAN_POINT ( 'NONE',  ( 0.3048570497350418518, -1.756853555320991189, 0.5694442476137144826 ) ) ;
#13423 = CARTESIAN_POINT ( 'NONE',  ( 0.3766087435943047956, -1.648707884900325604, -0.6331061992164871421 ) ) ;
#13424 = EDGE_CURVE ( 'NONE', #13497, #8912, #171, .T. ) ;
#13425 = CIRCLE ( 'NONE', #25231, 0.03749999999977554621 ) ;
#13426 = CARTESIAN_POINT ( 'NONE',  ( 0.5158078970339151637, -1.604330220985429767, -0.6142783388584680537 ) ) ;
#13427 = EDGE_CURVE ( 'NONE', #17938, #1703, #2608, .T. ) ;
#13428 = CARTESIAN_POINT ( 'NONE',  ( 0.5253354359398262341, -1.363713559762562033, 0.7943058037876152833 ) ) ;
#13429 = CIRCLE ( 'NONE', #7477, 0.5400000000000018119 ) ;
#13430 = CARTESIAN_POINT ( 'NONE',  ( -1.465953029183149908E-06, -0.7472984521689456372, -0.1083893734920139823 ) ) ;
#13431 = ADVANCED_FACE ( 'NONE', ( #31757 ), #38195, .T. ) ;
#13432 = DIRECTION ( 'NONE',  ( -0.4999999999999986677, 0.000000000000000000, 0.8660254037844393737 ) ) ;
#13433 = EDGE_CURVE ( 'NONE', #19821, #5177, #37728, .T. ) ;
#13434 = CARTESIAN_POINT ( 'NONE',  ( 0.4620959648888870452, -1.073996026857335417, -0.6125958513722957743 ) ) ;
#13435 = ADVANCED_FACE ( 'NONE', ( #3364 ), #37936, .F. ) ;
#13436 = CARTESIAN_POINT ( 'NONE',  ( -0.002083146443013338383, -0.8967360763018588088, 0.1457185332388704624 ) ) ;
#13437 = CARTESIAN_POINT ( 'NONE',  ( 0.4864609864856930255, -1.087049186798351608, 0.6366279691173203359 ) ) ;
#13438 = APPLICATION_PROTOCOL_DEFINITION ( 'international standard', 'automotive_design', 2000, #13202 ) ;
#13439 = DIRECTION ( 'NONE',  ( -1.000000000000000000, 0.000000000000000000, 0.000000000000000000 ) ) ;
#13440 = VECTOR ( 'NONE', #20658, 39.37007874015748854 ) ;
#13441 = TOROIDAL_SURFACE ( 'NONE', #18702, 0.04500000000000023426, 0.01499999999999999944 ) ;
#13442 = CARTESIAN_POINT ( 'NONE',  ( -0.2399999999999999079, -2.317513802384189692, -0.4844117508308344866 ) ) ;
#13443 = CARTESIAN_POINT ( 'NONE',  ( 0.4780517542678584531, -1.172877689127207024, 0.4182417262808778013 ) ) ;
#13444 = CIRCLE ( 'NONE', #24625, 0.5114999999999890745 ) ;
#13445 = CONICAL_SURFACE ( 'NONE', #37761, 0.5614999999999926716, 1.047197551196600296 ) ;
#13446 = ADVANCED_FACE ( 'NONE', ( #38125 ), #9949, .T. ) ;
#13447 = ORIENTED_EDGE ( 'NONE', *, *, #40185, .F. ) ;
#13448 = CARTESIAN_POINT ( 'NONE',  ( 0.4415369156091736302, -1.574510176363862479, 0.6025007236356999529 ) ) ;
#13449 = LOCAL_TIME ( 0, 53, 7.000000000000000000, #23873 ) ;
#13450 = APPROVAL ( #13123, 'UNSPECIFIED' ) ;
#13451 = CARTESIAN_POINT ( 'NONE',  ( 0.02423924040295103929, 0.06026721965051373003, 0.1249999999999993477 ) ) ;
#13452 = CARTESIAN_POINT ( 'NONE',  ( 0.08522006272954811557, -0.8097442991749735919, 0.1288917670895001755 ) ) ;
#13453 = EDGE_LOOP ( 'NONE', ( #15322, #13232, #16258, #14449, #26415, #10671, #1280, #2494 ) ) ;
#13454 = CARTESIAN_POINT ( 'NONE',  ( 0.1437340355044557927, -1.283861693981850349, 0.4177417262808780229 ) ) ;
#13455 = CIRCLE ( 'NONE', #22672, 0.5400000000000001465 ) ;
#13456 = CARTESIAN_POINT ( 'NONE',  ( 0.2120163453477715010, -0.5915265038663817254, 0.4276896445164236615 ) ) ;
#13458 = VERTEX_POINT ( 'NONE', #19626 ) ;
#13457 = EDGE_LOOP ( 'NONE', ( #23889, #5486, #29999, #9128 ) ) ;
#13459 = CYLINDRICAL_SURFACE ( 'NONE', #17234, 0.08000000000000000167 ) ;
#13460 =( BOUNDED_SURFACE ( )  B_SPLINE_SURFACE ( 3, 2, ( 
 ( #10037, #16613, #6530 ),
 ( #6735, #34928, #625 ),
 ( #3856, #16408, #1026 ),
 ( #35524, #4265, #19903 ) ),
 .UNSPECIFIED., .F., .F., .F. ) 
 B_SPLINE_SURFACE_WITH_KNOTS ( ( 4, 4 ),
 ( 3, 3 ),
 ( 6.938893903907228378E-18, 0.001175067160604088314 ),
 ( 0.000000000000000000, 1.000000000000000000 ),
 .UNSPECIFIED. ) 
 GEOMETRIC_REPRESENTATION_ITEM ( )  RATIONAL_B_SPLINE_SURFACE ( (
 ( 1.000000000000000000, 0.9000550641257055728, 1.000000000000000000),
 ( 1.000000000000000000, 0.9100375230753980915, 1.000000000000000000),
 ( 1.000000000000000000, 0.9182507546028528811, 1.000000000000000000),
 ( 1.000000000000000000, 0.9231872052445992960, 1.000000000000000000) ) ) 
 REPRESENTATION_ITEM ( '' )  SURFACE ( )  );
#13461 = ORIENTED_EDGE ( 'NONE', *, *, #1420, .T. ) ;
#13462 = CARTESIAN_POINT ( 'NONE',  ( -0.2746410161513782033, -1.835749455202394298, -0.3938319975228649072 ) ) ;
#13463 = CARTESIAN_POINT ( 'NONE',  ( -0.02000000000000000042, -2.177105168660885326, -0.2518349584362399862 ) ) ;
#13464 = CARTESIAN_POINT ( 'NONE',  ( -0.03642997641689546540, 0.5061875831641691192, -0.07642488348723255887 ) ) ;
#13465 = VERTEX_POINT ( 'NONE', #20429 ) ;
#13466 = CARTESIAN_POINT ( 'NONE',  ( 0.08612155440268152995, -0.6906331012568079908, 0.7711272665534666393 ) ) ;
#13467 = CARTESIAN_POINT ( 'NONE',  ( 0.08977666489915449299, -0.6469118995760279045, 0.2018334186708977129 ) ) ;
#13468 = CARTESIAN_POINT ( 'NONE',  ( 0.01518662448050903287, -0.4837837598039577136, 0.3562993236613829495 ) ) ;
#13469 = CARTESIAN_POINT ( 'NONE',  ( 0.3306407300723779308, -1.212941238661646715, 0.8562008246371364262 ) ) ;
#13471 = CARTESIAN_POINT ( 'NONE',  ( -0.1081899703030904242, -0.4934552128793911474, 0.3439540350797880564 ) ) ;
#13470 = CARTESIAN_POINT ( 'NONE',  ( 0.4996517707920770102, -1.622836357335520230, -0.4447391335572282167 ) ) ;
#13472 = CARTESIAN_POINT ( 'NONE',  ( 0.08524282091866439148, -1.033473658707478871, 0.5862322604168024309 ) ) ;
#13473 = ORIENTED_EDGE ( 'NONE', *, *, #19055, .T. ) ;
#13474 = VECTOR ( 'NONE', #19141, 39.37007874015748143 ) ;
#13475 = CARTESIAN_POINT ( 'NONE',  ( 0.4000099798367555137, -1.704638381955407400, 0.4282417262808771441 ) ) ;
#13476 = CARTESIAN_POINT ( 'NONE',  ( 0.2286386731437905495, -0.6007009410402062155, 0.5044687263126308441 ) ) ;
#13477 = AXIS2_PLACEMENT_3D ( 'NONE', #26600, #32333, #7840 ) ;
#13478 = CARTESIAN_POINT ( 'NONE',  ( -0.02953079040095640123, 0.2329676531120523086, -0.4763574306556315752 ) ) ;
#13479 = AXIS2_PLACEMENT_3D ( 'NONE', #39586, #8331, #20901 ) ;
#13480 = EDGE_CURVE ( 'NONE', #29455, #19345, #12885, .T. ) ;
#13481 = LOCAL_TIME ( 0, 53, 7.000000000000000000, #39945 ) ;
#13482 = DIRECTION ( 'NONE',  ( -6.217248937900885304E-15, 2.158931604386568927E-14, 1.000000000000000000 ) ) ;
#13483 = B_SPLINE_CURVE_WITH_KNOTS ( 'NONE', 3,
 ( #8427, #11922, #20993, #33513 ),
 .UNSPECIFIED., .F., .F.,
 ( 4, 4 ),
 ( 8.673617379884035472E-19, 0.004712633589911092123 ),
 .UNSPECIFIED. ) ;
#13484 = EDGE_CURVE ( 'NONE', #25919, #34346, #14742, .T. ) ;
#13485 = DIRECTION ( 'NONE',  ( -0.4999551463232371762, 0.8660512985181134660, -0.000000000000000000 ) ) ;
#13486 = EDGE_CURVE ( 'NONE', #16489, #27939, #20001, .T. ) ;
#13487 = CIRCLE ( 'NONE', #33836, 0.01000000000000002970 ) ;
#13488 = CARTESIAN_POINT ( 'NONE',  ( 0.6145270684574122289, -1.293427813764720824, 0.7790094959668801833 ) ) ;
#13489 = CARTESIAN_POINT ( 'NONE',  ( 0.4103533436992015671, -1.245885857446504374, 0.5182417262812503145 ) ) ;
#13490 = DIRECTION ( 'NONE',  ( 1.000000000000000000, 2.341930812374887555E-31, -1.664003471950578127E-31 ) ) ;
#13491 = CARTESIAN_POINT ( 'NONE',  ( 0.05634206451479474576, 0.4332270636364591865, -0.1516455289248239691 ) ) ;
#13492 = CARTESIAN_POINT ( 'NONE',  ( 0.4751758298663426583, -1.652426242819087010, -0.6334442537810192064 ) ) ;
#13493 = CARTESIAN_POINT ( 'NONE',  ( 0.2755989780306793424, -1.016327101040557901, 0.7228497138915612741 ) ) ;
#13494 = CARTESIAN_POINT ( 'NONE',  ( 0.02869712619511882029, -0.3396447909410097998, 0.3648221446286689651 ) ) ;
#13495 = CARTESIAN_POINT ( 'NONE',  ( 0.5953303036072959964, -1.457508885835639978, 0.6057417262805095959 ) ) ;
#13496 = EDGE_CURVE ( 'NONE', #24117, #652, #31525, .T. ) ;
#13497 = VERTEX_POINT ( 'NONE', #1743 ) ;
#13498 = CARTESIAN_POINT ( 'NONE',  ( -0.2399999999999999079, -2.416006048095809877, -1.059240699271965402 ) ) ;
#13499 = CARTESIAN_POINT ( 'NONE',  ( -0.07216878364870257800, 0.08000000000000023759, 0.1249999999999993477 ) ) ;
#13500 = EDGE_CURVE ( 'NONE', #17083, #25706, #25256, .T. ) ;
#13501 = CIRCLE ( 'NONE', #14138, 0.01500000000000001332 ) ;
#13502 = CARTESIAN_POINT ( 'NONE',  ( 0.02999607453758943582, -2.087869005097288788, -0.7252195465745524539 ) ) ;
#13503 = CARTESIAN_POINT ( 'NONE',  ( -0.02000000000000000042, -2.585754275622221154, -0.2040099479399058724 ) ) ;
#13504 = CIRCLE ( 'NONE', #11541, 0.1033070866141734129 ) ;
#13505 = CARTESIAN_POINT ( 'NONE',  ( 0.1098552746376899730, -0.9433422683584672397, 0.6393798403408993414 ) ) ;
#13506 = ORIENTED_EDGE ( 'NONE', *, *, #31764, .T. ) ;
#13507 = FACE_OUTER_BOUND ( 'NONE', #29402, .T. ) ;
#13508 = CARTESIAN_POINT ( 'NONE',  ( 0.3817504269947160078, -1.726033828776056378, 0.4251703030630522018 ) ) ;
#13509 = LOCAL_TIME ( 0, 53, 7.000000000000000000, #19494 ) ;
#13510 = DIRECTION ( 'NONE',  ( 0.3468893892380798261, -0.9373665302208751271, -0.03180785525163549315 ) ) ;
#13511 = CARTESIAN_POINT ( 'NONE',  ( 0.1992677735555647978, -1.286890397454214963, -0.7430133923425328302 ) ) ;
#13512 = CARTESIAN_POINT ( 'NONE',  ( 0.3846646194939473684, -1.128865715846599560, 0.7236265502079624046 ) ) ;
#13514 = CARTESIAN_POINT ( 'NONE',  ( 0.4000099798367660608, -1.704638381955401183, 0.4182417262808776903 ) ) ;
#13513 = DIRECTION ( 'NONE',  ( -1.000000000000000000, -2.280301054154495132E-31, 1.664003471950577689E-31 ) ) ;
#13515 = CARTESIAN_POINT ( 'NONE',  ( -0.1045574869087414066, -0.4741643323009803734, 0.09813923389047436718 ) ) ;
#13516 = EDGE_LOOP ( 'NONE', ( #28589, #16148, #39606, #9056 ) ) ;
#13517 = APPROVAL_ROLE ( '' ) ;
#13518 = AXIS2_PLACEMENT_3D ( 'NONE', #8411, #5303, #3073 ) ;
#13519 = DIRECTION ( 'NONE',  ( 0.4999551463232372317, -0.8660512985181133550, 0.000000000000000000 ) ) ;
#13520 = VERTEX_POINT ( 'NONE', #10770 ) ;
#13521 = VERTEX_POINT ( 'NONE', #38536 ) ;
#13522 = CARTESIAN_POINT ( 'NONE',  ( 0.1039735380096880463, -0.7886731789469053622, 0.6333316274729952067 ) ) ;
#13524 = CARTESIAN_POINT ( 'NONE',  ( 0.2020481313132333201, -0.6875151388636763228, 0.3386544405593424623 ) ) ;
#13523 = CARTESIAN_POINT ( 'NONE',  ( 0.06453910615976091170, -0.8346243741771329772, 0.1288229811268807867 ) ) ;
#13525 = CARTESIAN_POINT ( 'NONE',  ( 0.1302110173660007697, -1.291756932227970944, 0.4882610538605935413 ) ) ;
#13526 = VERTEX_POINT ( 'NONE', #7458 ) ;
#13527 = CARTESIAN_POINT ( 'NONE',  ( 0.3264055361853325232, -1.294304910894763072, 0.5706360388247739834 ) ) ;
#13528 = CARTESIAN_POINT ( 'NONE',  ( 0.1205771094107126462, -0.5739007583310267169, 0.2533364529363901219 ) ) ;
#13529 = ORIENTED_EDGE ( 'NONE', *, *, #2482, .T. ) ;
#13530 = DIRECTION ( 'NONE',  ( -1.387778780781449423E-15, 6.590151126658375938E-16, -1.000000000000000000 ) ) ;
#13531 = CARTESIAN_POINT ( 'NONE',  ( 0.007992636382689974339, -1.702839484628106081, -0.3714452569209771848 ) ) ;
#13532 = CARTESIAN_POINT ( 'NONE',  ( 0.1856180156872625775, -0.8149015557553581646, 0.1814193148890651530 ) ) ;
#13533 = CARTESIAN_POINT ( 'NONE',  ( 5.463695987328526437E-16, -0.2899999999999993694, -7.171100983368691195E-16 ) ) ;
#13534 = ADVANCED_FACE ( 'NONE', ( #10983 ), #1327, .F. ) ;
#13535 = CARTESIAN_POINT ( 'NONE',  ( 0.3486350902747559211, -1.743989531435688356, 0.6021158924634461007 ) ) ;
#13536 = CARTESIAN_POINT ( 'NONE',  ( 0.08861793153380866095, -0.6435352693684576186, 0.1047593608519658409 ) ) ;
#13537 = AXIS2_PLACEMENT_3D ( 'NONE', #969, #18858, #3203 ) ;
#13538 = CARTESIAN_POINT ( 'NONE',  ( 0.6630438016670622270, -1.374754038922163080, 0.8377997132616019638 ) ) ;
#13539 = CARTESIAN_POINT ( 'NONE',  ( 0.3929588477770515342, -1.748770905532780473, -0.7163146028298593704 ) ) ;
#13540 = DIRECTION ( 'NONE',  ( 0.8660512985181126888, 0.4999551463232385085, 0.000000000000000000 ) ) ;
#13541 = CARTESIAN_POINT ( 'NONE',  ( 0.02231181081520646273, -0.3551561381230135539, -0.3696296485972559998 ) ) ;
#13542 = CALENDAR_DATE ( 2026, 13, 10 ) ;
#13543 = LOCAL_TIME ( 0, 53, 7.000000000000000000, #28434 ) ;
#13544 = CARTESIAN_POINT ( 'NONE',  ( 0.6378390993400826492, -1.514931934295542293, -0.6154632752815170083 ) ) ;
#13545 = CARTESIAN_POINT ( 'NONE',  ( 0.02872242845530408734, 0.3729171224323689082, 0.3802687114177492056 ) ) ;
#13546 = CARTESIAN_POINT ( 'NONE',  ( 0.1847276542582137193, -0.6567261035475721043, -0.02741476136339842176 ) ) ;
#13547 = CARTESIAN_POINT ( 'NONE',  ( 0.4470752049162848851, -1.224679863139781721, 0.4807434620714813311 ) ) ;
#13548 = CARTESIAN_POINT ( 'NONE',  ( -0.3000000000000000999, -3.758594918004649621, -0.06617323996463192470 ) ) ;
#13549 = CARTESIAN_POINT ( 'NONE',  ( 0.2474040834808491629, -1.657462368044302137, 0.5682417262808785452 ) ) ;
#13550 = CARTESIAN_POINT ( 'NONE',  ( 0.6107159011204299492, -1.503447172704659884, -0.4209194897869562579 ) ) ;
#13551 = EDGE_CURVE ( 'NONE', #15736, #27340, #20254, .T. ) ;
#13552 = DIRECTION ( 'NONE',  ( -7.000205099780314469E-17, -1.000000000000000000, 6.590151126658399604E-16 ) ) ;
#13553 = CARTESIAN_POINT ( 'NONE',  ( 0.5578464603247045295, -1.622583067024152115, -0.5578993484895078403 ) ) ;
#13554 = DIRECTION ( 'NONE',  ( 0.4999551463232372317, -0.8660512985181134660, 0.000000000000000000 ) ) ;
#13555 = EDGE_CURVE ( 'NONE', #23581, #38697, #23308, .T. ) ;
#13556 = VERTEX_POINT ( 'NONE', #36252 ) ;
#13557 = ORIENTED_EDGE ( 'NONE', *, *, #10233, .F. ) ;
#13558 = EDGE_CURVE ( 'NONE', #36582, #4130, #35444, .T. ) ;
#13559 = CARTESIAN_POINT ( 'NONE',  ( 0.03309057659885102087, -0.2303206601891079897, -0.4671007096900161581 ) ) ;
#13560 = ORIENTED_EDGE ( 'NONE', *, *, #28330, .T. ) ;
#13561 = CARTESIAN_POINT ( 'NONE',  ( -0.02231181081520790255, -0.07006449514257452604, 0.5077922075898742005 ) ) ;
#13562 = CARTESIAN_POINT ( 'NONE',  ( 0.5960491110230784484, -1.583590495288289102, -0.4275273839149444366 ) ) ;
#13563 = CARTESIAN_POINT ( 'NONE',  ( 0.5249339888458012249, -1.337369657638982634, 0.7530580798306065748 ) ) ;
#13565 = ORIENTED_EDGE ( 'NONE', *, *, #19810, .F. ) ;
#13564 = CARTESIAN_POINT ( 'NONE',  ( 0.5668224073227418058, -1.626940512309301257, 0.5103467090509832271 ) ) ;
#13566 = CARTESIAN_POINT ( 'NONE',  ( 0.4529286794724542986, -1.051290237540063455, 0.7432202178062045084 ) ) ;
#13567 = CARTESIAN_POINT ( 'NONE',  ( 0.3837205613235070145, -1.661390420354927899, -0.6156094881597907742 ) ) ;
#13568 = EDGE_LOOP ( 'NONE', ( #38090, #25385, #1098, #5541 ) ) ;
#13569 = AXIS2_PLACEMENT_3D ( 'NONE', #21015, #17312, #30472 ) ;
#13570 = CARTESIAN_POINT ( 'NONE',  ( 0.2499757726471207031, -1.165244724628914375, -0.5155029497116575543 ) ) ;
#13571 = VERTEX_POINT ( 'NONE', #29293 ) ;
#13572 = CARTESIAN_POINT ( 'NONE',  ( 0.2891949312394517801, -1.508234465259375767, 0.8769322456029351454 ) ) ;
#13574 = CARTESIAN_POINT ( 'NONE',  ( -0.03158843595483515343, -0.2432919444504221540, 0.4277514783322121650 ) ) ;
#13573 = CARTESIAN_POINT ( 'NONE',  ( -0.1508044614562676355, 0.4665164580004940720, 0.3602693336111434941 ) ) ;
#13575 = CARTESIAN_POINT ( 'NONE',  ( -0.2399999999999999079, -1.891808285041389093, -0.4498908273618595910 ) ) ;
#13576 = LOCAL_TIME ( 0, 53, 7.000000000000000000, #908 ) ;
#13577 = CARTESIAN_POINT ( 'NONE',  ( -0.2267371898560524290, -0.4872893062166330780, 0.09999999999999989453 ) ) ;
#13578 = EDGE_LOOP ( 'NONE', ( #35820, #15425, #26058, #23044, #28276 ) ) ;
#13579 = DIRECTION ( 'NONE',  ( -2.218671295934093951E-31, -0.6954292836768477537, 0.7185945389471773970 ) ) ;
#13580 = AXIS2_PLACEMENT_3D ( 'NONE', #15912, #331, #12835 ) ;
#13581 = CARTESIAN_POINT ( 'NONE',  ( 0.1109049718728864486, -0.9286333055842306283, 0.1449575636331430772 ) ) ;
#13582 = CARTESIAN_POINT ( 'NONE',  ( -0.01548846960707477016, 0.3880410510314737382, -0.3755318131855000519 ) ) ;
#13583 = CARTESIAN_POINT ( 'NONE',  ( -2.128333683970191216E-14, -2.097675824466503691, -0.2907100122647986451 ) ) ;
#13584 = CARTESIAN_POINT ( 'NONE',  ( 0.1132625840440346782, -0.8395474731811463087, 0.3484180331796957741 ) ) ;
#13585 = CARTESIAN_POINT ( 'NONE',  ( 0.01056122778382778161, -0.5298774523167767425, 0.1553095696234600420 ) ) ;
#13586 = ADVANCED_FACE ( 'NONE', ( #13640 ), #22955, .F. ) ;
#13587 = CARTESIAN_POINT ( 'NONE',  ( 0.000000000000000000, 0.000000000000000000, 0.000000000000000000 ) ) ;
#13588 = DIRECTION ( 'NONE',  ( 0.4999551463232377313, -0.8660512985181132439, -0.000000000000000000 ) ) ;
#13589 = DIRECTION ( 'NONE',  ( 0.8660512985181134660, 0.4999551463232373427, 0.000000000000000000 ) ) ;
#13590 = DIRECTION ( 'NONE',  ( 1.000000000000000000, -0.000000000000000000, -0.000000000000000000 ) ) ;
#13591 = CARTESIAN_POINT ( 'NONE',  ( 0.3259879919982042185, -1.767950897709266611, 0.5312986935552648227 ) ) ;
#13592 = APPROVAL_ROLE ( '' ) ;
#13593 = AXIS2_PLACEMENT_3D ( 'NONE', #24534, #12789, #27612 ) ;
#13594 = CARTESIAN_POINT ( 'NONE',  ( 0.05999999999999990757, 0.000000000000000000, 0.000000000000000000 ) ) ;
#13595 = CARTESIAN_POINT ( 'NONE',  ( 0.1806271871886622193, -0.4979126063066979802, 0.1191298491398793680 ) ) ;
#13596 = CARTESIAN_POINT ( 'NONE',  ( 0.2059273467974227778, -1.283046334493782359, -0.7137159211901564770 ) ) ;
#13597 = APPROVAL_PERSON_ORGANIZATION ( #22900, #37929, #32317 ) ;
#13598 = LINE ( 'NONE', #20377, #15976 ) ;
#13599 = CARTESIAN_POINT ( 'NONE',  ( 0.4113341154505090747, -1.741801871956848657, -0.5994564538100538575 ) ) ;
#13600 = CARTESIAN_POINT ( 'NONE',  ( 0.2856903115327851239, -1.612432775839717225, 0.9415318914171060261 ) ) ;
#13601 = CARTESIAN_POINT ( 'NONE',  ( 0.000000000000000000, 0.000000000000000000, 0.000000000000000000 ) ) ;
#13602 = CARTESIAN_POINT ( 'NONE',  ( -2.070754768975508586, -0.09959325338431662678, 0.3600000000000021516 ) ) ;
#13603 = ORIENTED_EDGE ( 'NONE', *, *, #2706, .F. ) ;
#13604 = CYLINDRICAL_SURFACE ( 'NONE', #5262, 0.1000000000000000194 ) ;
#13605 = CARTESIAN_POINT ( 'NONE',  ( 0.5764473935400443727, -1.446560465971904463, 0.7291923036817888892 ) ) ;
#13607 = EDGE_LOOP ( 'NONE', ( #27791, #20278, #7171, #10118 ) ) ;
#13606 = CARTESIAN_POINT ( 'NONE',  ( 0.4879569794952549056, -1.656586030313209168, -0.4238502451869202159 ) ) ;
#13609 = ORIENTED_EDGE ( 'NONE', *, *, #8114, .T. ) ;
#13608 = VERTEX_POINT ( 'NONE', #2331 ) ;
#13610 = CARTESIAN_POINT ( 'NONE',  ( 0.5863399829793073392, -1.370111929318044597, 0.8757726842784098187 ) ) ;
#13611 = ORIENTED_EDGE ( 'NONE', *, *, #40315, .T. ) ;
#13612 = ORIENTED_EDGE ( 'NONE', *, *, #27855, .T. ) ;
#13613 = CARTESIAN_POINT ( 'NONE',  ( -0.007799093721804064433, -0.6030369617549071748, 0.3865317856287898146 ) ) ;
#13614 = CARTESIAN_POINT ( 'NONE',  ( 0.3999999999999787059, -2.097675824466503691, -0.7286991843995640483 ) ) ;
#13615 = CARTESIAN_POINT ( 'NONE',  ( -0.002000607657151622348, -0.7404579356088996089, -0.01138449076159512782 ) ) ;
#13616 = EDGE_LOOP ( 'NONE', ( #2681, #19331, #27929, #28702 ) ) ;
#13617 = CARTESIAN_POINT ( 'NONE',  ( 0.08970085000315114465, -0.8164246713187256477, 0.2562084196594314744 ) ) ;
#13618 = CARTESIAN_POINT ( 'NONE',  ( 0.3637049059787201832, -1.760756476090657330, -0.5110479723366356808 ) ) ;
#13619 = CARTESIAN_POINT ( 'NONE',  ( 0.1100478739389431776, -0.5471989581415684922, 0.1457185332388694632 ) ) ;
#13620 = CARTESIAN_POINT ( 'NONE',  ( 0.06720200293959881221, -1.311493277772410426, 0.6073410707387120189 ) ) ;
#13621 = CARTESIAN_POINT ( 'NONE',  ( 0.4573071940129567747, -1.592216967606236544, -0.4275647618858054999 ) ) ;
#13622 = CARTESIAN_POINT ( 'NONE',  ( 2.762449479338929480E-16, -0.05999999999999978961, 0.1849999999999999978 ) ) ;
#13623 = CARTESIAN_POINT ( 'NONE',  ( 0.3650261032261186700, -1.734273230346309091, 0.6015988091205355381 ) ) ;
#13624 = CARTESIAN_POINT ( 'NONE',  ( 0.3511758406044659386, -1.510956930971388834, -0.7187326247832951376 ) ) ;
#13625 = CARTESIAN_POINT ( 'NONE',  ( 0.5001189568028716614, -1.586255355638424236, -0.5583759577945262009 ) ) ;
#13626 = CARTESIAN_POINT ( 'NONE',  ( 0.3135533596100509857, -1.751749968712532635, 0.5597833863612885485 ) ) ;
#13627 = CARTESIAN_POINT ( 'NONE',  ( -0.02000000000000000042, -1.622350287959229087, -0.08960079202753243321 ) ) ;
#13628 = CARTESIAN_POINT ( 'NONE',  ( -2.158236442226783958E-06, -0.7557589808029421263, -0.1062375170323252432 ) ) ;
#13629 = CARTESIAN_POINT ( 'NONE',  ( 0.06952717988241019498, -0.5442879774309438146, 0.1846901343294024000 ) ) ;
#13630 = CARTESIAN_POINT ( 'NONE',  ( 0.007573306818223588845, -0.7572691898189487514, 0.003620172530112310012 ) ) ;
#13631 = CARTESIAN_POINT ( 'NONE',  ( 0.4484878740865431146, -1.108380718066777959, -0.3648515278348753443 ) ) ;
#13632 = CARTESIAN_POINT ( 'NONE',  ( 0.01266180416972241714, -0.9102398499036795654, 0.5581420674395337622 ) ) ;
#13633 = CARTESIAN_POINT ( 'NONE',  ( 0.4638997371337593156, -1.067608878195758448, 0.6494661525283214054 ) ) ;
#13634 = SHAPE_DEFINITION_REPRESENTATION ( #22606, #21742 ) ;
#13635 = CYLINDRICAL_SURFACE ( 'NONE', #16244, 0.2500000000000000000 ) ;
#13636 = CARTESIAN_POINT ( 'NONE',  ( 0.3187814993714178091, -1.760346054620885781, 0.5688112331864385585 ) ) ;
#13637 = ORIENTED_EDGE ( 'NONE', *, *, #38119, .T. ) ;
#13638 = CARTESIAN_POINT ( 'NONE',  ( 0.4465857567753348523, -1.571616349952935643, 0.6043008826171946124 ) ) ;
#13639 = CARTESIAN_POINT ( 'NONE',  ( 0.01075032470689779758, -0.5446343802999467076, 0.2276730487650680257 ) ) ;
#13640 = FACE_OUTER_BOUND ( 'NONE', #31374, .T. ) ;
#13641 = ORIENTED_EDGE ( 'NONE', *, *, #33119, .T. ) ;
#13642 = CARTESIAN_POINT ( 'NONE',  ( 0.1859432605888821921, -0.7573098151843028480, 0.1022962920937455361 ) ) ;
#13643 = EDGE_CURVE ( 'NONE', #25669, #36006, #24707, .T. ) ;
#13644 = ADVANCED_FACE ( 'NONE', ( #26755 ), #23056, .F. ) ;
#13645 = CARTESIAN_POINT ( 'NONE',  ( 0.2033263846434442690, -0.5675993867538808857, 0.3776288918835234987 ) ) ;
#13647 = ORIENTED_EDGE ( 'NONE', *, *, #30157, .F. ) ;
#13646 = ORIENTED_EDGE ( 'NONE', *, *, #25007, .T. ) ;
#13648 = FACE_OUTER_BOUND ( 'NONE', #28561, .T. ) ;
#13649 = CARTESIAN_POINT ( 'NONE',  ( 0.6590705178848084156, -1.601721441849921268, 0.5182417262812423209 ) ) ;
#13650 = CARTESIAN_POINT ( 'NONE',  ( 0.3993510570514907099, -1.686034264335497301, -0.5196087884962241610 ) ) ;
#13651 = EDGE_CURVE ( 'NONE', #5233, #34649, #23665, .T. ) ;
#13652 = CARTESIAN_POINT ( 'NONE',  ( -0.05615703521554947508, 0.4399943745474728107, -0.1321275321584859941 ) ) ;
#13653 = ORIENTED_EDGE ( 'NONE', *, *, #9941, .F. ) ;
#13654 = CARTESIAN_POINT ( 'NONE',  ( 0.3480299946200001715, -1.742528658578555989, 0.5682417262808788783 ) ) ;
#13655 = EDGE_CURVE ( 'NONE', #1334, #15898, #36189, .T. ) ;
#13656 = CARTESIAN_POINT ( 'NONE',  ( 0.2421733343592223919, -0.9179996579516339628, 0.6933330327357866141 ) ) ;
#13657 = CARTESIAN_POINT ( 'NONE',  ( 0.01846853196186494517, -0.5817156171557603672, 0.5516149763055392397 ) ) ;
#13658 = CARTESIAN_POINT ( 'NONE',  ( 0.4689754774150589056, -1.557726810111841775, 0.5609945539710509133 ) ) ;
#13660 = CARTESIAN_POINT ( 'NONE',  ( 0.3511758406044653280, -1.510956930971387724, -0.7187326247832955817 ) ) ;
#13659 = CARTESIAN_POINT ( 'NONE',  ( 0.2713590513584660524, -1.676816687660336758, 0.7035140810151785384 ) ) ;
#13661 = CARTESIAN_POINT ( 'NONE',  ( 0.2181072496379036219, -0.9917094513883838447, 0.5584457447843073075 ) ) ;
#13662 = ORIENTED_EDGE ( 'NONE', *, *, #26536, .T. ) ;
#13663 = VERTEX_POINT ( 'NONE', #35587 ) ;
#13664 = CARTESIAN_POINT ( 'NONE',  ( 0.2127800765133925076, -1.279090382353622601, -0.3161890964247149327 ) ) ;
#13665 = CARTESIAN_POINT ( 'NONE',  ( 0.1967274779738960033, -0.6939718894208231070, 0.6484394435625246977 ) ) ;
#13666 = CARTESIAN_POINT ( 'NONE',  ( -0.04047161733260026123, 0.2415827978909600438, -0.4392067210493235119 ) ) ;
#13667 = EDGE_CURVE ( 'NONE', #38406, #28968, #13775, .T. ) ;
#13668 = APPLIED_PERSON_AND_ORGANIZATION_ASSIGNMENT ( #30889, #15470, ( #29493 ) ) ;
#13669 = B_SPLINE_CURVE_WITH_KNOTS ( 'NONE', 3,
 ( #7680, #20244, #14258, #26821, #11171, #23727, #36255, #11373 ),
 .UNSPECIFIED., .F., .F.,
 ( 4, 2, 2, 4 ),
 ( 2.350980519545030896E-07, 0.001838925622864765559, 0.002758270885271171206, 0.003677616147677576636 ),
 .UNSPECIFIED. ) ;
#13670 = CARTESIAN_POINT ( 'NONE',  ( -0.04211471441534220955, -0.4433427331037121388, -0.1530948108196634461 ) ) ;
#13671 = DIRECTION ( 'NONE',  ( 0.000000000000000000, -2.294752314677981182E-14, -1.000000000000000000 ) ) ;
#13672 = AXIS2_PLACEMENT_3D ( 'NONE', #39226, #27079, #39612 ) ;
#13673 = DIRECTION ( 'NONE',  ( -1.000000000000000000, 0.000000000000000000, -7.762644838731319154E-16 ) ) ;
#13674 = CARTESIAN_POINT ( 'NONE',  ( 0.3857344834571298509, -0.9392921734164567660, 0.7474990102649032853 ) ) ;
#13675 = CARTESIAN_POINT ( 'NONE',  ( 0.4393445808683661413, -1.126265756603593182, 0.4785818640455667961 ) ) ;
#13676 = CARTESIAN_POINT ( 'NONE',  ( 0.06846619564075531739, -1.327627092167478873, 0.5756175524039078839 ) ) ;
#13677 = CARTESIAN_POINT ( 'NONE',  ( 0.04229974373173322338, 0.4430055847546675585, -0.1530238331097760751 ) ) ;
#13678 = CARTESIAN_POINT ( 'NONE',  ( 0.5195269094232773943, -1.645577264492883884, -0.5790482453853514899 ) ) ;
#13679 = ORIENTED_EDGE ( 'NONE', *, *, #22792, .T. ) ;
#13680 = CARTESIAN_POINT ( 'NONE',  ( 0.3952148919761621637, -1.141712405902378435, 0.7491518327547966871 ) ) ;
#13681 = CARTESIAN_POINT ( 'NONE',  ( 0.2683831008096893567, -1.674238039577110593, 0.5753345947181904840 ) ) ;
#13682 = CARTESIAN_POINT ( 'NONE',  ( -0.03642997641689347393, -0.2291049489869416145, -0.4577964116453033805 ) ) ;
#13683 = ORIENTED_EDGE ( 'NONE', *, *, #14696, .F. ) ;
#13684 = FACE_OUTER_BOUND ( 'NONE', #5710, .T. ) ;
#13685 = ORIENTED_EDGE ( 'NONE', *, *, #26303, .F. ) ;
#13686 = CARTESIAN_POINT ( 'NONE',  ( 0.09000415367089972807, -0.5660392021805559226, 0.1654146037094502697 ) ) ;
#13687 = CARTESIAN_POINT ( 'NONE',  ( 0.7255201985491259720, -1.551814629293185366, 0.5182417262812423209 ) ) ;
#13688 = CARTESIAN_POINT ( 'NONE',  ( 0.4233039937489216364, -1.123485956316199186, 0.5460366295032810235 ) ) ;
#13689 = CARTESIAN_POINT ( 'NONE',  ( 0.2388530902294009883, -1.245845591994676926, 0.7174669630728713887 ) ) ;
#13690 = ORIENTED_EDGE ( 'NONE', *, *, #36768, .T. ) ;
#13691 = EDGE_CURVE ( 'NONE', #26169, #17298, #7529, .T. ) ;
#13692 = CARTESIAN_POINT ( 'NONE',  ( -0.1642263573063267590, 0.5103503758723633155, 0.3090632479873802740 ) ) ;
#13693 = CARTESIAN_POINT ( 'NONE',  ( 0.01899496522504069002, 0.07377983897468347319, 0.5147126279162671514 ) ) ;
#13694 = CARTESIAN_POINT ( 'NONE',  ( 0.3991299184228387920, -1.748847125651597390, -0.4900826320043861206 ) ) ;
#13695 = EDGE_CURVE ( 'NONE', #34438, #14824, #8001, .T. ) ;
#13696 = CARTESIAN_POINT ( 'NONE',  ( 0.4637507040111739087, -1.233505390051135242, 0.6717282244380275991 ) ) ;
#13698 = CARTESIAN_POINT ( 'NONE',  ( 0.3116392842230071292, -1.763036623927723978, 0.5305946302528894432 ) ) ;
#13697 = CARTESIAN_POINT ( 'NONE',  ( -0.02000000000000000042, -2.320036485105098301, -0.2941690811493925528 ) ) ;
#13699 = CARTESIAN_POINT ( 'NONE',  ( 0.5788429232882181807, -1.529988839563255709, -0.4632948810236542370 ) ) ;
#13700 = VERTEX_POINT ( 'NONE', #17276 ) ;
#13701 = ADVANCED_FACE ( 'NONE', ( #27153 ), #375, .T. ) ;
#13702 = CARTESIAN_POINT ( 'NONE',  ( -0.1530296545635675409, 0.4740172026173952724, 0.3600612075995228700 ) ) ;
#13703 = ORIENTED_EDGE ( 'NONE', *, *, #876, .T. ) ;
#13704 = CARTESIAN_POINT ( 'NONE',  ( 0.04921512002571602068, -0.5620675706429341112, 0.2577714020897228786 ) ) ;
#13706 = CARTESIAN_POINT ( 'NONE',  ( 0.2024211440586259347, -0.7203912786704501636, 0.3419443000676659628 ) ) ;
#13705 = CARTESIAN_POINT ( 'NONE',  ( 0.08725757351828516972, -0.7039266628255411717, 0.02354379185445030359 ) ) ;
#13707 = CARTESIAN_POINT ( 'NONE',  ( 0.2341860847041785376, -1.597289339054992263, -0.3541232024024360547 ) ) ;
#13708 = ORIENTED_EDGE ( 'NONE', *, *, #6447, .F. ) ;
#13709 = ORIENTED_EDGE ( 'NONE', *, *, #23324, .F. ) ;
#13710 = DIRECTION ( 'NONE',  ( 0.000000000000000000, -0.9343694307158671997, 0.3563057211773427713 ) ) ;
#13711 = CARTESIAN_POINT ( 'NONE',  ( 0.1650742144947170698, -0.7251586625020333132, 0.5326188692438563743 ) ) ;
#13712 = VERTEX_POINT ( 'NONE', #5116 ) ;
#13713 = CARTESIAN_POINT ( 'NONE',  ( 0.3852571783543742301, -1.799609661962979112, -0.5248174630631543547 ) ) ;
#13714 = CARTESIAN_POINT ( 'NONE',  ( 0.05268932808080010327, -0.4428506128075276882, 0.1535014714533977642 ) ) ;
#13715 = EDGE_CURVE ( 'NONE', #22890, #8281, #23337, .T. ) ;
#13716 = CARTESIAN_POINT ( 'NONE',  ( 0.4032069153717364740, -1.732084460174936780, -0.4324387111440983200 ) ) ;
#13717 = PRODUCT_DEFINITION_SHAPE ( 'NONE', 'NONE',  #37836 ) ;
#13718 = CARTESIAN_POINT ( 'NONE',  ( 0.1991599691044491915, -1.252086681028342863, 0.4385478258677236729 ) ) ;
#13719 = CARTESIAN_POINT ( 'NONE',  ( 0.4741105259895962432, -1.670573610379107787, 0.5762220851322598092 ) ) ;
#13720 = CARTESIAN_POINT ( 'NONE',  ( 0.05634304521267756438, -0.01028134608269219187, 0.4588823192046725397 ) ) ;
#13721 = CARTESIAN_POINT ( 'NONE',  ( 0.7435985525077578595, -1.513373960891965186, 0.6163350003740883931 ) ) ;
#13722 = DIRECTION ( 'NONE',  ( 1.000000000000000000, -0.000000000000000000, -0.000000000000000000 ) ) ;
#13723 = CARTESIAN_POINT ( 'NONE',  ( -0.2399999999999999079, -3.672249662662566472, -0.1880352225538197142 ) ) ;
#13724 = PRODUCT_CONTEXT ( 'NONE', #26376, 'mechanical' ) ;
#13725 = CARTESIAN_POINT ( 'NONE',  ( 0.4159916692016358830, -1.069406866067976081, -0.5155029497116575543 ) ) ;
#13726 = CARTESIAN_POINT ( 'NONE',  ( 0.04229974373173651936, 0.2824305679197209873, 0.3740363831607525502 ) ) ;
#13727 = CARTESIAN_POINT ( 'NONE',  ( -0.1211759891752648838, -0.5069122841110333955, 0.3093762286737390954 ) ) ;
#13728 = FACE_OUTER_BOUND ( 'NONE', #12489, .T. ) ;
#13729 = CARTESIAN_POINT ( 'NONE',  ( -0.02953079040095652960, 0.5250338024619264354, -0.07436286310882528339 ) ) ;
#13730 = CARTESIAN_POINT ( 'NONE',  ( 0.1023011615166706662, -1.050388104772951969, 0.8771683563204210055 ) ) ;
#13731 = CARTESIAN_POINT ( 'NONE',  ( 0.5758566523281927196, -1.538448204759498283, -0.4771555642015232190 ) ) ;
#13732 = DIRECTION ( 'NONE',  ( -1.387778780781449423E-15, 6.590151126658376924E-16, -1.000000000000000000 ) ) ;
#13733 = B_SPLINE_CURVE_WITH_KNOTS ( 'NONE', 3,
 ( #32811, #14305, #17189, #27062, #20484, #26676, #2378, #27475, #17787, #33018, #24194, #33232, #40000, #11217, #5040, #36717, #14920, #4823 ),
 .UNSPECIFIED., .F., .F.,
 ( 4, 2, 2, 2, 2, 2, 2, 2, 4 ),
 ( -0.002633528389679732490, -0.001975271857855729826, -0.001317015326031727163, -0.0006587587942077244990, -5.022623837218354037E-07, 0.0006577542694402808282, 0.001316010801264283492, 0.001974267333088286155, 0.002632523864912288819 ),
 .UNSPECIFIED. ) ;
#13734 = DIRECTION ( 'NONE',  ( 0.9998941247116547304, -0.01455087607601020412, 0.0001066420868422379633 ) ) ;
#13735 = CARTESIAN_POINT ( 'NONE',  ( -0.02238765564325098656, -0.3549921663302747499, 0.3695537732572988232 ) ) ;
#13736 =( REPRESENTATION_RELATIONSHIP ('NONE','NONE', #33020, #30390 ) REPRESENTATION_RELATIONSHIP_WITH_TRANSFORMATION ( #30865 )SHAPE_REPRESENTATION_RELATIONSHIP( ) );
#13737 = VERTEX_POINT ( 'NONE', #4510 ) ;
#13738 = ORIENTED_EDGE ( 'NONE', *, *, #24733, .F. ) ;
#13739 = EDGE_CURVE ( 'NONE', #4078, #22774, #25951, .T. ) ;
#13740 = CARTESIAN_POINT ( 'NONE',  ( 0.3686476870012108109, -1.763285233157189769, -0.5845549610680257357 ) ) ;
#13741 = ORIENTED_EDGE ( 'NONE', *, *, #5635, .T. ) ;
#13742 = CARTESIAN_POINT ( 'NONE',  ( 0.05999999999999990757, -0.2793841226333812489, -0.1799682156082512696 ) ) ;
#13743 = CARTESIAN_POINT ( 'NONE',  ( 0.03113248654051816583, 0.5632502439596359656, -0.2139757610878384453 ) ) ;
#13744 = ADVANCED_FACE ( 'NONE', ( #1271 ), #29868, .T. ) ;
#13745 = CARTESIAN_POINT ( 'NONE',  ( 0.5475879855805122487, -1.373140497242092195, 0.6594375008024977447 ) ) ;
#13747 = ORIENTED_EDGE ( 'NONE', *, *, #31499, .F. ) ;
#13746 = CARTESIAN_POINT ( 'NONE',  ( -0.05283710938261119983, 0.4560492058803807813, 0.1064717188025598449 ) ) ;
#13748 = CARTESIAN_POINT ( 'NONE',  ( 0.3465599992496842807, -0.9476710551646405634, 0.6409924101657002993 ) ) ;
#13749 = EDGE_CURVE ( 'NONE', #1246, #22420, #6016, .T. ) ;
#13750 = CARTESIAN_POINT ( 'NONE',  ( 0.03654364704248846962, 0.5058694728073472868, -0.07650507870001040100 ) ) ;
#13751 = VERTEX_POINT ( 'NONE', #4917 ) ;
#13752 = DIRECTION ( 'NONE',  ( -0.1858595909941318236, -0.1072932506077262926, 0.9767007580674449407 ) ) ;
#13753 = ORIENTED_EDGE ( 'NONE', *, *, #35811, .T. ) ;
#13754 = CARTESIAN_POINT ( 'NONE',  ( 0.02432663359975386838, -0.5586419101762778450, 0.2615263354939962870 ) ) ;
#13756 = CARTESIAN_POINT ( 'NONE',  ( 0.1124368596819388111, -0.7940650780295996913, -0.07060698127412667890 ) ) ;
#13755 = CARTESIAN_POINT ( 'NONE',  ( 0.5388754901600865121, -1.668174632133634816, -0.4628410262239764372 ) ) ;
#13757 = DIRECTION ( 'NONE',  ( 1.000000000000000000, 0.000000000000000000, 0.000000000000000000 ) ) ;
#13758 = EDGE_CURVE ( 'NONE', #20946, #13015, #18052, .T. ) ;
#13759 = CARTESIAN_POINT ( 'NONE',  ( 0.009883767140662630749, -1.737539166105977362, -0.3362136773710249216 ) ) ;
#13760 = ORIENTED_EDGE ( 'NONE', *, *, #24119, .T. ) ;
#13761 = CARTESIAN_POINT ( 'NONE',  ( -0.2746410161513770931, -2.878813263491020180, -0.3823467908819087602 ) ) ;
#13762 = CARTESIAN_POINT ( 'NONE',  ( 0.2002687484916081118, -0.9229665737500837297, 0.3245110103503117682 ) ) ;
#13763 = CARTESIAN_POINT ( 'NONE',  ( 0.1241546671216074288, -1.317368862021473186, -0.6849612450614390724 ) ) ;
#13764 = DIRECTION ( 'NONE',  ( 0.000000000000000000, 0.000000000000000000, 1.000000000000000000 ) ) ;
#13765 = EDGE_CURVE ( 'NONE', #19084, #33509, #1863, .T. ) ;
#13766 = CARTESIAN_POINT ( 'NONE',  ( 0.2543894466873252158, -1.055563264917066091, 0.7376352696996288927 ) ) ;
#13767 = CARTESIAN_POINT ( 'NONE',  ( 0.04703489300812706275, -0.8021760332774975355, 0.6694782157141636603 ) ) ;
#13768 = EDGE_CURVE ( 'NONE', #13895, #27138, #6846, .T. ) ;
#13769 = DIRECTION ( 'NONE',  ( -8.881784197001246407E-16, 2.361472542561082612E-16, -1.000000000000000000 ) ) ;
#13770 = EDGE_CURVE ( 'NONE', #13940, #2287, #26587, .T. ) ;
#13771 = CARTESIAN_POINT ( 'NONE',  ( -0.1659631349965107749, 0.5156080474714448414, 0.3322463110352368298 ) ) ;
#13772 = CARTESIAN_POINT ( 'NONE',  ( -0.1157923916714435481, -0.5295015842440792264, 0.1380392329925451689 ) ) ;
#13773 = CARTESIAN_POINT ( 'NONE',  ( 0.05283102792148713922, 0.4560693389104583662, 0.1064538768721982470 ) ) ;
#13774 = CARTESIAN_POINT ( 'NONE',  ( 0.3999999999999787059, -2.183180860297921466, -0.4937760292030871079 ) ) ;
#13775 = LINE ( 'NONE', #1463, #31833 ) ;
#13776 = APPROVAL_DATE_TIME ( #20373, #40085 ) ;
#13777 = CARTESIAN_POINT ( 'NONE',  ( 0.02521977883247775859, -1.088411770194798178, 0.6474433479578449724 ) ) ;
#13778 = CARTESIAN_POINT ( 'NONE',  ( 0.1774972420046788679, -0.4900154790703133423, 0.1409049844863272671 ) ) ;
#13779 = PRODUCT_DEFINITION_CONTEXT ( 'detailed design', #38439, 'design' ) ;
#13780 = CARTESIAN_POINT ( 'NONE',  ( 0.5762321503990789351, -1.646609333902588235, -0.4868944820179721966 ) ) ;
#13781 = CARTESIAN_POINT ( 'NONE',  ( -0.08000000000000000167, -2.631664041040912227, -0.5119035495255163104 ) ) ;
#13782 = CARTESIAN_POINT ( 'NONE',  ( 0.3918182118607624331, -1.107073211027153725, 0.6042946153017959565 ) ) ;
#13783 = FACE_OUTER_BOUND ( 'NONE', #5446, .T. ) ;
#13784 = CARTESIAN_POINT ( 'NONE',  ( 0.02869712619511936846, 0.06034133159976078770, -0.4947855140619924486 ) ) ;
#13785 = VERTEX_POINT ( 'NONE', #20788 ) ;
#13786 = CARTESIAN_POINT ( 'NONE',  ( 0.1778984696810832766, -0.5443775716742050852, 0.2437360553562945842 ) ) ;
#13787 = ORIENTED_EDGE ( 'NONE', *, *, #34096, .T. ) ;
#13788 = CARTESIAN_POINT ( 'NONE',  ( 0.2592175946368545092, -1.678678769766079881, 0.5610528864763278944 ) ) ;
#13789 = EDGE_CURVE ( 'NONE', #33249, #7589, #16106, .T. ) ;
#13790 = CARTESIAN_POINT ( 'NONE',  ( 0.5409705397755507628, -1.398922715619407064, 0.7775598356702776437 ) ) ;
#13792 = ORIENTED_EDGE ( 'NONE', *, *, #14959, .T. ) ;
#13791 = DIRECTION ( 'NONE',  ( 0.000000000000000000, 1.951319995474463472E-15, -1.000000000000000000 ) ) ;
#13793 = EDGE_CURVE ( 'NONE', #13990, #1334, #37760, .T. ) ;
#13795 = ORIENTED_EDGE ( 'NONE', *, *, #9986, .T. ) ;
#13794 = VERTEX_POINT ( 'NONE', #31258 ) ;
#13796 = CARTESIAN_POINT ( 'NONE',  ( 0.4790210037517146358, -1.178264979292966252, 0.8995276976856623197 ) ) ;
#13797 =( BOUNDED_SURFACE ( )  B_SPLINE_SURFACE ( 3, 2, ( 
 ( #8046, #24518, #18334 ),
 ( #8652, #5573, #2090 ),
 ( #36233, #8869, #24128 ),
 ( #20622, #39937, #27411 ),
 ( #36650, #8454, #14418 ),
 ( #11954, #33158, #18133 ),
 ( #33542, #36446, #21223 ),
 ( #5352, #2697, #2507 ),
 ( #21447, #15047, #33974 ),
 ( #15245, #32439, #4262 ) ),
 .UNSPECIFIED., .F., .F., .T. ) 
 B_SPLINE_SURFACE_WITH_KNOTS ( ( 4, 2, 2, 2, 4 ),
 ( 3, 3 ),
 ( 0.0007861888542779920438, 0.001094194827383940163, 0.001402200800489888498, 0.001710206773595836617, 0.002018212746701784736 ),
 ( 0.000000000000000000, 0.6753453643475422208 ),
 .UNSPECIFIED. ) 
 GEOMETRIC_REPRESENTATION_ITEM ( )  RATIONAL_B_SPLINE_SURFACE ( (
 ( 1.000000000000000000, 0.7938099847028182721, 0.8661189114170375625),
 ( 1.000000000000000000, 0.8158720960386478538, 0.8804440448519528228),
 ( 1.000000000000000000, 0.8317178396726564449, 0.8907328331042354552),
 ( 1.000000000000000000, 0.8529323147884961820, 0.9045075884828177593),
 ( 1.000000000000000000, 0.8583035682245675480, 0.9079951931373873020),
 ( 1.000000000000000000, 0.8588125958609250654, 0.9083257095010246474),
 ( 1.000000000000000000, 0.8539403388225746960, 0.9051621078338429882),
 ( 1.000000000000000000, 0.8338631590414414818, 0.8921258088602976866),
 ( 1.000000000000000000, 0.8186530614390943317, 0.8822497514696410192),
 ( 1.000000000000000000, 0.7974297740311802052, 0.8684692741881134825) ) ) 
 REPRESENTATION_ITEM ( '' )  SURFACE ( )  );
#13798 = EDGE_LOOP ( 'NONE', ( #23684, #22743, #33044 ) ) ;
#13799 = CARTESIAN_POINT ( 'NONE',  ( -0.2399999999999999079, -2.026158573466833257, -0.3155405389364156488 ) ) ;
#13801 = CARTESIAN_POINT ( 'NONE',  ( 0.000000000000000000, 0.1919340784543128453, -0.1767348310837237868 ) ) ;
#13800 = CARTESIAN_POINT ( 'NONE',  ( 0.05252359774140119564, 0.4432374118283801123, 0.1535299757497397000 ) ) ;
#13802 = DIRECTION ( 'NONE',  ( -6.162975822039154046E-33, 0.000000000000000000, -1.000000000000000000 ) ) ;
#13803 = APPROVAL_DATE_TIME ( #1296, #28650 ) ;
#13804 = FACE_OUTER_BOUND ( 'NONE', #18513, .T. ) ;
#13806 = EDGE_LOOP ( 'NONE', ( #9703, #1016, #13085 ) ) ;
#13805 = ORIENTED_EDGE ( 'NONE', *, *, #12734, .F. ) ;
#13807 = CARTESIAN_POINT ( 'NONE',  ( 0.1487996072293812644, -0.8705227087253726292, 0.5144977190368104081 ) ) ;
#13808 = CARTESIAN_POINT ( 'NONE',  ( 0.09004308680322813119, -0.5453319202395334742, 0.1700947645392699159 ) ) ;
#13809 = CARTESIAN_POINT ( 'NONE',  ( 0.4164415605102140816, -1.305827022127384884, 0.8402016264797032008 ) ) ;
#13810 = CARTESIAN_POINT ( 'NONE',  ( 0.06579623839312427613, -1.299927852201166356, 0.6199554873623526197 ) ) ;
#13811 = CARTESIAN_POINT ( 'NONE',  ( 0.5007472363511182856, -1.585864761131932532, -0.4741568162196909131 ) ) ;
#13812 = CARTESIAN_POINT ( 'NONE',  ( 0.6933406572447815552, -1.440653850451423468, 0.5079424769205712620 ) ) ;
#13813 = CARTESIAN_POINT ( 'NONE',  ( 0.02999999999997886302, -2.183180860297921466, -0.4937760292030871079 ) ) ;
#13814 = B_SPLINE_CURVE_WITH_KNOTS ( 'NONE', 3,
 ( #9328, #25182, #30745, #34224, #14912, #37124, #27468, #6036, #21907, #18195, #37725, #18603, #34434, #15100, #6252, #31162 ),
 .UNSPECIFIED., .F., .F.,
 ( 4, 2, 2, 2, 2, 2, 2, 4 ),
 ( 0.001520026421036642893, 0.002129310495689869936, 0.002738594570343096547, 0.003347878644996323157, 0.003957162719649550200, 0.004566446794302777244, 0.005175730868956004288, 0.006394299018262457508 ),
 .UNSPECIFIED. ) ;
#13815 = CARTESIAN_POINT ( 'NONE',  ( 0.7430335777066456870, -1.516427533338710276, 0.5621624951216923627 ) ) ;
#13816 = CARTESIAN_POINT ( 'NONE',  ( 0.06581764578086071737, -1.340728352476673546, 0.5449258910593480776 ) ) ;
#13817 = DIRECTION ( 'NONE',  ( -1.000000000000000000, -0.000000000000000000, -0.000000000000000000 ) ) ;
#13818 = CIRCLE ( 'NONE', #1365, 0.01500000000000003067 ) ;
#13819 = DIRECTION ( 'NONE',  ( 0.000000000000000000, 1.951319995474468994E-15, -1.000000000000000000 ) ) ;
#13820 = CARTESIAN_POINT ( 'NONE',  ( -0.0002679541628580975484, -0.8872122825745146768, -0.004047411357262368885 ) ) ;
#13821 = CARTESIAN_POINT ( 'NONE',  ( 0.5721826821263369389, -1.458777054030341747, 0.7189295076877989521 ) ) ;
#13822 = DIRECTION ( 'NONE',  ( 0.000000000000000000, 0.8585432690668223232, -0.5127411190260187102 ) ) ;
#13823 = LINE ( 'NONE', #4756, #7408 ) ;
#13824 = CARTESIAN_POINT ( 'NONE',  ( 0.002166586416275674380, -0.8510908774931603693, 0.4206164911499951642 ) ) ;
#13825 = CARTESIAN_POINT ( 'NONE',  ( 0.4927016384402401195, -1.082581181811578697, 0.5750743434332348247 ) ) ;
#13826 = DATE_AND_TIME ( #39147, #22054 ) ;
#13827 = CARTESIAN_POINT ( 'NONE',  ( 0.5337404313129848754, -1.165174529015815530, 0.8761190665599410954 ) ) ;
#13828 = CARTESIAN_POINT ( 'NONE',  ( 0.3699999999999786793, -2.120797187169804143, -0.5256435360466946705 ) ) ;
#13829 = CARTESIAN_POINT ( 'NONE',  ( 0.3165154177081624387, -1.761756825665560022, 0.5689576620947197627 ) ) ;
#13830 = ORIENTED_EDGE ( 'NONE', *, *, #22110, .T. ) ;
#13831 = CARTESIAN_POINT ( 'NONE',  ( -0.004088490883478934287, -1.369644552158580053, -0.6494983983435047570 ) ) ;
#13832 = CARTESIAN_POINT ( 'NONE',  ( 0.01055999354154677286, -0.5296565605740106708, 0.1345257393686825065 ) ) ;
#13833 = AXIS2_PLACEMENT_3D ( 'NONE', #34842, #3790, #28882 ) ;
#13834 = CARTESIAN_POINT ( 'NONE',  ( 0.1251292443316412706, -1.283366339454344196, 0.4333571588881200976 ) ) ;
#13835 = ORIENTED_EDGE ( 'NONE', *, *, #3753, .F. ) ;
#13836 = DIRECTION ( 'NONE',  ( 1.000000000000000000, 0.000000000000000000, 0.000000000000000000 ) ) ;
#13837 = CARTESIAN_POINT ( 'NONE',  ( 0.5104750172518451867, -1.131314744720151477, 0.8088526445616294192 ) ) ;
#13839 = VERTEX_POINT ( 'NONE', #9037 ) ;
#13838 = ORIENTED_EDGE ( 'NONE', *, *, #32150, .T. ) ;
#13840 = CARTESIAN_POINT ( 'NONE',  ( -4.849418284861270240E-05, -2.028079589045944875, -0.6757198890148005122 ) ) ;
#13841 = AXIS2_PLACEMENT_3D ( 'NONE', #22580, #13510, #22790 ) ;
#13842 = CARTESIAN_POINT ( 'NONE',  ( 0.3616412802241143476, -1.759290408630900693, -0.5212859374495405484 ) ) ;
#13843 = CIRCLE ( 'NONE', #30941, 0.1033070866141734129 ) ;
#13844 = AXIS2_PLACEMENT_3D ( 'NONE', #8692, #11996, #33588 ) ;
#13845 = CARTESIAN_POINT ( 'NONE',  ( -0.05634115714581326706, 0.4380405955734048007, -0.1368374331724235560 ) ) ;
#13846 = VERTEX_POINT ( 'NONE', #30437 ) ;
#13847 = DIRECTION ( 'NONE',  ( 1.000000000000000000, -0.000000000000000000, -0.000000000000000000 ) ) ;
#13848 = CARTESIAN_POINT ( 'NONE',  ( 0.08904301877626455419, -0.6451442797342821223, 0.1752162043042217454 ) ) ;
#13849 = CARTESIAN_POINT ( 'NONE',  ( 0.2340814018463421020, -1.370659533647821116, 1.031107782677665119 ) ) ;
#13850 = CARTESIAN_POINT ( 'NONE',  ( 0.08527833055735040135, -0.5435345793325218056, 0.1626648481634892229 ) ) ;
#13852 = CARTESIAN_POINT ( 'NONE',  ( -0.02000000000000000042, -2.468922287121626091, -0.3957877349972418468 ) ) ;
#13851 = CARTESIAN_POINT ( 'NONE',  ( 0.2421782067677001327, -1.538462374013507494, 0.9033803661575985355 ) ) ;
#13853 = CARTESIAN_POINT ( 'NONE',  ( 0.3600618142828818646, -1.126602618899190666, 0.6272543034982291932 ) ) ;
#13854 = ORIENTED_EDGE ( 'NONE', *, *, #25287, .T. ) ;
#13855 = EDGE_LOOP ( 'NONE', ( #27615, #31717, #15117, #19507, #26633 ) ) ;
#13856 = CARTESIAN_POINT ( 'NONE',  ( 0.6613703362948644138, -1.499461042372710162, -0.6190604815614721979 ) ) ;
#13857 = CARTESIAN_POINT ( 'NONE',  ( 0.2438833895742764379, -0.7102944716943135894, 0.5217179281748908215 ) ) ;
#13858 = DIRECTION ( 'NONE',  ( 1.000000000000000000, 2.280301054154495132E-31, -1.664003471950577689E-31 ) ) ;
#13859 = DIRECTION ( 'NONE',  ( 0.000000000000000000, 0.000000000000000000, -1.000000000000000000 ) ) ;
#13860 = AXIS2_PLACEMENT_3D ( 'NONE', #1248, #20551, #10670 ) ;
#13861 = CARTESIAN_POINT ( 'NONE',  ( 0.001520397658112405872, -0.4673780482903918676, 0.1457185332388684362 ) ) ;
#13862 = DIRECTION ( 'NONE',  ( 0.8660512985181134660, 0.4999551463232371207, 0.000000000000000000 ) ) ;
#13863 = CARTESIAN_POINT ( 'NONE',  ( 0.6177995476601370051, -1.296677486146512681, 0.6035100636680229558 ) ) ;
#13864 = DIRECTION ( 'NONE',  ( 1.000000000000000000, 6.779273404243070203E-32, 4.314083075427408311E-32 ) ) ;
#13865 = CARTESIAN_POINT ( 'NONE',  ( 0.006138594813777389046, -0.8471251931369432331, 0.2368169677984677812 ) ) ;
#13866 = AXIS2_PLACEMENT_3D ( 'NONE', #10056, #13554, #10275 ) ;
#13867 = AXIS2_PLACEMENT_3D ( 'NONE', #25973, #13399, #19586 ) ;
#13868 = DIRECTION ( 'NONE',  ( 0.000000000000000000, 0.000000000000000000, -1.000000000000000000 ) ) ;
#13869 = LINE ( 'NONE', #1782, #14035 ) ;
#13870 = CARTESIAN_POINT ( 'NONE',  ( 0.3974715091898353148, -1.183013071782477610, 0.7014967152191310396 ) ) ;
#13871 = DIRECTION ( 'NONE',  ( 0.8660512985181131329, 0.4999551463232375648, 0.000000000000000000 ) ) ;
#13872 = CARTESIAN_POINT ( 'NONE',  ( -0.03303708955568313704, -0.2303604322856099840, -0.4672397951413049255 ) ) ;
#13873 = ORIENTED_EDGE ( 'NONE', *, *, #16230, .T. ) ;
#13874 = CARTESIAN_POINT ( 'NONE',  ( 0.5370561722153690543, -1.157568837174978160, 0.6041238513417164224 ) ) ;
#13875 = CARTESIAN_POINT ( 'NONE',  ( 0.08989780363036058153, -0.5646359461869331353, 0.1460065308160271857 ) ) ;
#13876 = CARTESIAN_POINT ( 'NONE',  ( 0.02999999999997891853, -2.097675824466501915, -0.7286991843995629381 ) ) ;
#13877 = DIRECTION ( 'NONE',  ( -8.881784197001245421E-16, 2.361472542561082612E-16, -1.000000000000000000 ) ) ;
#13878 = B_SPLINE_CURVE_WITH_KNOTS ( 'NONE', 3,
 ( #18221, #24397, #2791, #27682 ),
 .UNSPECIFIED., .F., .F.,
 ( 4, 4 ),
 ( 2.088448796179171202E-15, 0.0003951776346070152404 ),
 .UNSPECIFIED. ) ;
#13879 = AXIS2_PLACEMENT_3D ( 'NONE', #10024, #3838, #31838 ) ;
#13880 = CARTESIAN_POINT ( 'NONE',  ( 0.08519453467371698729, -0.8897552423473668037, 0.5328790022427215556 ) ) ;
#13881 = EDGE_LOOP ( 'NONE', ( #33399, #9327, #27667, #15318 ) ) ;
#13882 = CARTESIAN_POINT ( 'NONE',  ( -0.1631341089705740377, 0.4729174206798267277, 0.3373594846482269038 ) ) ;
#13883 = EDGE_CURVE ( 'NONE', #34509, #17498, #16074, .T. ) ;
#13884 = CARTESIAN_POINT ( 'NONE',  ( 0.6625354623209831484, -1.473466724634002523, -0.4125543668030850486 ) ) ;
#13885 = CARTESIAN_POINT ( 'NONE',  ( 0.01548846960707388198, -0.5203207976467953966, -0.08861466064782426433 ) ) ;
#13886 = PRODUCT_RELATED_PRODUCT_CATEGORY ( 'detail', '', ( #35397 ) ) ;
#13887 = DIRECTION ( 'NONE',  ( -0.3468893892380665034, -0.3199132558031917983, -0.8816593788960922495 ) ) ;
#13888 = CARTESIAN_POINT ( 'NONE',  ( 0.4400018551782722831, -1.199590102754184429, 0.6918963007991280056 ) ) ;
#13889 = AXIS2_PLACEMENT_3D ( 'NONE', #37864, #9682, #31683 ) ;
#13891 = CARTESIAN_POINT ( 'NONE',  ( 0.5680530317233595250, -1.627115649102798045, 0.5337353644224959170 ) ) ;
#13890 = FACE_BOUND ( 'NONE', #7514, .T. ) ;
#13892 = CARTESIAN_POINT ( 'NONE',  ( 0.5731004126284177103, -1.543550752164076112, -0.5377031886939181993 ) ) ;
#13893 = ORIENTED_EDGE ( 'NONE', *, *, #23589, .F. ) ;
#13894 = CYLINDRICAL_SURFACE ( 'NONE', #9285, 0.08000000000000000167 ) ;
#13895 = VERTEX_POINT ( 'NONE', #28164 ) ;
#13896 = AXIS2_PLACEMENT_3D ( 'NONE', #18736, #21626, #12760 ) ;
#13897 = AXIS2_PLACEMENT_3D ( 'NONE', #14590, #33117, #30222 ) ;
#13898 = CARTESIAN_POINT ( 'NONE',  ( 0.05234297472369140586, -0.5872343478182446841, 0.3233092731135888132 ) ) ;
#13900 = CARTESIAN_POINT ( 'NONE',  ( 0.4500146950278320346, -1.107499313017888065, -0.6660426939124520773 ) ) ;
#13899 = CARTESIAN_POINT ( 'NONE',  ( 0.08897024507276897476, -0.5939270582310836044, 0.06544685392209818875 ) ) ;
#13901 = CARTESIAN_POINT ( 'NONE',  ( -0.2746410161513776482, -3.941790907013290823, -0.4709369376873030477 ) ) ;
#13902 = ORIENTED_EDGE ( 'NONE', *, *, #20270, .T. ) ;
#13903 = CIRCLE ( 'NONE', #25083, 1.986674066779353875 ) ;
#13904 = DIRECTION ( 'NONE',  ( 0.9378410757839558132, 0.3470650033817763158, 0.000000000000000000 ) ) ;
#13905 = CARTESIAN_POINT ( 'NONE',  ( 0.5747667309145861880, -1.499072180388674180, 0.5927272562183352189 ) ) ;
#13906 = ORIENTED_EDGE ( 'NONE', *, *, #2221, .T. ) ;
#13907 = CARTESIAN_POINT ( 'NONE',  ( 0.01548846960707524721, 0.5346638663566671834, 0.07572681171513505338 ) ) ;
#13908 = CARTESIAN_POINT ( 'NONE',  ( 0.02238826743732968277, -0.4611641377668557196, 0.2234181651772608468 ) ) ;
#13909 = EDGE_CURVE ( 'NONE', #36405, #14568, #11905, .T. ) ;
#13910 = CARTESIAN_POINT ( 'NONE',  ( 0.6011193747858255554, -1.595581932925110857, 0.4276689662439312478 ) ) ;
#13911 = CARTESIAN_POINT ( 'NONE',  ( 0.08570207522761710828, -1.306251794185867565, 0.4630506868879065152 ) ) ;
#13912 = CARTESIAN_POINT ( 'NONE',  ( 0.1424029337235096226, -1.400533250147911746, -0.6250000000000000000 ) ) ;
#13913 = CARTESIAN_POINT ( 'NONE',  ( 0.08964573052713356582, -0.6030796524031889483, 0.1052737554848243579 ) ) ;
#13914 = AXIS2_PLACEMENT_3D ( 'NONE', #6275, #16357, #37751 ) ;
#13915 = ADVANCED_FACE ( 'NONE', ( #17871 ), #8830, .T. ) ;
#13916 = CARTESIAN_POINT ( 'NONE',  ( 0.3279357908889724005, -0.8116789304350262579, 0.7312476538325396458 ) ) ;
#13917 = EDGE_CURVE ( 'NONE', #26889, #28266, #2860, .T. ) ;
#13918 = DIRECTION ( 'NONE',  ( -2.218671295934093951E-31, -0.6954292836768477537, 0.7185945389471773970 ) ) ;
#13919 = CARTESIAN_POINT ( 'NONE',  ( 0.4781934768423676818, -1.682642038360962600, -0.6151431148613257793 ) ) ;
#13920 = APPROVAL_ROLE ( '' ) ;
#13921 = ADVANCED_FACE ( 'NONE', ( #33715 ), #30396, .T. ) ;
#13922 = AXIS2_PLACEMENT_3D ( 'NONE', #16067, #3903, #12981 ) ;
#13923 = EDGE_CURVE ( 'NONE', #6325, #9452, #35455, .T. ) ;
#13924 = B_SPLINE_CURVE_WITH_KNOTS ( 'NONE', 3,
 ( #1611, #13720, #4459, #20731, #20320, #17629, #7944, #20518, #23212, #39023 ),
 .UNSPECIFIED., .F., .F.,
 ( 4, 2, 2, 2, 4 ),
 ( 8.597723227810050162E-17, 0.0007834172717712229415, 0.001566834543542360448, 0.002350251815313497521, 0.003133669087084634593 ),
 .UNSPECIFIED. ) ;
#13925 = DIRECTION ( 'NONE',  ( 0.8660512985181134660, 0.4999551463232372872, 0.000000000000000000 ) ) ;
#13926 = CARTESIAN_POINT ( 'NONE',  ( 0.2261350199769993075, -1.351787128704465824, 0.4952186049488564445 ) ) ;
#13927 = CARTESIAN_POINT ( 'NONE',  ( -0.01548846960707477016, 0.2372406987223678043, 0.4850946823762586901 ) ) ;
#13928 = EDGE_CURVE ( 'NONE', #5083, #36014, #38395, .T. ) ;
#13929 = CARTESIAN_POINT ( 'NONE',  ( 0.4212779473123670071, -1.592273152480388365, -0.6162687442765694135 ) ) ;
#13930 = CARTESIAN_POINT ( 'NONE',  ( 0.1016012100809402935, -1.316932346213368854, 0.4414107644021351140 ) ) ;
#13931 = VECTOR ( 'NONE', #8647, 39.37007874015748143 ) ;
#13932 = AXIS2_PLACEMENT_3D ( 'NONE', #10586, #35897, #13673 ) ;
#13933 = CARTESIAN_POINT ( 'NONE',  ( 0.003124719664520466192, -0.5686731593868933343, 0.09441483597926585147 ) ) ;
#13934 = CARTESIAN_POINT ( 'NONE',  ( 0.6010818854071131589, -1.537619199427677552, -0.5899312111515385704 ) ) ;
#13935 = AXIS2_PLACEMENT_3D ( 'NONE', #347, #15108, #18397 ) ;
#13936 = CARTESIAN_POINT ( 'NONE',  ( 0.4165289612192157875, -1.649214957849792995, -0.4090022746517852359 ) ) ;
#13937 = CARTESIAN_POINT ( 'NONE',  ( 0.5943325146468168008, -1.599629339932625571, 0.4280854842635419266 ) ) ;
#13938 = CARTESIAN_POINT ( 'NONE',  ( -0.03171102739523559005, -0.2433685106468572723, 0.4273977451499074154 ) ) ;
#13939 = B_SPLINE_CURVE_WITH_KNOTS ( 'NONE', 3,
 ( #22832, #38222, #19324, #35534, #37834, #12946, #12727, #452, #32061, #25495, #6540, #35351, #19116, #22217 ),
 .UNSPECIFIED., .F., .F.,
 ( 4, 2, 2, 2, 2, 2, 4 ),
 ( 0.000000000000000000, 2.630382555147416532E-05, 5.260765110294833064E-05, 0.0001052153022059013369, 0.0002104306044118009933, 0.0004208612088236007398, 0.0008417224176471900954 ),
 .UNSPECIFIED. ) ;
#13940 = VERTEX_POINT ( 'NONE', #10869 ) ;
#13941 = ORIENTED_EDGE ( 'NONE', *, *, #36386, .T. ) ;
#13942 = CARTESIAN_POINT ( 'NONE',  ( 0.1051168147106792405, -1.410983822109892261, 0.5678361409211155619 ) ) ;
#13943 = EDGE_CURVE ( 'NONE', #13132, #19301, #16739, .T. ) ;
#13944 = DIRECTION ( 'NONE',  ( -0.8660512985181133550, -0.4999551463232373982, 0.000000000000000000 ) ) ;
#13945 = ORIENTED_EDGE ( 'NONE', *, *, #29097, .F. ) ;
#13946 = CARTESIAN_POINT ( 'NONE',  ( -1.019575837292306053, -0.04310840302198148261, 0.09999999999999975575 ) ) ;
#13947 = CARTESIAN_POINT ( 'NONE',  ( 0.3512419370235244087, -1.705526293757532397, -0.4723484404679085258 ) ) ;
#13948 = CARTESIAN_POINT ( 'NONE',  ( 0.4421893865606449370, -1.209647901485848109, 0.7918999424850913238 ) ) ;
#13950 = ORIENTED_EDGE ( 'NONE', *, *, #32147, .F. ) ;
#13949 = CARTESIAN_POINT ( 'NONE',  ( -0.1508021419688887199, 0.4665171419162565392, 0.09550516381870571836 ) ) ;
#13951 = CARTESIAN_POINT ( 'NONE',  ( 0.2017226021742919428, -0.8083333955854449249, 0.3447374551949819454 ) ) ;
#13952 = CARTESIAN_POINT ( 'NONE',  ( -2.112274968902149179E-14, -2.062017255485956824, -0.3032107891533308286 ) ) ;
#13953 = ORIENTED_EDGE ( 'NONE', *, *, #30108, .T. ) ;
#13954 = DIRECTION ( 'NONE',  ( 1.000000000000000000, 1.609192080950324210E-13, -1.762723797404872045E-11 ) ) ;
#13955 = CARTESIAN_POINT ( 'NONE',  ( 0.3285372126246737245, -1.620950097204016283, 0.7294768256710487675 ) ) ;
#13957 = CARTESIAN_POINT ( 'NONE',  ( -0.01895884884825285027, -0.5124024296374548593, 0.08888335629179863751 ) ) ;
#13956 = CARTESIAN_POINT ( 'NONE',  ( 0.6870256655133099022, -1.509029865219357003, 0.4581990961816077568 ) ) ;
#13958 = CARTESIAN_POINT ( 'NONE',  ( 0.1581650021276240492, -1.285700486175305413, 0.4282417262808778102 ) ) ;
#13959 = VECTOR ( 'NONE', #37050, 39.37007874015748854 ) ;
#13960 = CARTESIAN_POINT ( 'NONE',  ( 0.02666506398941732164, -1.593264902264835081, -0.3735695336613014117 ) ) ;
#13961 = ORIENTED_EDGE ( 'NONE', *, *, #34775, .T. ) ;
#13962 = CARTESIAN_POINT ( 'NONE',  ( -0.05464101615137770263, -2.183180860297908144, -0.4937760292030871079 ) ) ;
#13963 = CARTESIAN_POINT ( 'NONE',  ( -0.1163196563843198195, -0.5318992644065131392, 0.3135508459095567302 ) ) ;
#13964 = DIRECTION ( 'NONE',  ( -0.3779644730092268090, 0.000000000000000000, 0.9258200997725516412 ) ) ;
#13965 = AXIS2_PLACEMENT_3D ( 'NONE', #4925, #23670, #29624 ) ;
#13966 = CIRCLE ( 'NONE', #30426, 0.04749999999977543713 ) ;
#13967 = CARTESIAN_POINT ( 'NONE',  ( 0.3513474575719932047, -1.212688753581547152, 0.6982256170334331102 ) ) ;
#13968 = CARTESIAN_POINT ( 'NONE',  ( -0.02953079040095700838, 0.09152108205202039160, -0.5223162075576429642 ) ) ;
#13969 = AXIS2_PLACEMENT_3D ( 'NONE', #28185, #14827, #2680 ) ;
#13970 = CARTESIAN_POINT ( 'NONE',  ( -0.1625122179509601028, 0.5048329626761722810, 0.3461446680885716387 ) ) ;
#13971 = DIRECTION ( 'NONE',  ( -0.8660512985181135770, -0.4999551463232370652, 0.000000000000000000 ) ) ;
#13972 = EDGE_CURVE ( 'NONE', #27442, #22278, #37081, .T. ) ;
#13973 = DIRECTION ( 'NONE',  ( 0.000000000000000000, 0.000000000000000000, -1.000000000000000000 ) ) ;
#13974 = DIRECTION ( 'NONE',  ( -1.355854680848614260E-31, 3.330669073875470114E-16, 1.000000000000000000 ) ) ;
#13975 = DIRECTION ( 'NONE',  ( 1.188678714063518227E-15, -1.000000000000000000, -3.263080277421930985E-16 ) ) ;
#13976 = CARTESIAN_POINT ( 'NONE',  ( 0.1876095839365586326, -1.270310460104812966, 0.4182417262808778013 ) ) ;
#13977 = ADVANCED_FACE ( 'NONE', ( #31601 ), #32673, .F. ) ;
#13978 = CARTESIAN_POINT ( 'NONE',  ( 0.3619206956467402869, -1.158069748661290310, 0.4377863372772762829 ) ) ;
#13979 = ADVANCED_FACE ( 'NONE', ( #9383 ), #31213, .F. ) ;
#13980 = CARTESIAN_POINT ( 'NONE',  ( 5.463695987328526437E-16, -0.2899999999999993694, -7.171100983368691195E-16 ) ) ;
#13981 = CARTESIAN_POINT ( 'NONE',  ( 0.7089445223657345752, -1.512404601863501119, 0.5481705145598362305 ) ) ;
#13982 = ORIENTED_EDGE ( 'NONE', *, *, #4525, .F. ) ;
#13983 = DIRECTION ( 'NONE',  ( 1.000000000000000000, 0.000000000000000000, 0.000000000000000000 ) ) ;
#13984 = CARTESIAN_POINT ( 'NONE',  ( -0.3000000000000000999, -3.880844374714816247, -0.2860650318788287017 ) ) ;
#13985 = AXIS2_PLACEMENT_3D ( 'NONE', #31853, #13324, #3858 ) ;
#13986 = CARTESIAN_POINT ( 'NONE',  ( 0.1975154665785900376, -1.291488013533474755, 1.023236177360688393 ) ) ;
#13987 = FACE_OUTER_BOUND ( 'NONE', #13402, .T. ) ;
#13988 = EDGE_LOOP ( 'NONE', ( #13135, #32168, #32468, #18007 ) ) ;
#13989 = CIRCLE ( 'NONE', #8731, 0.1599999999999999201 ) ;
#13990 = VERTEX_POINT ( 'NONE', #15761 ) ;
#13991 = VECTOR ( 'NONE', #24840, 39.37007874015748143 ) ;
#13992 = ADVANCED_FACE ( 'NONE', ( #5695 ), #8992, .F. ) ;
#13993 = CARTESIAN_POINT ( 'NONE',  ( 0.1912095264562755359, -0.5378710435959832559, 0.2569485330840456383 ) ) ;
#13994 = ORIENTED_EDGE ( 'NONE', *, *, #23531, .T. ) ;
#13995 = CARTESIAN_POINT ( 'NONE',  ( 0.4207172239728091956, -1.680578273617128859, -0.4138233700378491364 ) ) ;
#13996 = EDGE_CURVE ( 'NONE', #18456, #11375, #23976, .T. ) ;
#13997 = CARTESIAN_POINT ( 'NONE',  ( 0.6017699220438542662, -1.483087398378163613, 0.5690941353624772159 ) ) ;
#13999 = ORIENTED_EDGE ( 'NONE', *, *, #12838, .F. ) ;
#13998 = CARTESIAN_POINT ( 'NONE',  ( -0.001435095205611100358, -0.8221821212370526988, 0.04482441723982503318 ) ) ;
#14000 = EDGE_CURVE ( 'NONE', #25089, #40017, #13444, .T. ) ;
#14001 = VECTOR ( 'NONE', #8053, 39.37007874015748143 ) ;
#14002 = ORIENTED_EDGE ( 'NONE', *, *, #23769, .T. ) ;
#14003 = CARTESIAN_POINT ( 'NONE',  ( 0.5780995139542189909, -1.354416361880780073, 0.8813196190093472993 ) ) ;
#14004 = VERTEX_POINT ( 'NONE', #30796 ) ;
#14005 = CARTESIAN_POINT ( 'NONE',  ( 0.2226433022657542116, -1.491184131797351764, 0.9185802828613613968 ) ) ;
#14007 = DIRECTION ( 'NONE',  ( -0.8660254037844421493, -0.1903656704315992709, -0.4623428506218321132 ) ) ;
#14006 = CARTESIAN_POINT ( 'NONE',  ( 0.1977814221236954828, -1.253108843398078820, -0.3161890964247148217 ) ) ;
#14008 = CARTESIAN_POINT ( 'NONE',  ( 0.7879355633825926297, -1.507076940126293341, -0.5155029497116575543 ) ) ;
#14009 = COORDINATED_UNIVERSAL_TIME_OFFSET ( 0, 0, .AHEAD. ) ;
#14010 = DIRECTION ( 'NONE',  ( 0.000000000000000000, 0.000000000000000000, -1.000000000000000000 ) ) ;
#14012 = EDGE_LOOP ( 'NONE', ( #3886, #36272, #25424, #3053 ) ) ;
#14011 = EDGE_LOOP ( 'NONE', ( #40493, #9094 ) ) ;
#14013 = CARTESIAN_POINT ( 'NONE',  ( 0.1246135125235463964, -0.8485378787666528755, 0.4456728382190667248 ) ) ;
#14014 = CARTESIAN_POINT ( 'NONE',  ( 0.03641803280491349298, -0.9675207775044110114, 0.6564218488141688734 ) ) ;
#14015 = CARTESIAN_POINT ( 'NONE',  ( 0.1040734670749448865, -0.6192425880305225672, 0.3761511251374745068 ) ) ;
#14016 = CARTESIAN_POINT ( 'NONE',  ( 0.5527105129315168508, -1.511112255258006076, 0.5682628627402200872 ) ) ;
#14017 = CARTESIAN_POINT ( 'NONE',  ( 0.1867173357226489527, -0.5319602528017867149, 0.2749521773151894499 ) ) ;
#14018 = CARTESIAN_POINT ( 'NONE',  ( 0.4846270837680086707, -1.589735006747021506, -0.4491141958821768809 ) ) ;
#14019 = CARTESIAN_POINT ( 'NONE',  ( 0.6350649561464823956, -1.569019770697453353, 0.4218989278589421743 ) ) ;
#14020 = AXIS2_PLACEMENT_3D ( 'NONE', #20860, #29905, #1143 ) ;
#14021 = CARTESIAN_POINT ( 'NONE',  ( 0.3344130170398624813, -1.762663979654706781, 0.5617402743204308324 ) ) ;
#14022 = DIRECTION ( 'NONE',  ( 1.000000000000000000, 0.000000000000000000, 0.000000000000000000 ) ) ;
#14023 = CARTESIAN_POINT ( 'NONE',  ( 0.07014435923142074703, -1.325199841737238593, 0.5075297796643147841 ) ) ;
#14024 = AXIS2_PLACEMENT_3D ( 'NONE', #30550, #2368, #14909 ) ;
#14025 = DIRECTION ( 'NONE',  ( 0.000000000000000000, 0.000000000000000000, 1.000000000000000000 ) ) ;
#14026 = CARTESIAN_POINT ( 'NONE',  ( -0.1212602504878780296, -0.5073146173917505442, 0.1497995784944539388 ) ) ;
#14027 = VECTOR ( 'NONE', #30924, 39.37007874015747433 ) ;
#14028 = CARTESIAN_POINT ( 'NONE',  ( 8.553562515601560484E-05, -0.6062534121257077135, -0.09029379233708857699 ) ) ;
#14029 = CARTESIAN_POINT ( 'NONE',  ( 0.5701105534977165545, -1.454650725906061481, 0.7252577283312120482 ) ) ;
#14030 =( CONVERSION_BASED_UNIT ( 'INCH', #33166 ) LENGTH_UNIT ( ) NAMED_UNIT ( #10478 ) );
#14031 = EDGE_CURVE ( 'NONE', #40356, #38394, #35118, .T. ) ;
#14032 = CARTESIAN_POINT ( 'NONE',  ( 0.008070443708631632601, -0.7078080424802363213, -0.01128278948062920277 ) ) ;
#14033 = DIRECTION ( 'NONE',  ( 0.5000000000000001110, -3.759415251443887888E-31, -0.8660254037844385966 ) ) ;
#14034 = CARTESIAN_POINT ( 'NONE',  ( 0.04376425988958544677, -0.9339557565548041174, 0.7112009851976159869 ) ) ;
#14035 = VECTOR ( 'NONE', #20078, 39.37007874015748143 ) ;
#14036 = CARTESIAN_POINT ( 'NONE',  ( 0.3793958449840821867, -1.004087596663555848, 0.6383754926613092184 ) ) ;
#14037 = DATE_TIME_ROLE ( 'creation_date' ) ;
#14038 = CARTESIAN_POINT ( 'NONE',  ( 0.5117021325268811260, -1.128961434293810129, 0.8718124831259003171 ) ) ;
#14039 = AXIS2_PLACEMENT_3D ( 'NONE', #38479, #13377, #18956 ) ;
#14040 = CARTESIAN_POINT ( 'NONE',  ( 0.1999999999999789724, -2.183180860297921466, -0.4437760292030870635 ) ) ;
#14041 = CARTESIAN_POINT ( 'NONE',  ( 0.3047912954742191260, -1.756872613064056399, 0.5682345314727886842 ) ) ;
#14042 =( BOUNDED_SURFACE ( )  B_SPLINE_SURFACE ( 3, 2, ( 
 ( #20088, #32202, #39750 ),
 ( #32618, #4428, #38989 ),
 ( #11582, #10822, #23394 ),
 ( #20286, #32806, #36665 ),
 ( #29126, #22966, #35487 ),
 ( #19869, #16795, #39951 ),
 ( #21248, #9086, #11769 ),
 ( #37269, #34598, #30703 ),
 ( #2716, #5988, #27614 ),
 ( #21462, #33781, #37678 ),
 ( #37069, #15478, #6400 ),
 ( #9496, #18770, #24539 ),
 ( #24746, #5791, #8887 ),
 ( #18348, #15263, #40355 ) ),
 .UNSPECIFIED., .F., .F., .T. ) 
 B_SPLINE_SURFACE_WITH_KNOTS ( ( 4, 2, 2, 2, 2, 2, 4 ),
 ( 3, 3 ),
 ( -2.179246366695863912E-17, 0.0004568857926695675986, 0.0009137715853391569897, 0.001827543170678335663, 0.002741314756017514120, 0.003198200548687103566, 0.003655086341356693011 ),
 ( 0.000000000000000000, 1.000000000000000000 ),
 .UNSPECIFIED. ) 
 GEOMETRIC_REPRESENTATION_ITEM ( )  RATIONAL_B_SPLINE_SURFACE ( (
 ( 1.000000000000000000, 0.9183064432839357361, 1.000000000000000000),
 ( 1.000000000000000000, 0.9101286041442225860, 1.000000000000000000),
 ( 1.000000000000000000, 0.8997559524681660870, 1.000000000000000000),
 ( 1.000000000000000000, 0.8756591830432681745, 1.000000000000000000),
 ( 1.000000000000000000, 0.8619285237115705822, 1.000000000000000000),
 ( 1.000000000000000000, 0.8162943315712432035, 1.000000000000000000),
 ( 1.000000000000000000, 0.7805544280714898919, 1.000000000000000000),
 ( 1.000000000000000000, 0.7004798398954502625, 1.000000000000000000),
 ( 1.000000000000000000, 0.6558961615331188044, 1.000000000000000000),
 ( 1.000000000000000000, 0.5832821677979773689, 1.000000000000000000),
 ( 1.000000000000000000, 0.5580595141226901701, 1.000000000000000000),
 ( 1.000000000000000000, 0.5067813355089282323, 1.000000000000000000),
 ( 1.000000000000000000, 0.4806792815092485460, 1.000000000000000000),
 ( 1.000000000000000000, 0.4546663607463262702, 1.000000000000000000) ) ) 
 REPRESENTATION_ITEM ( '' )  SURFACE ( )  );
#14043 = ORIENTED_EDGE ( 'NONE', *, *, #24114, .F. ) ;
#14044 = CARTESIAN_POINT ( 'NONE',  ( 0.03113248654051816583, -0.1022126893003200560, -0.2231384537392532841 ) ) ;
#14045 = CARTESIAN_POINT ( 'NONE',  ( 0.002296835029420976181, -0.5198933010532034160, 0.1394354128953856353 ) ) ;
#14046 = EDGE_CURVE ( 'NONE', #4078, #33332, #2936, .T. ) ;
#14047 = AXIS2_PLACEMENT_3D ( 'NONE', #23405, #1378, #23593 ) ;
#14048 = APPLIED_PERSON_AND_ORGANIZATION_ASSIGNMENT ( #14834, #15034, ( #30020 ) ) ;
#14049 = CARTESIAN_POINT ( 'NONE',  ( 0.2196843594954665801, -1.228680355308193084, 0.4993826538774071566 ) ) ;
#14050 = ORIENTED_EDGE ( 'NONE', *, *, #30892, .T. ) ;
#14051 = ADVANCED_FACE ( 'NONE', ( #9177 ), #34277, .T. ) ;
#14052 = CARTESIAN_POINT ( 'NONE',  ( 0.5216412942450647794, -1.664807960596781378, -0.4415788522785766834 ) ) ;
#14053 = CARTESIAN_POINT ( 'NONE',  ( 0.3628146410451159598, -0.9034970372909253422, 0.7254628211502860413 ) ) ;
#14055 = ORIENTED_EDGE ( 'NONE', *, *, #10577, .T. ) ;
#14054 = ORIENTED_EDGE ( 'NONE', *, *, #14934, .F. ) ;
#14056 = CARTESIAN_POINT ( 'NONE',  ( 0.02113718185538869185, -1.627702592408575288, -0.6650890321891688162 ) ) ;
#14057 = TOROIDAL_SURFACE ( 'NONE', #27867, 0.05000000000000000971, 0.1700000000000000400 ) ;
#14058 = ORIENTED_EDGE ( 'NONE', *, *, #7465, .T. ) ;
#14059 = AXIS2_PLACEMENT_3D ( 'NONE', #3276, #24291, #16644 ) ;
#14060 = CARTESIAN_POINT ( 'NONE',  ( 0.3546968572579735635, -1.819852142027485131, -0.4886286422906724325 ) ) ;
#14061 = PRODUCT_DEFINITION_SHAPE ( 'NONE', 'NONE',  #40664 ) ;
#14062 = CARTESIAN_POINT ( 'NONE',  ( 0.4422962341139744513, -1.227940648741109531, 0.5902935990525034482 ) ) ;
#14063 = CARTESIAN_POINT ( 'NONE',  ( -0.05279185365593402207, 0.4562178057548016419, -0.1062796545748909277 ) ) ;
#14064 = VERTEX_POINT ( 'NONE', #3415 ) ;
#14065 = CARTESIAN_POINT ( 'NONE',  ( 0.1766140053765036799, -0.4884607529735562892, 0.1457336358543773192 ) ) ;
#14066 = CARTESIAN_POINT ( 'NONE',  ( 0.09293816641532150202, -0.6949693946930408650, 0.2718681940744577252 ) ) ;
#14067 = VECTOR ( 'NONE', #27900, 39.37007874015748143 ) ;
#14068 = CARTESIAN_POINT ( 'NONE',  ( 0.1805964634074843922, -1.181094138890736334, 1.011330471386135743 ) ) ;
#14069 = CARTESIAN_POINT ( 'NONE',  ( 0.4706205245075478771, -1.558028661862049136, 0.5883446331395899564 ) ) ;
#14070 = VECTOR ( 'NONE', #23054, 39.37007874015748143 ) ;
#14072 = CARTESIAN_POINT ( 'NONE',  ( 0.3182330667144250280, -1.645712786916206927, 0.6043827481625060338 ) ) ;
#14071 = CARTESIAN_POINT ( 'NONE',  ( 0.2705891343394069004, -1.683541877783801377, 0.6654023006082908642 ) ) ;
#14073 = CARTESIAN_POINT ( 'NONE',  ( 0.04894342265781252005, -0.9443920355984648518, 0.2726795326779477557 ) ) ;
#14074 = ORIENTED_EDGE ( 'NONE', *, *, #9504, .F. ) ;
#14075 = CARTESIAN_POINT ( 'NONE',  ( 0.6539014128097314638, -1.538642141127189777, -0.6149031108187260619 ) ) ;
#14076 = CARTESIAN_POINT ( 'NONE',  ( 0.1220876931611632188, -0.4987358795490002272, 0.3421387242878536905 ) ) ;
#14077 = DIRECTION ( 'NONE',  ( 0.000000000000000000, 0.000000000000000000, -1.000000000000000000 ) ) ;
#14078 = CARTESIAN_POINT ( 'NONE',  ( -0.04047161733259348887, -0.4923636041515490613, -0.09403655331106135218 ) ) ;
#14079 = CIRCLE ( 'NONE', #18015, 0.5756329413417605734 ) ;
#14080 = EDGE_CURVE ( 'NONE', #24800, #13526, #20806, .T. ) ;
#14081 = DIRECTION ( 'NONE',  ( 0.2828184691484104119, -0.9591734532964044657, 6.098997937655262350E-13 ) ) ;
#14082 = FACE_OUTER_BOUND ( 'NONE', #34572, .T. ) ;
#14083 = CARTESIAN_POINT ( 'NONE',  ( 0.3991878447057942703, -0.9797369418029474586, 0.7176166460480870590 ) ) ;
#14084 = AXIS2_PLACEMENT_3D ( 'NONE', #15617, #21179, #24470 ) ;
#14085 = CIRCLE ( 'NONE', #27868, 0.2526340763130724976 ) ;
#14086 = CARTESIAN_POINT ( 'NONE',  ( -0.1137534828624041094, -0.5201328034396337507, 0.1183403147931640642 ) ) ;
#14087 = AXIS2_PLACEMENT_3D ( 'NONE', #22454, #35201, #12565 ) ;
#14088 = CARTESIAN_POINT ( 'NONE',  ( 0.1960722456818423942, -1.288731303253011218, -0.2917126172454974631 ) ) ;
#14089 = CARTESIAN_POINT ( 'NONE',  ( 0.4252567597254975906, -1.612150615425755662, -0.6654510194314403604 ) ) ;
#14090 = VERTEX_POINT ( 'NONE', #21961 ) ;
#14091 = DIRECTION ( 'NONE',  ( -1.000000000000000000, -2.280301054154495132E-31, 1.664003471950577689E-31 ) ) ;
#14092 = CARTESIAN_POINT ( 'NONE',  ( -0.2399999999999999079, -3.579933075828130473, -0.2145427270617870641 ) ) ;
#14093 = AXIS2_PLACEMENT_3D ( 'NONE', #18992, #37488, #15899 ) ;
#14094 = CARTESIAN_POINT ( 'NONE',  ( -0.05186792262756985405, -0.2620061627190611864, -0.3911910583554863430 ) ) ;
#14095 = EDGE_LOOP ( 'NONE', ( #5548, #13153, #11439, #29443 ) ) ;
#14096 = CARTESIAN_POINT ( 'NONE',  ( 0.5209244318938980323, -1.136454935809554589, 0.6601900591555691644 ) ) ;
#14097 = CARTESIAN_POINT ( 'NONE',  ( -0.05561170715395123004, 0.02038383341412555033, -0.4604752114371309935 ) ) ;
#14098 = B_SPLINE_CURVE_WITH_KNOTS ( 'NONE', 3,
 ( #25743, #16680, #3916, #29231, #38680, #10497, #35801, #19759, #10319, #16890 ),
 .UNSPECIFIED., .F., .F.,
 ( 4, 2, 2, 2, 4 ),
 ( 0.005469996267440097384, 0.006262957826661069011, 0.007055919385882040637, 0.007848880945103012263, 0.008641842504323983890 ),
 .UNSPECIFIED. ) ;
#14099 = DIRECTION ( 'NONE',  ( -1.000000000000000000, -0.000000000000000000, -0.000000000000000000 ) ) ;
#14100 = CARTESIAN_POINT ( 'NONE',  ( 0.2111199334379703363, -1.188696133188541282, 0.7441100336498001067 ) ) ;
#14101 = VERTEX_POINT ( 'NONE', #180 ) ;
#14102 = CARTESIAN_POINT ( 'NONE',  ( 0.02953079040095704308, 0.3810518745593911571, 0.3687679460475725701 ) ) ;
#14103 = FACE_OUTER_BOUND ( 'NONE', #5, .T. ) ;
#14104 = CARTESIAN_POINT ( 'NONE',  ( 0.4487773978977022127, -1.660532028014278794, -0.6367102607372966405 ) ) ;
#14105 = CARTESIAN_POINT ( 'NONE',  ( -0.01548846960707463312, 0.2306506793134060762, 0.4716198300880322658 ) ) ;
#14106 = AXIS2_PLACEMENT_3D ( 'NONE', #17409, #11444, #36537 ) ;
#14107 = CARTESIAN_POINT ( 'NONE',  ( 0.4674780132050370685, -1.240604882716528357, 0.6861010688927965395 ) ) ;
#14108 = EDGE_CURVE ( 'NONE', #9912, #35757, #32490, .T. ) ;
#14110 = DIRECTION ( 'NONE',  ( 0.8660512985181133550, 0.4999551463232373982, 0.000000000000000000 ) ) ;
#14109 = CARTESIAN_POINT ( 'NONE',  ( 0.03113248654051816583, 0.000000000000000000, 0.000000000000000000 ) ) ;
#14111 = CARTESIAN_POINT ( 'NONE',  ( 0.5716789463609788235, -1.545080002123852214, -0.5247704640587483871 ) ) ;
#14112 = ORIENTED_EDGE ( 'NONE', *, *, #16286, .T. ) ;
#14113 = AXIS2_PLACEMENT_3D ( 'NONE', #8916, #2146, #2746 ) ;
#14114 = DIRECTION ( 'NONE',  ( -7.000205099780314469E-17, -1.000000000000000000, 6.590151126658399604E-16 ) ) ;
#14115 = EDGE_LOOP ( 'NONE', ( #15, #28784, #38037, #30231 ) ) ;
#14116 = CIRCLE ( 'NONE', #32522, 0.07999999999999996003 ) ;
#14117 = CARTESIAN_POINT ( 'NONE',  ( 0.1888324354095312907, -0.6407273034312881421, -0.03797464539687132185 ) ) ;
#14118 = AXIS2_PLACEMENT_3D ( 'NONE', #5334, #39711, #17896 ) ;
#14119 = CARTESIAN_POINT ( 'NONE',  ( 0.1449436508646830823, -0.9125365724582368276, 0.7473170813620255704 ) ) ;
#14121 = DIRECTION ( 'NONE',  ( 7.000205099780314469E-17, 1.000000000000000000, -6.590151126658399604E-16 ) ) ;
#14120 = CARTESIAN_POINT ( 'NONE',  ( 0.08986786782462405365, -0.5434483850344659084, 0.1394973511444336789 ) ) ;
#14122 = LINE ( 'NONE', #1807, #30960 ) ;
#14123 = LOCAL_TIME ( 0, 53, 7.000000000000000000, #12942 ) ;
#14124 = ORIENTED_EDGE ( 'NONE', *, *, #30515, .T. ) ;
#14125 = ORIENTED_EDGE ( 'NONE', *, *, #22971, .F. ) ;
#14126 = CARTESIAN_POINT ( 'NONE',  ( 0.5618860505435292474, -1.504674554817216903, 0.5302722728681629194 ) ) ;
#14127 = CARTESIAN_POINT ( 'NONE',  ( 0.5739910737716292788, -1.499268627441381563, 0.5745547377076620776 ) ) ;
#14128 = ORIENTED_EDGE ( 'NONE', *, *, #18352, .T. ) ;
#14129 = VECTOR ( 'NONE', #39676, 39.37007874015748143 ) ;
#14130 = FACE_OUTER_BOUND ( 'NONE', #29526, .T. ) ;
#14131 = CARTESIAN_POINT ( 'NONE',  ( 0.03875673594170155750, -0.4622647171927982135, 0.1151965740700821167 ) ) ;
#14132 = CARTESIAN_POINT ( 'NONE',  ( 0.6474224700345215799, -1.554264730535300343, 0.4226295179704261384 ) ) ;
#14133 = CARTESIAN_POINT ( 'NONE',  ( 0.1619861451291866039, -1.262021649189480010, 0.4327121414366898455 ) ) ;
#14134 = CARTESIAN_POINT ( 'NONE',  ( 0.000000000000000000, 0.5209315849442416324, 0.3202538583802939098 ) ) ;
#14135 = LINE ( 'NONE', #23430, #19418 ) ;
#14136 = CARTESIAN_POINT ( 'NONE',  ( 0.1983812210006687116, -0.5262237738225362671, 0.3723155052761787376 ) ) ;
#14137 = DIRECTION ( 'NONE',  ( -3.406373435249024214E-19, -1.000000000000000000, -7.170354002788761615E-17 ) ) ;
#14138 = AXIS2_PLACEMENT_3D ( 'NONE', #35782, #36179, #32885 ) ;
#14139 = CARTESIAN_POINT ( 'NONE',  ( 0.5746532143667183457, -1.612791820318843605, -0.5120221665867487060 ) ) ;
#14140 = CIRCLE ( 'NONE', #23397, 0.1946589359789743512 ) ;
#14141 = CARTESIAN_POINT ( 'NONE',  ( 0.03875673594170226527, 0.2524061059367339599, 0.4040421724581182983 ) ) ;
#14142 = DIRECTION ( 'NONE',  ( 1.188678714063518227E-15, -1.000000000000000000, -3.263080277421930985E-16 ) ) ;
#14143 = DIRECTION ( 'NONE',  ( 0.9780874495037195082, 0.000000000000000000, -0.2081944790894049990 ) ) ;
#14144 = CARTESIAN_POINT ( 'NONE',  ( -0.04582713223189551627, 0.4790191777205496382, -0.08746099429787626556 ) ) ;
#14145 = LOCAL_TIME ( 0, 53, 7.000000000000000000, #27462 ) ;
#14146 = CARTESIAN_POINT ( 'NONE',  ( 0.02434420200121316033, -0.6484821100597173427, 0.5849520929678148073 ) ) ;
#14147 = CARTESIAN_POINT ( 'NONE',  ( 0.5711877923250709976, -1.574828153980617929, -0.4617130944781254187 ) ) ;
#14148 = CARTESIAN_POINT ( 'NONE',  ( 0.4137599315575946624, -1.590143257116402697, -0.4137273532990791702 ) ) ;
#14149 = DIRECTION ( 'NONE',  ( 1.000000000000000000, -0.000000000000000000, -0.000000000000000000 ) ) ;
#14150 = CARTESIAN_POINT ( 'NONE',  ( 0.7022701326239239039, -1.539209993927390219, 0.4224083929475443977 ) ) ;
#14151 = CIRCLE ( 'NONE', #15488, 0.2000000000000000111 ) ;
#14152 = ORIENTED_EDGE ( 'NONE', *, *, #9212, .F. ) ;
#14153 = ORIENTED_EDGE ( 'NONE', *, *, #7231, .T. ) ;
#14154 = FACE_OUTER_BOUND ( 'NONE', #3278, .T. ) ;
#14155 = CARTESIAN_POINT ( 'NONE',  ( 0.2320755761173002307, -1.232873731908348480, 0.4177417262808779674 ) ) ;
#14156 = ORIENTED_EDGE ( 'NONE', *, *, #26089, .F. ) ;
#14157 = DIRECTION ( 'NONE',  ( 1.000000000000000000, 0.000000000000000000, 0.000000000000000000 ) ) ;
#14158 = CARTESIAN_POINT ( 'NONE',  ( 0.03113248654051816583, 0.1997995745459845707, -0.008951536808938304751 ) ) ;
#14159 = CARTESIAN_POINT ( 'NONE',  ( 0.5380345666174809471, -1.356870216577685140, 0.6895596520374281946 ) ) ;
#14161 = ORIENTED_EDGE ( 'NONE', *, *, #37142, .F. ) ;
#14160 = CARTESIAN_POINT ( 'NONE',  ( -0.03654364704248907331, 0.5058694728073477309, 0.07650507870001060917 ) ) ;
#14162 = CARTESIAN_POINT ( 'NONE',  ( 0.5135987199389938640, -1.118799288056715691, 0.5631670202300380623 ) ) ;
#14163 = EDGE_CURVE ( 'NONE', #5331, #27640, #4878, .T. ) ;
#14164 = CARTESIAN_POINT ( 'NONE',  ( 0.5264113014007612001, -1.640729993778266893, -0.5166151207188711680 ) ) ;
#14165 = ORIENTED_EDGE ( 'NONE', *, *, #7634, .T. ) ;
#14166 = CARTESIAN_POINT ( 'NONE',  ( 0.02953079040095700838, 0.2329676531120452587, -0.4763574306556336291 ) ) ;
#14167 = ADVANCED_FACE ( 'NONE', ( #22174 ), #6492, .T. ) ;
#14168 = CARTESIAN_POINT ( 'NONE',  ( 0.3268949200113892006, -1.639137555909581323, 0.5723008474438366910 ) ) ;
#14170 = DIRECTION ( 'NONE',  ( 0.000000000000000000, -1.024442997624094674E-14, -1.000000000000000000 ) ) ;
#14169 = CARTESIAN_POINT ( 'NONE',  ( 0.7064611863037917328, -1.500587082211219503, 0.5320914120227480115 ) ) ;
#14171 = FACE_OUTER_BOUND ( 'NONE', #34245, .T. ) ;
#14172 = EDGE_CURVE ( 'NONE', #6555, #40516, #10599, .T. ) ;
#14173 = DIRECTION ( 'NONE',  ( 0.8660512985181135770, 0.4999551463232370652, 0.000000000000000000 ) ) ;
#14174 = ORIENTED_EDGE ( 'NONE', *, *, #1522, .F. ) ;
#14175 = CLOSED_SHELL ( 'NONE', ( #24895, #33771, #40099, #16279, #2554, #27287, #17526, #12245, #33590, #38588, #14220, #32602, #7487, #35837, #27852, #21879, #30413, #29280, #2715, #23000, #21714, #2845, #1038, #15189, #27430, #34568, #20808, #19238, #24833, #9237, #21368, #11481, #28807, #26178, #19307, #25738, #4590, #17480, #20035, #13979, #16323, #33066, #2964, #29583, #29641, #5152, #24564, #4369, #10744, #11048, #9247, #1256, #2604, #8417, #32323, #24366, #12519, #33036, #32270, #29441, #33367, #29845, #17733, #26144, #40643, #12759, #12287, #24123, #9133, #25510, #25044, #30127, #32128, #25304, #8404, #25170, #20313, #16238, #40591, #22625, #8924, #13291, #31641, #10936, #3915, #15758, #5217, #10176, #15060, #18916, #2374, #36656, #2750, #12978, #16525, #5962, #9372, #31520, #15236, #20513, #20459, #27335, #7234, #19296, #34160, #34035, #40441, #40068, #14835, #27356, #37874, #23855, #39825, #23295, #12405, #391, #24610, #15667, #28898, #30526, #22310, #32796, #2623, #32388, #37346, #8119, #38614, #22337, #34560, #19011, #36148, #17619, #30024, #21768, #1948, #17235, #5953, #7357, #29779, #18083, #10629, #16561, #26614, #32845 ) ) ;
#14176 = AXIS2_PLACEMENT_3D ( 'NONE', #9315, #31952, #9734 ) ;
#14177 = EDGE_CURVE ( 'NONE', #16906, #30709, #1008, .T. ) ;
#14178 = FACE_OUTER_BOUND ( 'NONE', #4577, .T. ) ;
#14179 = CARTESIAN_POINT ( 'NONE',  ( 0.1721177234224999797, -1.269400047185449187, -0.7059945205881884567 ) ) ;
#14180 = CARTESIAN_POINT ( 'NONE',  ( 0.04229956186878608415, 0.4429651807893710269, 0.1531492745855134174 ) ) ;
#14181 = CARTESIAN_POINT ( 'NONE',  ( 0.2434700144512876308, -1.137288946556442637, 0.7468722051079026425 ) ) ;
#14182 = LOCAL_TIME ( 0, 53, 7.000000000000000000, #21763 ) ;
#14183 = CARTESIAN_POINT ( 'NONE',  ( 0.1042552114927189771, -1.347860640450032843, -0.3579751000943771633 ) ) ;
#14184 = FACE_OUTER_BOUND ( 'NONE', #27515, .T. ) ;
#14185 = CARTESIAN_POINT ( 'NONE',  ( -0.1743922129835729085, -0.5166151207188712791, 0.3750000000000001110 ) ) ;
#14186 = DIRECTION ( 'NONE',  ( 0.000000000000000000, -3.414809992080327938E-15, -1.000000000000000000 ) ) ;
#14187 = DIRECTION ( 'NONE',  ( -8.881784197001246407E-16, 2.361472542561082612E-16, -1.000000000000000000 ) ) ;
#14188 = EDGE_CURVE ( 'NONE', #32592, #15505, #15415, .T. ) ;
#14189 = CARTESIAN_POINT ( 'NONE',  ( 0.3967966609207765338, -1.138601119762225222, 0.4806637341673061226 ) ) ;
#14190 = DIRECTION ( 'NONE',  ( -1.000000000000000000, -0.000000000000000000, -0.000000000000000000 ) ) ;
#14191 = PERSON_AND_ORGANIZATION ( #28500, #32463 ) ;
#14192 = APPROVAL ( #38421, 'UNSPECIFIED' ) ;
#14193 = CARTESIAN_POINT ( 'NONE',  ( 0.4023555552517616429, -1.144080005235271980, 0.4308225822695866958 ) ) ;
#14194 = DIRECTION ( 'NONE',  ( 1.000000000000000000, 0.000000000000000000, 0.000000000000000000 ) ) ;
#14195 = DIRECTION ( 'NONE',  ( -0.8660512985181119117, -0.4999551463232398962, 0.000000000000000000 ) ) ;
#14196 = CARTESIAN_POINT ( 'NONE',  ( 0.4469283285619459201, -1.099869350908816878, -0.4033480720695140631 ) ) ;
#14197 = CARTESIAN_POINT ( 'NONE',  ( 0.4366310749037827232, -1.106409655742623732, 0.5865638872146798910 ) ) ;
#14198 = CARTESIAN_POINT ( 'NONE',  ( 0.1460529063005417405, -1.108260578017826958, 0.9816109277214414286 ) ) ;
#14199 = CARTESIAN_POINT ( 'NONE',  ( 0.3999999999999787059, -2.183180860297921466, -0.4437760292030870635 ) ) ;
#14200 = EDGE_CURVE ( 'NONE', #14410, #1288, #11479, .T. ) ;
#14201 = ORIENTED_EDGE ( 'NONE', *, *, #17808, .F. ) ;
#14202 = ORIENTED_EDGE ( 'NONE', *, *, #27413, .T. ) ;
#14203 = CARTESIAN_POINT ( 'NONE',  ( 0.1846896762568759620, -0.5250301188136093922, 0.2658526725181787898 ) ) ;
#14204 = ORIENTED_EDGE ( 'NONE', *, *, #25766, .F. ) ;
#14205 = APPLIED_APPROVAL_ASSIGNMENT ( #3604, ( #31951 ) ) ;
#14206 = CARTESIAN_POINT ( 'NONE',  ( 0.05999999999999990757, 0.07140090991423790612, -0.1319162994607513684 ) ) ;
#14207 = CARTESIAN_POINT ( 'NONE',  ( 0.1346587401131250639, -0.5534557573801949237, 0.1697811908328959729 ) ) ;
#14209 = VERTEX_POINT ( 'NONE', #23173 ) ;
#14208 = CARTESIAN_POINT ( 'NONE',  ( 0.007458128862430835580, -0.7676047858832847348, 0.009162072377978345075 ) ) ;
#14210 = AXIS2_PLACEMENT_3D ( 'NONE', #34638, #6435, #31539 ) ;
#14211 = ORIENTED_EDGE ( 'NONE', *, *, #6354, .T. ) ;
#14212 = ADVANCED_BREP_SHAPE_REPRESENTATION ( '', ( #18866, #27819 ), #37726 ) ;
#14213 = CARTESIAN_POINT ( 'NONE',  ( 0.3331429932986941789, -1.175170333239869080, 0.4490264977604416230 ) ) ;
#14214 = ADVANCED_FACE ( 'NONE', ( #35701 ), #25450, .T. ) ;
#14215 = CARTESIAN_POINT ( 'NONE',  ( -0.01398755374478911906, -0.5253281656772126329, 0.1551995070683278577 ) ) ;
#14217 = CARTESIAN_POINT ( 'NONE',  ( 0.1497796767655423800, -1.269200906667645068, 0.6056742027281973861 ) ) ;
#14216 = DIRECTION ( 'NONE',  ( 0.4999551463232372317, -0.8660512985181135770, 0.000000000000000000 ) ) ;
#14218 = CARTESIAN_POINT ( 'NONE',  ( 0.3999999999999786504, -1.971318270955308982, -0.3048432623593835822 ) ) ;
#14219 = ITEM_DEFINED_TRANSFORMATION ( 'NONE', 'NONE', #36406,  #31163 ) ;
#14220 = ADVANCED_FACE ( 'NONE', ( #7507, #12894 ), #29340, .F. ) ;
#14221 = CARTESIAN_POINT ( 'NONE',  ( 0.1909286924077254199, -1.257064795538238577, -0.7137147910238503812 ) ) ;
#14223 = ORIENTED_EDGE ( 'NONE', *, *, #11800, .T. ) ;
#14222 = ORIENTED_EDGE ( 'NONE', *, *, #28342, .T. ) ;
#14224 = EDGE_CURVE ( 'NONE', #36975, #12802, #37111, .T. ) ;
#14225 = CARTESIAN_POINT ( 'NONE',  ( 0.08940417447797945061, -0.7934870992831885017, 0.2534929935647216026 ) ) ;
#14226 = DIRECTION ( 'NONE',  ( -0.4999551463232377313, 0.8660512985181132439, -0.000000000000000000 ) ) ;
#14227 = CARTESIAN_POINT ( 'NONE',  ( 0.1561519734742241317, -0.7461896296692774877, 0.5632227496451408522 ) ) ;
#14228 = CARTESIAN_POINT ( 'NONE',  ( 0.5229475576413166182, -1.460849917182648117, 0.7558602880573046523 ) ) ;
#14229 = CARTESIAN_POINT ( 'NONE',  ( 0.04419567591603339174, -1.150503204610852759, 0.6622665436056601740 ) ) ;
#14230 = FACE_OUTER_BOUND ( 'NONE', #16540, .T. ) ;
#14231 = CARTESIAN_POINT ( 'NONE',  ( 0.6214871112804610798, -1.581993459657260459, 0.4227591190029512114 ) ) ;
#14232 = CARTESIAN_POINT ( 'NONE',  ( 0.3694960952278112942, -1.758893817052062047, -0.4279539500891009762 ) ) ;
#14233 = CARTESIAN_POINT ( 'NONE',  ( 0.4742406144748878005, -1.652140135034469548, -0.3982345435323125238 ) ) ;
#14234 = CIRCLE ( 'NONE', #24763, 0.02999999999999998848 ) ;
#14235 = CARTESIAN_POINT ( 'NONE',  ( 0.5033819511562486193, -1.584744444923489981, -0.5494471831687954833 ) ) ;
#14236 = CARTESIAN_POINT ( 'NONE',  ( 0.3700000000004778355, -2.070564670722348399, -0.2996183892224198453 ) ) ;
#14237 = CARTESIAN_POINT ( 'NONE',  ( 0.3999999999999798161, -2.097675824466503247, -0.2588528740066090017 ) ) ;
#14238 = CARTESIAN_POINT ( 'NONE',  ( 0.01137246303666041881, -0.9338259276304594625, 0.06621170400641679388 ) ) ;
#14239 = EDGE_CURVE ( 'NONE', #18110, #2068, #17408, .T. ) ;
#14240 = CARTESIAN_POINT ( 'NONE',  ( 0.3479125287944198064, -1.635177719134558894, -0.3750029027766745848 ) ) ;
#14241 = APPROVAL_PERSON_ORGANIZATION ( #36431, #16070, #27583 ) ;
#14242 = CARTESIAN_POINT ( 'NONE',  ( 0.006548395810636918092, -0.8294761337169994642, 0.07557146525729462050 ) ) ;
#14243 = CARTESIAN_POINT ( 'NONE',  ( 0.6146019880314795847, -1.612374571812595248, -0.5489582571658230270 ) ) ;
#14244 = CARTESIAN_POINT ( 'NONE',  ( 0.01517484414490882783, -0.7999702980829028753, 0.5364596547344525623 ) ) ;
#14245 = CARTESIAN_POINT ( 'NONE',  ( 0.3394669778924194747, -0.9758008820872865474, 0.6115353432225060226 ) ) ;
#14246 = APPLICATION_PROTOCOL_DEFINITION ( 'international standard', 'automotive_design', 2000, #29256 ) ;
#14247 = CARTESIAN_POINT ( 'NONE',  ( 0.6952872927582756102, -1.427253715223001374, 0.8000406204621429707 ) ) ;
#14248 = ORIENTED_EDGE ( 'NONE', *, *, #676, .T. ) ;
#14249 = CARTESIAN_POINT ( 'NONE',  ( 0.3811251628308331418, -1.654782503697138196, -0.6335434503995733824 ) ) ;
#14250 = CARTESIAN_POINT ( 'NONE',  ( 0.3084692838263019543, -1.760909596431265323, 0.5689466516523863371 ) ) ;
#14251 = ORIENTED_EDGE ( 'NONE', *, *, #31872, .T. ) ;
#14252 = CARTESIAN_POINT ( 'NONE',  ( 0.3391281936521367002, -1.652498152482349880, -0.5834905395359444302 ) ) ;
#14253 = CARTESIAN_POINT ( 'NONE',  ( 0.004762859065977665535, -0.5845126036323667895, 0.3389153922995538082 ) ) ;
#14254 = DIRECTION ( 'NONE',  ( 0.8660512985181133550, 0.4999551463232373427, 0.000000000000000000 ) ) ;
#14256 = ORIENTED_EDGE ( 'NONE', *, *, #26242, .T. ) ;
#14255 = CARTESIAN_POINT ( 'NONE',  ( 0.3484951945142048535, -1.627819363848378220, -0.3328913857909800433 ) ) ;
#14257 = AXIS2_PLACEMENT_3D ( 'NONE', #35597, #3919, #10105 ) ;
#14258 = CARTESIAN_POINT ( 'NONE',  ( 0.09596847297451024938, 0.06113703066755007964, -0.08377772888334847345 ) ) ;
#14259 = CARTESIAN_POINT ( 'NONE',  ( 0.6159793682513172719, -1.299209393623256492, 0.5257027981018284057 ) ) ;
#14261 = ORIENTED_EDGE ( 'NONE', *, *, #13424, .T. ) ;
#14260 = ORIENTED_EDGE ( 'NONE', *, *, #12716, .T. ) ;
#14262 = CARTESIAN_POINT ( 'NONE',  ( 0.1099573354880377524, -1.390855924928339427, -0.6976862894067923371 ) ) ;
#14263 = EDGE_CURVE ( 'NONE', #23421, #36711, #27294, .T. ) ;
#14264 = CARTESIAN_POINT ( 'NONE',  ( 0.3624369654652807027, -1.771784488814728720, -0.5049173149664405447 ) ) ;
#14265 = DIRECTION ( 'NONE',  ( -1.000000000000000000, 0.000000000000000000, 0.000000000000000000 ) ) ;
#14266 = ITEM_DEFINED_TRANSFORMATION ( 'NONE', 'NONE', #14087,  #27819 ) ;
#14267 = ADVANCED_FACE ( 'NONE', ( #13285 ), #779, .T. ) ;
#14268 = CARTESIAN_POINT ( 'NONE',  ( -0.05543910610525212834, 0.4446004295725625166, -0.1230574251923853557 ) ) ;
#14269 = ORIENTED_EDGE ( 'NONE', *, *, #37185, .T. ) ;
#14270 = CARTESIAN_POINT ( 'NONE',  ( 0.2014751060404549599, -1.236718649590243357, 0.5759633585842109937 ) ) ;
#14271 = CARTESIAN_POINT ( 'NONE',  ( 0.09052338057520342707, -0.6901709929874992877, 0.2401866993428223851 ) ) ;
#14272 = CARTESIAN_POINT ( 'NONE',  ( 0.2422216273152858479, -1.437769439691266360, 1.028655097037083799 ) ) ;
#14273 = CARTESIAN_POINT ( 'NONE',  ( 0.09832713360691919258, -0.5593462231477130953, 0.2221295432580932538 ) ) ;
#14275 = CARTESIAN_POINT ( 'NONE',  ( -0.1155415985277060270, -0.5283611291160981160, 0.1337613384747759759 ) ) ;
#14274 = CARTESIAN_POINT ( 'NONE',  ( 0.2546023288931325013, -1.584778239651395859, 0.8703522911872779710 ) ) ;
#14276 = CARTESIAN_POINT ( 'NONE',  ( 0.1143170209530945808, -0.9583121728649094395, 0.4320137086143686633 ) ) ;
#14277 = EDGE_LOOP ( 'NONE', ( #6919, #22576, #5759, #38904, #13560 ) ) ;
#14278 = EDGE_CURVE ( 'NONE', #39344, #25764, #6901, .T. ) ;
#14279 = ORIENTED_EDGE ( 'NONE', *, *, #11773, .F. ) ;
#14280 = DIRECTION ( 'NONE',  ( 0.000000000000000000, 0.000000000000000000, 1.000000000000000000 ) ) ;
#14281 = CARTESIAN_POINT ( 'NONE',  ( 0.2124872757274005319, -0.6329494883420956342, 0.4106774159388293377 ) ) ;
#14282 = CARTESIAN_POINT ( 'NONE',  ( -0.04575334816098036717, 0.2311426348461442515, -0.4288046462019702854 ) ) ;
#14283 = EDGE_CURVE ( 'NONE', #13526, #799, #31222, .T. ) ;
#14284 = CARTESIAN_POINT ( 'NONE',  ( -0.04575334816098059615, -0.4792444552800824153, -0.08732178612071218871 ) ) ;
#14285 = EDGE_CURVE ( 'NONE', #1740, #15439, #7897, .T. ) ;
#14286 = CARTESIAN_POINT ( 'NONE',  ( 0.07244838799016078967, -1.323543130859661465, 0.4946272753632746655 ) ) ;
#14287 = EDGE_CURVE ( 'NONE', #8639, #19627, #39840, .T. ) ;
#14288 = CARTESIAN_POINT ( 'NONE',  ( 0.1913350121442598251, -1.664335509868100527, -0.6864462211259728663 ) ) ;
#14289 = CARTESIAN_POINT ( 'NONE',  ( -0.2399999999999999079, -1.804235510932644004, -0.1501860188971498311 ) ) ;
#14290 = CARTESIAN_POINT ( 'NONE',  ( 0.5591717342432651616, -1.201875270489466407, 0.7301083282254506868 ) ) ;
#14291 = B_SPLINE_SURFACE_WITH_KNOTS ( 'NONE', 3, 3, ( 
 ( #27477, #21522, #2777, #24385, #36920, #27882, #8734, #5653, #30756, #12247, #24807, #37327, #9137, #1320, #17127, #4976, #29677, #14247, #1519, #5365, #30089, #39744, #11578, #26612, #29476, #39148, #1731, #8272, #38929, #7668, #14432, #36460, #29891, #13827, #39527, #14038, #5173, #8468, #26810, #36243, #35854, #2103, #26397, #24140, #1917, #26999, #14640, #7850, #10759, #23331, #21032, #39338, #33555, #11360, #20234, #36051, #11159, #32754, #20636, #8058, #33171, #4558, #23716, #10975, #23533, #20422, #32956, #4761, #17333, #27211, #17543, #23929, #20845, #33365, #17725, #30274, #36662, #31099 ),
 ( #15663, #10048, #18544, #34173, #39946, #31313, #27814, #34380, #24323, #40138, #24532, #11967, #18345, #22620, #33776, #30699, #40555, #24740, #12572, #35153, #38220, #24931, #17930, #28212, #30491, #2919, #5981, #11766, #40349, #5585, #18144, #5788, #15471, #2520, #25689, #2319, #14860, #15059, #21458, #37061, #28023, #2711, #8882, #33983, #30890, #12375, #27609, #37459, #78, #9276, #15255, #21649, #27423, #21852, #36851, #6196, #18764, #8664, #3122, #21239, #12178, #37267, #9083, #13456, #4567, #13645, #26022, #38332, #26411, #3973, #7862, #38542, #4180, #20041, #32970, #35447, #10557, #20433 ),
 ( #26632, #16944, #16339, #10369, #38733, #13243, #16749, #28878, #16536, #736, #10989, #25810, #7248, #22733, #29296, #10164, #35262, #19823, #1144, #7461, #22931, #32356, #29077, #26210, #19629, #38944, #23133, #39160, #17139, #7061, #23546, #23346, #35868, #35659, #13837, #32571, #4388, #29486, #7681, #32164, #36063, #944, #1330, #20246, #10773, #32765, #29691, #1533, #14053, #15070, #11591, #4991, #27623, #11780, #24336, #8289, #2335, #17740, #39761, #21044, #36865, #17348, #24548, #29907, #36256, #8680, #23942, #39351, #20861, #2122, #39959, #40152, #24153, #17558, #18156, #14656, #21255, #11172 ),
 ( #2532, #14259, #36677, #1748, #33382, #30290, #37077, #33792, #17946, #8483, #11982, #5599, #23729, #5185, #20648, #30710, #27225, #8074, #8897, #21469, #30100, #33571, #1931, #14445, #26824, #33187, #4774, #27013, #39540, #11374, #5384, #36476, #30504, #14874, #27435, #28981, #28040, #21869, #27827, #13353, #13566, #18564, #9506, #6974, #31118, #22085, #30903, #10285, #5997, #26133, #15677, #16437, #2932, #22851, #31332, #15489, #15273, #3884, #21659, #38647, #40568, #34397, #37685, #10466, #12387, #28223, #33993, #1057, #6211, #90, #7160, #32259, #5798, #34186, #35172, #24943, #18779, #37470 ),
 ( #4079, #9290, #18356, #3136, #12584, #25928, #2726, #12195, #19546, #845, #25146, #40366, #38451, #32078, #35370, #24754, #19727, #16646, #37276, #9093, #29195, #26314, #29403, #35768, #20762, #32469, #29801, #35559, #39056, #35975, #2028, #11278, #36165, #1643, #5091, #26921, #1247, #10887, #38840, #39451, #26520, #16860, #1841, #14557, #7579, #26732, #20153, #23241, #7356, #19934, #23845, #13748, #27125, #36367, #23457, #10669, #32681, #4487, #39261, #17459, #17050, #7781, #29593, #14357, #39655, #1437, #11084, #7975, #13951, #23645, #4294, #8188, #20350, #23033, #4678, #4892, #32870, #33284 ),
 ( #20549, #17250, #14162, #33082, #30008, #17651, #30197, #39868, #31231, #5896, #27339, #11689, #8386, #21761, #12094, #28139, #8578, #33911, #20954, #40052, #11492, #24243, #24057, #6100, #36583, #2439, #17847, #24444, #33476, #5282, #14976, #36976, #2631, #21155, #5496, #36766, #11875, #14777, #21570, #33684, #34295, #12301, #2237, #18668, #18457, #31010, #27530, #9008, #8796, #5708, #27726, #2831, #30406, #3048, #18063, #30614, #15382, #21374, #18266, #30810, #15167, #27938, #15592, #40261, #24660, #24859, #37191, #40478, #34093, #37379, #9192, #25251, #198, #25041, #37576, #3831, #6315, #4028 ),
 ( #6507, #413, #13098, #12690, #25657, #22796, #604, #12908, #3645, #35319, #16207, #9399, #38188, #28742, #16595, #13302, #7109, #16386, #19285, #25463, #4, #18888, #34702, #34504, #9612, #10014, #19078, #22377, #21975, #31425, #3228, #15777, #28324, #19676, #35112, #37793, #22187, #31617, #10227, #22586, #12484, #3433, #34900, #15991, #28537, #37995, #9805, #6711, #32212, #31826, #6918, #19492, #32023, #28927, #794, #25874, #38389, #20298, #38784, #23191, #1196, #29542, #32420, #39218, #10614, #11224, #29964, #19883, #23791, #36113, #7919, #32632, #26684, #1382, #23410, #4623, #20494, #1001 ) ),
 .UNSPECIFIED., .F., .F., .F.,
 ( 4, 1, 1, 1, 4 ),
 ( 4, 3, 1, 1, 1, 1, 1, 1, 1, 1, 1, 1, 1, 1, 1, 1, 1, 1, 1, 1, 1, 1, 1, 1, 1, 1, 1, 1, 1, 1, 1, 1, 1, 1, 1, 1, 1, 1, 1, 1, 1, 1, 1, 1, 1, 1, 1, 1, 1, 1, 1, 1, 1, 1, 1, 1, 1, 1, 1, 1, 1, 1, 1, 1, 1, 1, 1, 1, 1, 1, 1, 1, 1, 4 ),
 ( 0.000000000000000000, 0.2500000000000000000, 0.5000000000000000000, 0.7500000000000000000, 1.000000000000000000 ),
 ( -0.01000000000000000021, 0.000000000000000000, 0.002255859375000000052, 0.004511718750000000104, 0.006767578124999999722, 0.009023437500000000208, 0.01127929687499999896, 0.01353515624999999944, 0.01579101562499999820, 0.01804687500000000042, 0.02255859374999999792, 0.02707031249999999889, 0.03158203124999999639, 0.03609375000000000083, 0.04060546874999999833, 0.04511718749999999584, 0.04962890625000000028, 0.05414062499999999778, 0.05865234375000000222, 0.06316406249999999278, 0.06767578124999999722, 0.07218750000000000167, 0.07669921874999999223, 0.08121093749999999667, 0.09023437499999999167, 0.09925781250000000056, 0.1082812499999999956, 0.1173046875000000044, 0.1263281249999999856, 0.1353515624999999944, 0.1443750000000000033, 0.1533984374999999845, 0.1624218749999999933, 0.1714453125000000022, 0.1804687499999999833, 0.1894921874999999922, 0.1985156250000000011, 0.2075390624999999822, 0.2165624999999999911, 0.2346093750000000089, 0.2526562499999999711, 0.2707031249999999889, 0.2887500000000000067, 0.3067968749999999689, 0.3248437499999999867, 0.3428906250000000044, 0.3609374999999999667, 0.3789843749999999845, 0.3970312500000000022, 0.4150781249999999645, 0.4331249999999999822, 0.4511718750000000000, 0.4692187500000000178, 0.4872656250000000355, 0.5053124999999999423, 0.5414062499999999778, 0.5775000000000000133, 0.6303124999999999423, 0.6567187500000000178, 0.6831249999999999822, 0.7095312499999999467, 0.7359375000000000222, 0.7623437499999999867, 0.7887500000000000622, 0.8151562500000000266, 0.8415624999999999911, 0.8679687499999999556, 0.8943750000000001421, 0.9207812499999998845, 0.9471875000000000711, 0.9603906250000000533, 0.9735937500000000355, 0.9867968750000000178, 1.000000000000000000 ),
 .UNSPECIFIED. ) ;
#14292 =( BOUNDED_SURFACE ( )  B_SPLINE_SURFACE ( 3, 2, ( 
 ( #31742, #28666, #6835 ),
 ( #6019, #19415, #31950 ),
 ( #18587, #110, #31144 ),
 ( #17689, #29639, #1480 ),
 ( #39913, #7627, #39706 ),
 ( #32916, #10934, #36209 ),
 ( #4726, #30054, #17296 ),
 ( #39107, #8021, #13998 ),
 ( #23290, #5326, #36421 ),
 ( #8433, #1690, #32719 ),
 ( #2285, #23683, #27389 ),
 ( #14208, #17091, #39303 ),
 ( #30235, #17888, #20194 ),
 ( #29850, #20598, #4526 ),
 ( #1884, #26776, #36013 ),
 ( #11124, #26570, #23497 ),
 ( #7818, #20389, #14823 ),
 ( #14395, #33130, #4939 ),
 ( #35813, #17505, #26960 ),
 ( #39493, #11322, #23892 ),
 ( #8232, #27173, #20810 ),
 ( #33328, #30455, #5135 ),
 ( #2066, #14601, #11539 ),
 ( #24104, #36629, #20997 ),
 ( #33518, #36811, #15434 ),
 ( #6158, #5755, #40313 ),
 ( #31278, #31469, #37022 ),
 ( #8625, #30854, #33734 ),
 ( #2881, #6365, #30664 ),
 ( #34344, #8845, #47 ),
 ( #15831, #15217, #24704 ),
 ( #15635, #40097, #15023 ),
 ( #18722, #27574, #11926 ),
 ( #24490, #21196, #22032 ) ),
 .UNSPECIFIED., .F., .F., .T. ) 
 B_SPLINE_SURFACE_WITH_KNOTS ( ( 4, 2, 2, 2, 2, 2, 2, 2, 2, 2, 2, 2, 2, 2, 2, 2, 4 ),
 ( 3, 3 ),
 ( 0.001355756759087015529, 0.002198797089660819298, 0.003041837420234622634, 0.003884877750808425970, 0.004727918081382229305, 0.005570958411956032641, 0.006413998742529836844, 0.007257039073103640180, 0.008100079403677443515, 0.008943119734251245984, 0.009786160064825050187, 0.01062920039539885439, 0.01147224072597265859, 0.01231528105654646280, 0.01315832138712026526, 0.01400136171769406773, 0.01484440204826787194 ),
 ( 0.000000000000000000, 1.000000000000000000 ),
 .UNSPECIFIED. ) 
 GEOMETRIC_REPRESENTATION_ITEM ( )  RATIONAL_B_SPLINE_SURFACE ( (
 ( 1.000000000000000000, 0.7632905047465364801, 1.000000000000000000),
 ( 1.000000000000000000, 0.7632367077656201371, 1.000000000000000000),
 ( 1.000000000000000000, 0.7632388388605254592, 1.000000000000000000),
 ( 1.000000000000000000, 0.7632991344096814457, 1.000000000000000000),
 ( 1.000000000000000000, 0.7633576247790648805, 1.000000000000000000),
 ( 1.000000000000000000, 0.7635011905928678067, 1.000000000000000000),
 ( 1.000000000000000000, 0.7635855781863163383, 1.000000000000000000),
 ( 1.000000000000000000, 0.7637789697554389079, 1.000000000000000000),
 ( 1.000000000000000000, 0.7638898926440848003, 1.000000000000000000),
 ( 1.000000000000000000, 0.7641372409602232851, 1.000000000000000000),
 ( 1.000000000000000000, 0.7642744383510835515, 1.000000000000000000),
 ( 1.000000000000000000, 0.7645793446138899885, 1.000000000000000000),
 ( 1.000000000000000000, 0.7647454238010300553, 1.000000000000000000),
 ( 1.000000000000000000, 0.7650925878231267241, 1.000000000000000000),
 ( 1.000000000000000000, 0.7652762098147284364, 1.000000000000000000),
 ( 1.000000000000000000, 0.7656549625587164565, 1.000000000000000000),
 ( 1.000000000000000000, 0.7658461486473470137, 1.000000000000000000),
 ( 1.000000000000000000, 0.7662298608678012046, 1.000000000000000000),
 ( 1.000000000000000000, 0.7664244233119626992, 1.000000000000000000),
 ( 1.000000000000000000, 0.7667980329912454929, 1.000000000000000000),
 ( 1.000000000000000000, 0.7669780830225270130, 1.000000000000000000),
 ( 1.000000000000000000, 0.7673223890870666253, 1.000000000000000000),
 ( 1.000000000000000000, 0.7674857715588927487, 1.000000000000000000),
 ( 1.000000000000000000, 0.7677804493114095408, 1.000000000000000000),
 ( 1.000000000000000000, 0.7679136995718428560, 1.000000000000000000),
 ( 1.000000000000000000, 0.7681530618753115158, 1.000000000000000000),
 ( 1.000000000000000000, 0.7682555419669827579, 1.000000000000000000),
 ( 1.000000000000000000, 0.7684354526188612589, 1.000000000000000000),
 ( 1.000000000000000000, 0.7685141687395736776, 1.000000000000000000),
 ( 1.000000000000000000, 0.7686421839867699779, 1.000000000000000000),
 ( 1.000000000000000000, 0.7686922298276939181, 1.000000000000000000),
 ( 1.000000000000000000, 0.7687384693205387975, 1.000000000000000000),
 ( 1.000000000000000000, 0.7687334298366129692, 1.000000000000000000),
 ( 1.000000000000000000, 0.7686749430622512591, 1.000000000000000000) ) ) 
 REPRESENTATION_ITEM ( '' )  SURFACE ( )  );
#14293 = LINE ( 'NONE', #33218, #28643 ) ;
#14294 = CARTESIAN_POINT ( 'NONE',  ( -0.08000000000000000167, -1.968175500587574067, -0.6048844944454191408 ) ) ;
#14295 = DIRECTION ( 'NONE',  ( -1.000000000000000000, -7.857794173099924470E-32, -8.628166150854818811E-32 ) ) ;
#14296 = EDGE_LOOP ( 'NONE', ( #34641, #34802, #10428, #33912 ) ) ;
#14297 = LINE ( 'NONE', #26857, #37227 ) ;
#14298 = CARTESIAN_POINT ( 'NONE',  ( -0.02953079040095693900, -0.09152108205202422186, -0.5223162075576424090 ) ) ;
#14299 = CARTESIAN_POINT ( 'NONE',  ( -0.05138886601528206560, -0.2952081121918937456, -0.3684218102521223392 ) ) ;
#14300 = EDGE_LOOP ( 'NONE', ( #14505, #2931, #5097, #10123 ) ) ;
#14301 = CARTESIAN_POINT ( 'NONE',  ( 0.3668321548077844163, -0.9575135872197984011, 0.6682895851757253425 ) ) ;
#14302 = DIRECTION ( 'NONE',  ( 0.4999551463232372317, -0.8660512985181133550, 0.000000000000000000 ) ) ;
#14303 = CARTESIAN_POINT ( 'NONE',  ( 0.06047107820563558944, -0.8445096946280080674, 0.3194460826658605535 ) ) ;
#14304 = ORIENTED_EDGE ( 'NONE', *, *, #9504, .T. ) ;
#14305 = CARTESIAN_POINT ( 'NONE',  ( -0.01895494625228195951, 0.3623053290767001000, 0.3730957266516555793 ) ) ;
#14306 = CARTESIAN_POINT ( 'NONE',  ( 0.03170874437002779017, 0.05432941731172492156, 0.4888251740112576349 ) ) ;
#14307 = CARTESIAN_POINT ( 'NONE',  ( 0.4105658344535222937, -1.676523150947434759, -0.6311718820832802335 ) ) ;
#14308 = CARTESIAN_POINT ( 'NONE',  ( -0.01548846960707490547, 0.09061086148575973886, 0.5171215251571029681 ) ) ;
#14309 = CARTESIAN_POINT ( 'NONE',  ( 0.4691550673861196730, -1.240601932822466003, 0.5838046598153082689 ) ) ;
#14310 = ADVANCED_FACE ( 'NONE', ( #32200 ), #4014, .F. ) ;
#14311 = ADVANCED_FACE ( 'NONE', ( #13684 ), #26249, .F. ) ;
#14313 = FACE_OUTER_BOUND ( 'NONE', #30419, .T. ) ;
#14312 = CARTESIAN_POINT ( 'NONE',  ( 0.3984114568195522010, -1.599003643269838904, -0.5155029497116575543 ) ) ;
#14314 = CARTESIAN_POINT ( 'NONE',  ( 0.5801945607878721267, -1.527237371078230099, -0.5722706679201888802 ) ) ;
#14315 = ORIENTED_EDGE ( 'NONE', *, *, #1200, .F. ) ;
#14316 = EDGE_CURVE ( 'NONE', #9001, #21617, #9539, .T. ) ;
#14317 = LINE ( 'NONE', #35501, #17163 ) ;
#14318 = ORIENTED_EDGE ( 'NONE', *, *, #22230, .T. ) ;
#14319 = CARTESIAN_POINT ( 'NONE',  ( 0.1872963375802847441, -0.4547550531002670371, 0.1015045423513593059 ) ) ;
#14320 = CARTESIAN_POINT ( 'NONE',  ( 0.06072818908143945427, -0.5500858300393093314, 0.2145042832497142393 ) ) ;
#14322 = FACE_BOUND ( 'NONE', #10279, .T. ) ;
#14321 = CARTESIAN_POINT ( 'NONE',  ( 0.08992183057946913360, -0.5436920459133731676, 0.1491868301061692603 ) ) ;
#14323 = VERTEX_POINT ( 'NONE', #23392 ) ;
#14324 = ORIENTED_EDGE ( 'NONE', *, *, #26089, .T. ) ;
#14325 = CARTESIAN_POINT ( 'NONE',  ( 0.1499999999999993561, 0.000000000000000000, 0.000000000000000000 ) ) ;
#14326 = CARTESIAN_POINT ( 'NONE',  ( 0.1260890751152980438, -0.6040517541015768543, 0.3288134516145302944 ) ) ;
#14327 = AXIS2_PLACEMENT_3D ( 'NONE', #14676, #7696, #10792 ) ;
#14328 = EDGE_LOOP ( 'NONE', ( #9956, #18315, #13612, #9849 ) ) ;
#14329 = DIRECTION ( 'NONE',  ( -1.000000000000000000, -7.857794173099924470E-32, -8.628166150854818811E-32 ) ) ;
#14330 = DIRECTION ( 'NONE',  ( -1.000000000000000000, -2.341930812374887555E-31, 1.664003471950578127E-31 ) ) ;
#14331 = CARTESIAN_POINT ( 'NONE',  ( 0.6047424516501676006, -1.591284807845871896, 0.4182417262808776903 ) ) ;
#14332 = CARTESIAN_POINT ( 'NONE',  ( 0.09761789444427076967, -1.310832906678207399, 0.4542993516864344272 ) ) ;
#14333 = DIRECTION ( 'NONE',  ( -0.000000000000000000, -0.000000000000000000, 1.000000000000000000 ) ) ;
#14334 = CARTESIAN_POINT ( 'NONE',  ( 0.08905620747404956183, -0.5633431237458920160, 0.06417412856409884792 ) ) ;
#14335 = CARTESIAN_POINT ( 'NONE',  ( 0.7203159877618242612, -1.479638488134456420, 0.5307775041526673343 ) ) ;
#14336 = CARTESIAN_POINT ( 'NONE',  ( -0.2300000000000000655, 0.5182417262804733804, 0.3749999999999999445 ) ) ;
#14337 = DIRECTION ( 'NONE',  ( 0.000000000000000000, -0.8090169943749496717, -0.5877852522924700285 ) ) ;
#14338 = CARTESIAN_POINT ( 'NONE',  ( 0.6041280778791606743, -1.590911168834266087, -0.4817497659024419510 ) ) ;
#14339 = CARTESIAN_POINT ( 'NONE',  ( 0.05076679145662137127, 0.3165345149637581734, 0.3525336044145316872 ) ) ;
#14340 = CARTESIAN_POINT ( 'NONE',  ( 0.6611009558453398993, -1.574486732712688353, 0.6100612929419876318 ) ) ;
#14341 = DIRECTION ( 'NONE',  ( -1.000000000000000000, -0.000000000000000000, -0.000000000000000000 ) ) ;
#14342 = FACE_OUTER_BOUND ( 'NONE', #8072, .T. ) ;
#14343 = CARTESIAN_POINT ( 'NONE',  ( 0.003338613830247910610, -0.5117837562375455729, 0.3073580953312808339 ) ) ;
#14344 = CARTESIAN_POINT ( 'NONE',  ( 0.5662217921320245040, -1.581573517294255327, -0.5498102858096727275 ) ) ;
#14345 = CARTESIAN_POINT ( 'NONE',  ( 0.000000000000000000, 0.08000000000000023759, 0.000000000000000000 ) ) ;
#14346 = CARTESIAN_POINT ( 'NONE',  ( 0.4578876639573271623, -1.691832011784833334, 0.5885088351307257160 ) ) ;
#14347 = CARTESIAN_POINT ( 'NONE',  ( -0.04947837552028283570, -0.2513950290986461944, 0.4056869761633379867 ) ) ;
#14348 = ORIENTED_EDGE ( 'NONE', *, *, #35406, .T. ) ;
#14349 = CARTESIAN_POINT ( 'NONE',  ( 0.4771029018757274587, -1.092484280813812880, -0.6132796080549755002 ) ) ;
#14350 = CARTESIAN_POINT ( 'NONE',  ( 0.3625960434667522270, -1.762758894398491760, -0.5926935080085824481 ) ) ;
#14351 = ORIENTED_EDGE ( 'NONE', *, *, #30010, .F. ) ;
#14352 = CYLINDRICAL_SURFACE ( 'NONE', #28298, 0.06250000000000000000 ) ;
#14353 = CARTESIAN_POINT ( 'NONE',  ( 0.03174060074383010938, 0.2437182008228720997, -0.4645020220639604069 ) ) ;
#14354 = CARTESIAN_POINT ( 'NONE',  ( 0.4603505868040601023, -1.234063264705831831, 0.7371433527421650256 ) ) ;
#14356 = ORIENTED_EDGE ( 'NONE', *, *, #40303, .F. ) ;
#14355 = CARTESIAN_POINT ( 'NONE',  ( -0.05634307799789435578, 0.4332460723641307077, 0.1515798417490766270 ) ) ;
#14357 = CARTESIAN_POINT ( 'NONE',  ( 0.2316395767834320274, -0.8375294501127626967, 0.4569101180231894821 ) ) ;
#14358 = CARTESIAN_POINT ( 'NONE',  ( 0.001234214386605718763, -1.915398013912305020, -0.3390371575412679528 ) ) ;
#14359 = ORIENTED_EDGE ( 'NONE', *, *, #22736, .T. ) ;
#14360 = DIRECTION ( 'NONE',  ( -1.416619696839553375E-11, -0.5877852522924736922, -0.8090169943749470072 ) ) ;
#14361 = CARTESIAN_POINT ( 'NONE',  ( 0.3271890457909016336, -1.639240316579513301, 0.5762784469172572699 ) ) ;
#14363 = CARTESIAN_POINT ( 'NONE',  ( 0.1153056239832157825, -0.4463068649386734421, 0.1349004977409720973 ) ) ;
#14362 = CARTESIAN_POINT ( 'NONE',  ( 0.7083658949752495992, -1.503526964170632363, 0.5307393902334478497 ) ) ;
#14364 = CARTESIAN_POINT ( 'NONE',  ( 0.4972671625857253974, -1.080199071502573771, 0.5707417262808780478 ) ) ;
#14365 = CARTESIAN_POINT ( 'NONE',  ( -1.019575837292306053, -0.04310840302198148261, 0.09999999999999975575 ) ) ;
#14366 = VERTEX_POINT ( 'NONE', #11420 ) ;
#14367 = EDGE_LOOP ( 'NONE', ( #3841, #39719, #38750, #23469 ) ) ;
#14368 = CARTESIAN_POINT ( 'NONE',  ( 0.02069983512658924232, -1.633280642454262299, -0.6383422127260822698 ) ) ;
#14369 = CARTESIAN_POINT ( 'NONE',  ( 0.04230188431063428012, 0.4483687697007492923, 0.1365048020681075280 ) ) ;
#14370 = CARTESIAN_POINT ( 'NONE',  ( 0.08122039712038266190, -0.8352997518968716673, 0.2480260592104332473 ) ) ;
#14371 = CARTESIAN_POINT ( 'NONE',  ( -0.1684323895664678050, 0.5231977504175353566, 0.3749999999999996669 ) ) ;
#14372 = DIRECTION ( 'NONE',  ( -0.4999551463232373427, 0.8660512985181134660, -0.000000000000000000 ) ) ;
#14373 = CARTESIAN_POINT ( 'NONE',  ( 0.1458957113803953376, -0.9479994470368805493, 0.4102629441475512673 ) ) ;
#14374 = CARTESIAN_POINT ( 'NONE',  ( -0.2746410161513782033, -2.292669950144801572, -0.8383185228372386222 ) ) ;
#14375 = CARTESIAN_POINT ( 'NONE',  ( 0.04582713223189471136, 0.2312054150958161580, -0.4285473768184981935 ) ) ;
#14376 = CARTESIAN_POINT ( 'NONE',  ( 0.6584301050327935334, -1.489287037768582511, 0.4182417262808776903 ) ) ;
#14377 = CARTESIAN_POINT ( 'NONE',  ( -0.08000000000000000167, -1.599201040860868339, 0.1642182323853691728 ) ) ;
#14378 = CALENDAR_DATE ( 2026, 13, 10 ) ;
#14379 = CARTESIAN_POINT ( 'NONE',  ( 0.01941756462488182511, -1.054556591395360732, 0.6186745803816108280 ) ) ;
#14380 = CARTESIAN_POINT ( 'NONE',  ( 0.03664605387828124422, -0.4684681574363452339, 0.1090337349854996613 ) ) ;
#14381 = DIRECTION ( 'NONE',  ( 1.000000000000000000, -0.000000000000000000, -0.000000000000000000 ) ) ;
#14382 = ORIENTED_EDGE ( 'NONE', *, *, #18213, .F. ) ;
#14383 = PRODUCT ( 'pulley bushing', 'pulley bushing', '', ( #22719 ) ) ;
#14384 = CARTESIAN_POINT ( 'NONE',  ( 1.413395339180376537E-05, -0.4273865596755438423, 0.1159049528290725523 ) ) ;
#14385 = CARTESIAN_POINT ( 'NONE',  ( 0.3830122863959673496, -1.758151531859595940, -0.5806909769145761624 ) ) ;
#14386 = CARTESIAN_POINT ( 'NONE',  ( 0.3182145041783619455, -1.756683996043875817, 0.4922019062452683835 ) ) ;
#14387 = DIRECTION ( 'NONE',  ( 1.000000000000000000, 2.043171224247294526E-14, 7.702990362679453920E-16 ) ) ;
#14388 = ORIENTED_EDGE ( 'NONE', *, *, #22629, .F. ) ;
#14389 = ORIENTED_EDGE ( 'NONE', *, *, #31027, .T. ) ;
#14390 = CARTESIAN_POINT ( 'NONE',  ( 0.1869361049589261248, -0.5056481182092611437, 0.1703966547429595357 ) ) ;
#14391 = ORIENTED_EDGE ( 'NONE', *, *, #14563, .T. ) ;
#14392 = CARTESIAN_POINT ( 'NONE',  ( 0.4286120410367322831, -1.695948118333154175, -0.4141277345387682218 ) ) ;
#14394 = ORIENTED_EDGE ( 'NONE', *, *, #29609, .F. ) ;
#14393 = CYLINDRICAL_SURFACE ( 'NONE', #25634, 0.08139150547213666598 ) ;
#14396 = ORIENTED_EDGE ( 'NONE', *, *, #20792, .T. ) ;
#14395 = CARTESIAN_POINT ( 'NONE',  ( 0.008358225017219852657, -0.6771875044183260917, -0.01225903253533247063 ) ) ;
#14397 = B_SPLINE_CURVE_WITH_KNOTS ( 'NONE', 3,
 ( #36889, #8700, #21276, #12003, #33813, #11192, #5619, #17579, #18175, #11395 ),
 .UNSPECIFIED., .F., .F.,
 ( 4, 2, 2, 2, 4 ),
 ( 7.806255641894676664E-18, 0.0004362256165457106902, 0.0008724512330914135742, 0.001308676849637116458, 0.001744902466182819342 ),
 .UNSPECIFIED. ) ;
#14398 = ORIENTED_EDGE ( 'NONE', *, *, #39807, .F. ) ;
#14399 = CARTESIAN_POINT ( 'NONE',  ( 0.3191007316647460068, -1.183265676571765068, 0.4690969661098124965 ) ) ;
#14400 = ORIENTED_EDGE ( 'NONE', *, *, #37284, .F. ) ;
#14401 = EDGE_CURVE ( 'NONE', #25464, #17394, #10195, .T. ) ;
#14402 = CARTESIAN_POINT ( 'NONE',  ( 0.2421644059368991964, -1.556966573662585729, 0.8831382204369367939 ) ) ;
#14404 = CARTESIAN_POINT ( 'NONE',  ( 0.2066987746313611596, -1.235937867595670925, 0.5698435078237830131 ) ) ;
#14403 = FACE_OUTER_BOUND ( 'NONE', #10889, .T. ) ;
#14405 = APPLIED_PERSON_AND_ORGANIZATION_ASSIGNMENT ( #17928, #27812, ( #37152 ) ) ;
#14406 = FACE_OUTER_BOUND ( 'NONE', #27349, .T. ) ;
#14407 = APPROVAL_ROLE ( '' ) ;
#14408 = DIRECTION ( 'NONE',  ( -1.000000000000000000, -0.000000000000000000, -0.000000000000000000 ) ) ;
#14410 = VERTEX_POINT ( 'NONE', #17781 ) ;
#14409 = ORIENTED_EDGE ( 'NONE', *, *, #18042, .T. ) ;
#14411 = CARTESIAN_POINT ( 'NONE',  ( 0.01153542426051554215, -0.8583083583799452354, -0.04937503800822783118 ) ) ;
#14412 = CARTESIAN_POINT ( 'NONE',  ( -0.07216878364870250862, 0.000000000000000000, 0.1249999999999993477 ) ) ;
#14413 = CARTESIAN_POINT ( 'NONE',  ( 0.08281856743603543958, -0.6169226312293338843, 0.3801866279162453566 ) ) ;
#14414 = CARTESIAN_POINT ( 'NONE',  ( 0.1873051443137325467, -0.7000652135061801173, 0.03156626986716101063 ) ) ;
#14415 = CARTESIAN_POINT ( 'NONE',  ( 0.02999607453758957112, -2.087869005097287900, -0.7252195465745518987 ) ) ;
#14416 = CARTESIAN_POINT ( 'NONE',  ( 0.06844213494250783736, -1.327645458249330002, 0.5609147710633128892 ) ) ;
#14417 = CARTESIAN_POINT ( 'NONE',  ( 0.3699434352739217058, -1.746858712014902837, -0.4245076167963743874 ) ) ;
#14418 = CARTESIAN_POINT ( 'NONE',  ( 0.3968489921746024551, -1.715760314589834135, 0.4219785499399157924 ) ) ;
#14419 = CARTESIAN_POINT ( 'NONE',  ( 0.3438206814357017693, -1.630517872472182717, -0.5974003366333684450 ) ) ;
#14420 = DIRECTION ( 'NONE',  ( -0.000000000000000000, 0.9396926207859077618, -0.3420201433256703782 ) ) ;
#14421 = LINE ( 'NONE', #29881, #36385 ) ;
#14422 = CARTESIAN_POINT ( 'NONE',  ( 0.1499999999999993561, 0.000000000000000000, 0.000000000000000000 ) ) ;
#14423 = CARTESIAN_POINT ( 'NONE',  ( 0.3853365039963215777, -1.652093682163138899, -0.3956870249903656767 ) ) ;
#14424 = CARTESIAN_POINT ( 'NONE',  ( 0.000000000000000000, 0.000000000000000000, 0.000000000000000000 ) ) ;
#14425 = CARTESIAN_POINT ( 'NONE',  ( 0.6343156381093978391, -1.595758837318228318, -0.5875140676452393906 ) ) ;
#14426 = EDGE_CURVE ( 'NONE', #26509, #29116, #30338, .T. ) ;
#14427 = CARTESIAN_POINT ( 'NONE',  ( 0.2949815950263163233, -1.721662039081772733, 0.6893651101351793153 ) ) ;
#14428 = B_SPLINE_CURVE_WITH_KNOTS ( 'NONE', 3,
 ( #40391, #33210, #5016, #2150, #11615, #24175, #17583, #25579, #25168, #15511, #534, #40589, #28859, #22108, #12827, #25786, #37708, #38109 ),
 .UNSPECIFIED., .F., .F.,
 ( 4, 2, 2, 2, 2, 2, 2, 2, 4 ),
 ( -0.003133633995111274450, -0.002350221109836769448, -0.001566808224562264446, -0.0007833953392877594443, 1.754598674555754578E-08, 0.0007834304312612518605, 0.001566843316535758163, 0.002350256201810264466, 0.003133669087084770769 ),
 .UNSPECIFIED. ) ;
#14429 = CARTESIAN_POINT ( 'NONE',  ( 0.4515156439561487933, -1.057718100141998407, 0.6525781907329395448 ) ) ;
#14430 = EDGE_CURVE ( 'NONE', #27329, #37901, #17182, .T. ) ;
#14431 = DATE_TIME_ROLE ( 'creation_date' ) ;
#14432 = CARTESIAN_POINT ( 'NONE',  ( 0.5698123312952257935, -1.224001199585974087, 0.8774075775261976906 ) ) ;
#14433 = EDGE_CURVE ( 'NONE', #3591, #849, #28551, .T. ) ;
#14434 = ADVANCED_FACE ( 'NONE', ( #36518 ), #27058, .T. ) ;
#14435 = CARTESIAN_POINT ( 'NONE',  ( 0.4120109984136325343, -1.649442217255613352, -0.6281670533134574574 ) ) ;
#14436 = ADVANCED_FACE ( 'NONE', ( #33423 ), #14708, .F. ) ;
#14437 = CARTESIAN_POINT ( 'NONE',  ( 0.05561310505367213913, 0.02041094169100532082, -0.4604718309744556537 ) ) ;
#14438 = ORIENTED_EDGE ( 'NONE', *, *, #21100, .T. ) ;
#14439 = SPHERICAL_SURFACE ( 'NONE', #32252, 0.01499999999999999944 ) ;
#14440 = CARTESIAN_POINT ( 'NONE',  ( 0.1464017060796926617, -1.195235124438886354, 0.9160713362441239571 ) ) ;
#14441 = CARTESIAN_POINT ( 'NONE',  ( 0.2078177976682006600, -1.286321083125659070, -0.6333872262875119841 ) ) ;
#14443 = ORIENTED_EDGE ( 'NONE', *, *, #2898, .T. ) ;
#14442 = CARTESIAN_POINT ( 'NONE',  ( 0.3922705187144002181, -1.780030872646382489, -0.5047570873693943971 ) ) ;
#14444 = CARTESIAN_POINT ( 'NONE',  ( 0.4887921365776448090, -1.679766821171225999, -0.4193976862638449377 ) ) ;
#14445 = CARTESIAN_POINT ( 'NONE',  ( 0.5675876754196318430, -1.214623637701154335, 0.7236292717493534310 ) ) ;
#14447 = ORIENTED_EDGE ( 'NONE', *, *, #7887, .F. ) ;
#14446 = ORIENTED_EDGE ( 'NONE', *, *, #16968, .T. ) ;
#14448 = CARTESIAN_POINT ( 'NONE',  ( -2.141776632491413013E-14, -2.087870288139423547, -0.7252158372584678325 ) ) ;
#14449 = ORIENTED_EDGE ( 'NONE', *, *, #22629, .T. ) ;
#14450 = DIRECTION ( 'NONE',  ( -1.000000000000000000, -0.000000000000000000, -0.000000000000000000 ) ) ;
#14451 = EDGE_CURVE ( 'NONE', #9282, #10169, #15525, .T. ) ;
#14452 = CARTESIAN_POINT ( 'NONE',  ( 0.4627101603843286615, -1.231251100330559067, 0.6049053019777383966 ) ) ;
#14453 = CALENDAR_DATE ( 2026, 13, 10 ) ;
#14454 = LINE ( 'NONE', #27023, #9294 ) ;
#14455 = EDGE_LOOP ( 'NONE', ( #36631, #9231, #40112, #1800 ) ) ;
#14456 = CARTESIAN_POINT ( 'NONE',  ( -0.2399999999999999079, -3.849534981189179028, -0.3510928155360652503 ) ) ;
#14457 = AXIS2_PLACEMENT_3D ( 'NONE', #10573, #30116, #1947 ) ;
#14458 = CARTESIAN_POINT ( 'NONE',  ( 0.1000922401158252234, -0.7453142721180914254, 0.3380235344004010600 ) ) ;
#14459 = CARTESIAN_POINT ( 'NONE',  ( 0.3063131332306592847, -1.685742840915233964, 0.8776895394429725661 ) ) ;
#14460 = CONICAL_SURFACE ( 'NONE', #38767, 0.4615209409081865166, 1.047197551196599852 ) ;
#14461 = CARTESIAN_POINT ( 'NONE',  ( 0.1615841970432282948, -0.7812715960922147485, 0.6051956874001962472 ) ) ;
#14463 = CARTESIAN_POINT ( 'NONE',  ( 0.2871104898329135402, -1.663473480287219308, 0.5826563087959247822 ) ) ;
#14462 = CARTESIAN_POINT ( 'NONE',  ( 0.2008187405414252891, -1.396362803482375181, 0.9475840340812614615 ) ) ;
#14464 = CARTESIAN_POINT ( 'NONE',  ( 0.08010764652114535367, -1.230296665588101801, 0.6540593777872614201 ) ) ;
#14465 = ORIENTED_EDGE ( 'NONE', *, *, #38413, .F. ) ;
#14466 = ORIENTED_EDGE ( 'NONE', *, *, #22315, .T. ) ;
#14467 = DIRECTION ( 'NONE',  ( 0.000000000000000000, 0.5877852522924910117, -0.8090169943749343506 ) ) ;
#14468 = CARTESIAN_POINT ( 'NONE',  ( 0.3820242417005274560, -0.9048593497249316497, 0.7921066019177993578 ) ) ;
#14469 = CARTESIAN_POINT ( 'NONE',  ( -0.2399999999999999079, -3.253295730098268113, -0.6063490597057096254 ) ) ;
#14470 = CARTESIAN_POINT ( 'NONE',  ( 0.4685868260997171353, -1.116540410224083901, 0.5688321002147588290 ) ) ;
#14471 = CARTESIAN_POINT ( 'NONE',  ( -0.2399999999999999079, -3.961846414800720861, -0.6040940090217902236 ) ) ;
#14472 = DIRECTION ( 'NONE',  ( -1.000000000000000000, -0.000000000000000000, -0.000000000000000000 ) ) ;
#14473 = CARTESIAN_POINT ( 'NONE',  ( 0.1844445096220149738, -1.686387118119738071, -0.6842090968296730136 ) ) ;
#14474 = CARTESIAN_POINT ( 'NONE',  ( 0.3596349888097467029, -1.738430108238112837, -0.5125614369301060291 ) ) ;
#14475 = CARTESIAN_POINT ( 'NONE',  ( 0.6089993539687283963, -1.280207732015472333, 0.6563525730433853456 ) ) ;
#14476 = ADVANCED_FACE ( 'NONE', ( #30552 ), #36910, .T. ) ;
#14477 = DIRECTION ( 'NONE',  ( -1.000000000000000000, -1.450080480853946466E-15, 8.881784197001242463E-16 ) ) ;
#14478 = EDGE_CURVE ( 'NONE', #37277, #27529, #27870, .T. ) ;
#14479 = AXIS2_PLACEMENT_3D ( 'NONE', #13649, #26215, #38738 ) ;
#14480 = CARTESIAN_POINT ( 'NONE',  ( 0.05999999999999990757, -0.01787811284557883421, -0.1489307660662511357 ) ) ;
#14481 = CARTESIAN_POINT ( 'NONE',  ( 0.000000000000000000, 0.5878163732725504298, -0.1704268771689479434 ) ) ;
#14482 = ORIENTED_EDGE ( 'NONE', *, *, #38438, .T. ) ;
#14483 = DIRECTION ( 'NONE',  ( 7.771561172376107616E-16, -7.170354002788761615E-17, 1.000000000000000000 ) ) ;
#14484 = CARTESIAN_POINT ( 'NONE',  ( -0.05562150110511283885, -0.02029635476683529227, -0.4604536315446556838 ) ) ;
#14485 = EDGE_CURVE ( 'NONE', #16906, #20255, #12813, .T. ) ;
#14486 = CARTESIAN_POINT ( 'NONE',  ( 0.6069176374591634948, -1.480164522464830990, 0.5706138896049881559 ) ) ;
#14487 = CIRCLE ( 'NONE', #23064, 0.01499999999999999944 ) ;
#14488 = ORIENTED_EDGE ( 'NONE', *, *, #16453, .F. ) ;
#14489 = CARTESIAN_POINT ( 'NONE',  ( 0.1952262678655195816, -0.8446586641751220315, 0.3137089587960322778 ) ) ;
#14490 = AXIS2_PLACEMENT_3D ( 'NONE', #3238, #15784, #34511 ) ;
#14491 = CARTESIAN_POINT ( 'NONE',  ( 0.4724743651013526557, -1.036800466722356928, -0.6317669042598009765 ) ) ;
#14492 = CARTESIAN_POINT ( 'NONE',  ( 0.1060741297991164983, -1.041550032235545764, 0.7252733955407512090 ) ) ;
#14493 = ORIENTED_EDGE ( 'NONE', *, *, #9719, .T. ) ;
#14494 = LINE ( 'NONE', #30556, #31006 ) ;
#14495 = EDGE_CURVE ( 'NONE', #23348, #25087, #4911, .T. ) ;
#14496 = CARTESIAN_POINT ( 'NONE',  ( 0.05561375719525353534, 0.02040745343124195435, 0.4604703763991767618 ) ) ;
#14497 = EDGE_CURVE ( 'NONE', #37952, #15629, #18744, .T. ) ;
#14498 = CARTESIAN_POINT ( 'NONE',  ( 0.04285640132274045472, -0.4878352195310067252, -0.08281044837501300160 ) ) ;
#14499 = EDGE_CURVE ( 'NONE', #16008, #20283, #614, .T. ) ;
#14500 = CARTESIAN_POINT ( 'NONE',  ( 0.1826252287685201647, -1.735863041130423001, -0.3273879975417062216 ) ) ;
#14501 = CARTESIAN_POINT ( 'NONE',  ( 0.4280344223824243954, -1.180185467868497540, 0.6702189010033869909 ) ) ;
#14503 = CARTESIAN_POINT ( 'NONE',  ( 0.5029219481274004311, -1.126576722786344797, 0.5684425849584162638 ) ) ;
#14502 = DIRECTION ( 'NONE',  ( 0.000000000000000000, 0.000000000000000000, -1.000000000000000000 ) ) ;
#14504 = CARTESIAN_POINT ( 'NONE',  ( -0.2746410161513779258, -3.985676108854518507, -0.6623095129438225648 ) ) ;
#14505 = ORIENTED_EDGE ( 'NONE', *, *, #30515, .F. ) ;
#14506 = EDGE_CURVE ( 'NONE', #2486, #33860, #38794, .T. ) ;
#14507 = DIRECTION ( 'NONE',  ( 1.000000000000000000, 0.000000000000000000, 7.762195515159383243E-16 ) ) ;
#14508 = ORIENTED_EDGE ( 'NONE', *, *, #12809, .F. ) ;
#14509 = CARTESIAN_POINT ( 'NONE',  ( 2.567413883183506000E-16, -0.03000000000000006481, 0.1699999999999995126 ) ) ;
#14510 = EDGE_CURVE ( 'NONE', #40111, #1740, #13814, .T. ) ;
#14511 = CARTESIAN_POINT ( 'NONE',  ( 0.2372522076649659917, -1.104445432429510543, 0.8445417033709822219 ) ) ;
#14513 = CARTESIAN_POINT ( 'NONE',  ( 0.4434606427239963788, -1.107327905743432206, -0.6343696257487794199 ) ) ;
#14512 = CARTESIAN_POINT ( 'NONE',  ( 0.6987147365403517663, -1.542558173564892776, 0.5853929165781885935 ) ) ;
#14514 = CARTESIAN_POINT ( 'NONE',  ( -0.1142670043590670731, -0.4723146173917492918, 0.1178658435937000315 ) ) ;
#14515 = VERTEX_POINT ( 'NONE', #17990 ) ;
#14516 = VECTOR ( 'NONE', #9196, 39.37007874015748854 ) ;
#14517 = FACE_OUTER_BOUND ( 'NONE', #10057, .T. ) ;
#14518 = CARTESIAN_POINT ( 'NONE',  ( 0.5737671756752078522, -1.499224592217952123, 0.5704870461232408596 ) ) ;
#14519 =( REPRESENTATION_RELATIONSHIP ('NONE','NONE', #33020, #30147 ) REPRESENTATION_RELATIONSHIP_WITH_TRANSFORMATION ( #21434 )SHAPE_REPRESENTATION_RELATIONSHIP( ) );
#14520 = EDGE_LOOP ( 'NONE', ( #19738, #3660, #22933, #37892, #35814, #1485, #6547, #19289, #8592 ) ) ;
#14521 = CARTESIAN_POINT ( 'NONE',  ( 0.3225409073800189486, -1.758071532568285633, 0.5684393614938241246 ) ) ;
#14522 = DIRECTION ( 'NONE',  ( 0.000000000000000000, 0.000000000000000000, -1.000000000000000000 ) ) ;
#14523 = AXIS2_PLACEMENT_3D ( 'NONE', #22182, #3640, #31611 ) ;
#14524 =( BOUNDED_SURFACE ( )  B_SPLINE_SURFACE ( 3, 2, ( 
 ( #13885, #20486, #33023 ),
 ( #11219, #36306, #33235 ),
 ( #5042, #26261, #38778 ),
 ( #10608, #30149, #14498 ),
 ( #27064, #23184, #5840 ),
 ( #21097, #2575, #33622 ),
 ( #5235, #17789, #18401 ),
 ( #34237, #15327, #40002 ),
 ( #5435, #39813, #15111 ),
 ( #30558, #11824, #14717 ),
 ( #21703, #17999, #27671 ),
 ( #40203, #30347, #30953 ),
 ( #6047, #33850, #18207 ),
 ( #34039, #2381, #14922 ),
 ( #37134, #36719, #33429 ),
 ( #21312, #24599, #2178 ),
 ( #12039, #27280, #11638 ),
 ( #8947, #24196, #8529 ) ),
 .UNSPECIFIED., .F., .F., .T. ) 
 B_SPLINE_SURFACE_WITH_KNOTS ( ( 4, 2, 2, 2, 2, 2, 2, 2, 4 ),
 ( 3, 3 ),
 ( -0.001532620576208818235, -0.0007637936630077494203, 5.033250193319503164E-06, 0.0007738601633943884266, 0.001542687076595457242, 0.002311513989796526274, 0.003080340902997595089, 0.003849167816198663904, 0.004617994729399732719 ),
 ( 0.000000000000000000, 1.000000000000000000 ),
 .UNSPECIFIED. ) 
 GEOMETRIC_REPRESENTATION_ITEM ( )  RATIONAL_B_SPLINE_SURFACE ( (
 ( 1.000000000000000000, 0.7283825911960469801, 1.000000000000000000),
 ( 1.000000000000000000, 0.7404385082113237315, 1.000000000000000000),
 ( 1.000000000000000000, 0.7521504257739495269, 1.000000000000000000),
 ( 1.000000000000000000, 0.7744497410760391443, 1.000000000000000000),
 ( 1.000000000000000000, 0.7845654757373858867, 1.000000000000000000),
 ( 1.000000000000000000, 0.8022083990892294736, 1.000000000000000000),
 ( 1.000000000000000000, 0.8094167424699034719, 1.000000000000000000),
 ( 1.000000000000000000, 0.8194491993616881409, 1.000000000000000000),
 ( 1.000000000000000000, 0.8220634900780661170, 1.000000000000000000),
 ( 1.000000000000000000, 0.8220705070823304261, 1.000000000000000000),
 ( 1.000000000000000000, 0.8194468812481864317, 1.000000000000000000),
 ( 1.000000000000000000, 0.8094220769838590401, 1.000000000000000000),
 ( 1.000000000000000000, 0.8022659121987882891, 1.000000000000000000),
 ( 1.000000000000000000, 0.7845681159033097707, 1.000000000000000000),
 ( 1.000000000000000000, 0.7744426415185602375, 1.000000000000000000),
 ( 1.000000000000000000, 0.7522890290928357926, 1.000000000000000000),
 ( 1.000000000000000000, 0.7403540167215585388, 1.000000000000000000),
 ( 1.000000000000000000, 0.7283825911960204458, 1.000000000000000000) ) ) 
 REPRESENTATION_ITEM ( '' )  SURFACE ( )  );
#14525 = CARTESIAN_POINT ( 'NONE',  ( 0.6208236476055652986, -1.581963837082470903, 0.4231406649541298859 ) ) ;
#14526 = AXIS2_PLACEMENT_3D ( 'NONE', #7964, #34891, #3040 ) ;
#14527 = CARTESIAN_POINT ( 'NONE',  ( 0.1178701413495470002, -1.287575236778115473, 0.4358679387939850547 ) ) ;
#14528 = AXIS2_PLACEMENT_3D ( 'NONE', #1398, #23813, #11239 ) ;
#14529 = CARTESIAN_POINT ( 'NONE',  ( 0.002304987189221298447, -0.5222059228616647841, 0.1457140420755211052 ) ) ;
#14530 = FACE_OUTER_BOUND ( 'NONE', #8476, .T. ) ;
#14531 = B_SPLINE_CURVE_WITH_KNOTS ( 'NONE', 3,
 ( #38997, #16994, #14104, #7517, #14307, #26679 ),
 .UNSPECIFIED., .F., .F.,
 ( 4, 2, 4 ),
 ( 1.734723475976807480E-18, 0.001056481483988077653, 0.002112962967976153572 ),
 .UNSPECIFIED. ) ;
#14532 = CARTESIAN_POINT ( 'NONE',  ( 0.1875000000000003608, -0.4593131964907914422, 0.1498534765393862711 ) ) ;
#14533 = CARTESIAN_POINT ( 'NONE',  ( 0.3925725722532341089, -1.687157587457473129, -0.6235540241194872380 ) ) ;
#14534 = CARTESIAN_POINT ( 'NONE',  ( -0.1710642718812832863, 0.4986889572247755198, 0.3032895567580813356 ) ) ;
#14535 = EDGE_CURVE ( 'NONE', #23886, #14931, #34494, .T. ) ;
#14536 = CARTESIAN_POINT ( 'NONE',  ( 0.6401971904170186134, -1.582074201254710655, -0.5981628054357688296 ) ) ;
#14537 = CARTESIAN_POINT ( 'NONE',  ( 0.09571836153246564283, -1.423919396819204763, -0.6901719388955009915 ) ) ;
#14538 = CARTESIAN_POINT ( 'NONE',  ( 0.6088579185943825411, -1.605814602209477249, 0.5994446572727915035 ) ) ;
#14539 = EDGE_CURVE ( 'NONE', #11583, #15927, #20713, .T. ) ;
#14540 = PLANE ( 'NONE',  #8704 ) ;
#14541 = CARTESIAN_POINT ( 'NONE',  ( -0.03309057659885111802, 0.4608882367397823532, -0.2425133248664002594 ) ) ;
#14542 = CARTESIAN_POINT ( 'NONE',  ( 0.03474859143381433396, -0.6982915424597320175, 0.6540940360414806420 ) ) ;
#14543 = CARTESIAN_POINT ( 'NONE',  ( 0.5812003729376085115, -1.520186550829109029, -0.4529008768009907815 ) ) ;
#14544 = FACE_OUTER_BOUND ( 'NONE', #39454, .T. ) ;
#14545 = AXIS2_PLACEMENT_3D ( 'NONE', #22047, #6172, #12157 ) ;
#14546 = CARTESIAN_POINT ( 'NONE',  ( 0.4521978803666491520, -1.695070482658580735, 0.5936670903620218098 ) ) ;
#14547 = VERTEX_POINT ( 'NONE', #8720 ) ;
#14548 = CARTESIAN_POINT ( 'NONE',  ( 0.4493096126656548339, -1.113522177362729959, 0.5923215117436996247 ) ) ;
#14549 = CIRCLE ( 'NONE', #2180, 0.005000000000000014849 ) ;
#14550 = CARTESIAN_POINT ( 'NONE',  ( 0.3878029384188880213, -1.139735408412443141, 0.6057421502664560586 ) ) ;
#14551 = DIRECTION ( 'NONE',  ( 0.4999551463232372317, -0.8660512985181135770, 0.000000000000000000 ) ) ;
#14552 = CARTESIAN_POINT ( 'NONE',  ( -0.05283710938261127615, 0.2421875768565603382, -0.4008269984734620928 ) ) ;
#14553 = CIRCLE ( 'NONE', #23128, 0.01500000000000006536 ) ;
#14554 = CARTESIAN_POINT ( 'NONE',  ( 0.5331776585576782912, -1.350023506793375461, 0.6065130868984314194 ) ) ;
#14556 = ORIENTED_EDGE ( 'NONE', *, *, #19142, .F. ) ;
#14555 = CARTESIAN_POINT ( 'NONE',  ( -0.1650539334306601047, 0.4792632177816724126, 0.1214379789123969933 ) ) ;
#14557 = CARTESIAN_POINT ( 'NONE',  ( 0.4199047739250627576, -1.021165802582503890, 0.6853183793762346321 ) ) ;
#14558 = ORIENTED_EDGE ( 'NONE', *, *, #13883, .F. ) ;
#14559 = EDGE_CURVE ( 'NONE', #4225, #1885, #31863, .T. ) ;
#14560 = CARTESIAN_POINT ( 'NONE',  ( 0.01381577305234537624, -1.692631703545224298, -0.3687587685671118720 ) ) ;
#14561 = ORIENTED_EDGE ( 'NONE', *, *, #14934, .T. ) ;
#14562 = CARTESIAN_POINT ( 'NONE',  ( 0.3400028867877604721, -1.710946582846349484, -0.5979181485037454724 ) ) ;
#14563 = EDGE_CURVE ( 'NONE', #19176, #32215, #15712, .T. ) ;
#14564 = CARTESIAN_POINT ( 'NONE',  ( 0.3567070568950239662, -1.622554001505994270, 0.5819357718811433156 ) ) ;
#14566 = CARTESIAN_POINT ( 'NONE',  ( 0.1152431668949159965, -0.4475630518674869607, 0.1186598434184487072 ) ) ;
#14565 = CARTESIAN_POINT ( 'NONE',  ( 0.7091947434576362230, -1.510530529667985178, 0.5453121661639291906 ) ) ;
#14567 = CARTESIAN_POINT ( 'NONE',  ( 0.4559719632891928720, -1.698713290701216350, -0.5155029497116575543 ) ) ;
#14568 = VERTEX_POINT ( 'NONE', #40193 ) ;
#14569 = VECTOR ( 'NONE', #21935, 39.37007874015748143 ) ;
#14570 = ORIENTED_EDGE ( 'NONE', *, *, #3854, .T. ) ;
#14571 = CARTESIAN_POINT ( 'NONE',  ( 0.1909286924077254199, -1.257064795538238577, -0.7137147910238503812 ) ) ;
#14572 = DIRECTION ( 'NONE',  ( -2.563099466555620041E-12, 0.5877852522924830181, 0.8090169943749403458 ) ) ;
#14573 = CARTESIAN_POINT ( 'NONE',  ( 0.1779430133141695625, -1.002639472607745219, 0.7064557712546435386 ) ) ;
#14574 = CARTESIAN_POINT ( 'NONE',  ( -0.1509132741912892484, 0.4664843738648666305, 0.09813923389061192382 ) ) ;
#14575 = VECTOR ( 'NONE', #432, 39.37007874015748143 ) ;
#14576 = DIRECTION ( 'NONE',  ( 1.000000000000000000, 1.195566832711459831E-12, -1.235392033522776487E-12 ) ) ;
#14577 = CARTESIAN_POINT ( 'NONE',  ( 0.5860257985473278364, -1.592810714289450758, 0.4282417262808776437 ) ) ;
#14578 = CIRCLE ( 'NONE', #37567, 0.07999999999999996003 ) ;
#14579 = CARTESIAN_POINT ( 'NONE',  ( 0.3914506609052950670, -1.712970798409825690, 0.5197417262808792238 ) ) ;
#14580 = CIRCLE ( 'NONE', #7340, 2.001558204291732146 ) ;
#14581 = DIRECTION ( 'NONE',  ( -1.000000000000000000, -1.441634041478669458E-15, 8.359771364787550201E-16 ) ) ;
#14582 = DIRECTION ( 'NONE',  ( 1.000000000000000000, 1.373428330785184770E-31, -7.771561172376108602E-16 ) ) ;
#14583 = DIRECTION ( 'NONE',  ( 1.000000000000000000, 8.638708177629562344E-13, -2.382021192243037336E-12 ) ) ;
#14584 = DATE_AND_TIME ( #36399, #13449 ) ;
#14585 = CIRCLE ( 'NONE', #15913, 0.5302738246768103902 ) ;
#14586 = EDGE_CURVE ( 'NONE', #16852, #34414, #20179, .T. ) ;
#14587 = CARTESIAN_POINT ( 'NONE',  ( 0.4767939168565226704, -1.131656391368646597, 0.4766437606999714416 ) ) ;
#14588 = CARTESIAN_POINT ( 'NONE',  ( 0.4609956292016122448, -1.239833488668546480, 0.6057417262809813296 ) ) ;
#14589 = CYLINDRICAL_SURFACE ( 'NONE', #4118, 0.08000000000000000167 ) ;
#14590 = CARTESIAN_POINT ( 'NONE',  ( 0.4264202721361137760, -1.467519734074644200, -0.5166151207188711680 ) ) ;
#14591 = CARTESIAN_POINT ( 'NONE',  ( 0.3864838284833568283, -1.745248947331494493, -0.5867414496849889805 ) ) ;
#14592 = CARTESIAN_POINT ( 'NONE',  ( 0.02557412545052138719, -0.6296114640116060590, 0.6017223022440639779 ) ) ;
#14593 = CARTESIAN_POINT ( 'NONE',  ( 0.03664605387828146627, 0.04106737781738913767, -0.4792329708773127583 ) ) ;
#14594 = VERTEX_POINT ( 'NONE', #37934 ) ;
#14595 = ORIENTED_EDGE ( 'NONE', *, *, #30344, .T. ) ;
#14596 = CARTESIAN_POINT ( 'NONE',  ( 0.1766202724171772875, -0.4927511983303360932, 0.1950252429630008055 ) ) ;
#14597 = EDGE_LOOP ( 'NONE', ( #38798, #38368, #10421, #22992 ) ) ;
#14598 = CARTESIAN_POINT ( 'NONE',  ( 0.4308075356823584112, -1.675781595220191544, -0.4121263904455738647 ) ) ;
#14599 = TOROIDAL_SURFACE ( 'NONE', #22527, 0.6154198107346402491, 0.7750185148639454624 ) ;
#14600 = FACE_OUTER_BOUND ( 'NONE', #2976, .T. ) ;
#14602 = VERTEX_POINT ( 'NONE', #7055 ) ;
#14601 = CARTESIAN_POINT ( 'NONE',  ( 0.0008398931413175443400, -0.6066849459851459958, 0.007899750923771155578 ) ) ;
#14603 = ORIENTED_EDGE ( 'NONE', *, *, #19810, .T. ) ;
#14604 = CARTESIAN_POINT ( 'NONE',  ( 0.1205771420324995152, -0.4915166019810813247, 0.3243857998619378846 ) ) ;
#14605 = AXIS2_PLACEMENT_3D ( 'NONE', #28771, #630, #817 ) ;
#14606 = ORIENTED_EDGE ( 'NONE', *, *, #27835, .T. ) ;
#14607 = CIRCLE ( 'NONE', #27751, 0.009999999999999995004 ) ;
#14608 = CARTESIAN_POINT ( 'NONE',  ( -0.001512435542830417026, -0.5371720154798181879, 0.2089148858682966237 ) ) ;
#14610 = CARTESIAN_POINT ( 'NONE',  ( 0.1287248250748170286, -1.260341800920546484, 0.6227168118355963511 ) ) ;
#14609 = DIRECTION ( 'NONE',  ( 0.000000000000000000, 0.000000000000000000, 1.000000000000000000 ) ) ;
#14611 = B_SPLINE_CURVE_WITH_KNOTS ( 'NONE', 3,
 ( #16432, #13137, #32465, #32074, #19338, #13947, #26515, #39052, #22637, #32254, #35168, #10883 ),
 .UNSPECIFIED., .F., .F.,
 ( 4, 2, 2, 2, 2, 4 ),
 ( 0.000000000000000000, 0.0004057368307213396106, 0.0008114736614426792212, 0.001622947322885360611, 0.002434420984328041892, 0.003245894645770723390 ),
 .UNSPECIFIED. ) ;
#14612 = CARTESIAN_POINT ( 'NONE',  ( -0.2399999999999999079, -2.289343986263487896, -0.6686455968847019316 ) ) ;
#14613 = APPROVAL_STATUS ( 'not_yet_approved' ) ;
#14614 = AXIS2_PLACEMENT_3D ( 'NONE', #36632, #21001, #40102 ) ;
#14615 = CARTESIAN_POINT ( 'NONE',  ( 0.5304035836234874957, -1.638499236635372780, 0.5682417262808785452 ) ) ;
#14617 = ORIENTED_EDGE ( 'NONE', *, *, #32150, .F. ) ;
#14616 = VERTEX_POINT ( 'NONE', #26017 ) ;
#14618 = CARTESIAN_POINT ( 'NONE',  ( 0.3246167692519850156, -1.179669033920380805, 0.5775999012672733413 ) ) ;
#14619 = CARTESIAN_POINT ( 'NONE',  ( 0.2200407913522031411, -1.228412753058486073, 0.5340532311266873444 ) ) ;
#14620 = B_SPLINE_SURFACE_WITH_KNOTS ( 'NONE', 3, 3, ( 
 ( #28736, #25867, #3638, #31420 ),
 ( #598, #25032, #34497, #13092 ),
 ( #3221, #18881, #3426, #405 ),
 ( #12902, #38382, #28317, #3825 ),
 ( #19486, #191, #37785, #12684 ),
 ( #9606, #28132, #19280, #25457 ),
 ( #5009, #37989, #22181, #25650 ) ),
 .UNSPECIFIED., .F., .F., .F.,
 ( 4, 3, 4 ),
 ( 4, 4 ),
 ( -6.200793099907373929, -3.019996348331698499, 0.1608004032439768194 ),
 ( -2.017105796196418055, 1.822539631016510064 ),
 .UNSPECIFIED. ) ;
#14621 = CARTESIAN_POINT ( 'NONE',  ( 0.08992993224852839640, -0.5649945132296568806, 0.1558695816954820679 ) ) ;
#14622 = CARTESIAN_POINT ( 'NONE',  ( 0.1872312464940305565, -0.7051497005520173111, 0.03070732711193139425 ) ) ;
#14623 = CIRCLE ( 'NONE', #35652, 0.06250000000000001388 ) ;
#14624 = DIRECTION ( 'NONE',  ( -1.000000000000000000, -0.000000000000000000, -0.000000000000000000 ) ) ;
#14625 = CARTESIAN_POINT ( 'NONE',  ( -0.2746410161513776482, -3.753843787845913216, -0.2458487048530572650 ) ) ;
#14626 = CARTESIAN_POINT ( 'NONE',  ( 0.4098430630954423282, -1.734253481485309889, -0.4297810291093706048 ) ) ;
#14627 = DIRECTION ( 'NONE',  ( -0.2352930446943608811, 0.000000000000000000, 0.9719244739785378728 ) ) ;
#14628 = CARTESIAN_POINT ( 'NONE',  ( 0.3879575449432583478, -1.659955875966160344, -0.6176084244450742444 ) ) ;
#14629 = CARTESIAN_POINT ( 'NONE',  ( 0.1999999999739020262, -2.089771245945420297, -0.2936552384769813839 ) ) ;
#14630 = CARTESIAN_POINT ( 'NONE',  ( 0.1614670899430008522, -0.7569536277469717245, 0.1022936816274460647 ) ) ;
#14631 = CARTESIAN_POINT ( 'NONE',  ( 0.4378920954596315362, -1.115947916920391636, 0.5895459110645610012 ) ) ;
#14632 = DIRECTION ( 'NONE',  ( 0.000000000000000000, -0.5781348229923760629, 0.8159412518334724362 ) ) ;
#14633 =( NAMED_UNIT ( * ) SI_UNIT ( $, .STERADIAN. ) SOLID_ANGLE_UNIT ( ) );
#14634 = AXIS2_PLACEMENT_3D ( 'NONE', #10694, #32699, #23052 ) ;
#14635 = CARTESIAN_POINT ( 'NONE',  ( 0.1959265899308195724, -1.288818386415671036, -0.7414046965098800568 ) ) ;
#14636 = CARTESIAN_POINT ( 'NONE',  ( 0.2474040834808491629, -1.657462368044302137, 0.5682417262808785452 ) ) ;
#14637 = CARTESIAN_POINT ( 'NONE',  ( 0.4907992349987285730, -1.081537398447262266, 0.5876768462667140147 ) ) ;
#14638 = CARTESIAN_POINT ( 'NONE',  ( 0.01863187058585013059, -0.9402654431934535095, 0.5981457854821163878 ) ) ;
#14639 = COORDINATED_UNIVERSAL_TIME_OFFSET ( 0, 0, .AHEAD. ) ;
#14640 = CARTESIAN_POINT ( 'NONE',  ( 0.3762811493344272451, -0.8989788859175238400, 0.7888608478858359918 ) ) ;
#14641 = AXIS2_PLACEMENT_3D ( 'NONE', #12890, #15148, #18439 ) ;
#14642 = AXIS2_PLACEMENT_3D ( 'NONE', #7393, #13387, #32109 ) ;
#14643 = CYLINDRICAL_SURFACE ( 'NONE', #16885, 0.08000000000000002942 ) ;
#14644 = CARTESIAN_POINT ( 'NONE',  ( 0.05268932808079344193, -0.009140209359764809791, -0.4686105243965638656 ) ) ;
#14645 = AXIS2_PLACEMENT_3D ( 'NONE', #19322, #6346, #3864 ) ;
#14646 = AXIS2_PLACEMENT_3D ( 'NONE', #26049, #38568, #10197 ) ;
#14647 = CARTESIAN_POINT ( 'NONE',  ( -0.3000000000000000999, -3.941790907013290823, -0.4709369376873030477 ) ) ;
#14648 = ORIENTED_EDGE ( 'NONE', *, *, #28629, .F. ) ;
#14649 = CARTESIAN_POINT ( 'NONE',  ( 0.2628772568534702980, -1.648529995711587093, -0.6889491329077820359 ) ) ;
#14650 = CARTESIAN_POINT ( 'NONE',  ( 0.03972200282294607865, -0.8089223363086154306, 0.6796728585062656869 ) ) ;
#14651 = CARTESIAN_POINT ( 'NONE',  ( 0.5883443998395444519, -1.491224512076320341, 0.5816035368030421093 ) ) ;
#14652 = CARTESIAN_POINT ( 'NONE',  ( 0.3751224099013009128, -1.759386797955041937, -0.4365224296969196782 ) ) ;
#14654 = EDGE_LOOP ( 'NONE', ( #32860, #27774, #33295, #17643 ) ) ;
#14653 = CARTESIAN_POINT ( 'NONE',  ( -0.2746410161513770931, -3.525450504378606187, -0.1357627943591874498 ) ) ;
#14655 = CARTESIAN_POINT ( 'NONE',  ( 0.01895884884825209393, 0.3622979475331369326, 0.3730907371368772929 ) ) ;
#14656 = CARTESIAN_POINT ( 'NONE',  ( 0.1906860423535042259, -0.5845769100630294757, 0.1622375173579828633 ) ) ;
#14658 = VERTEX_POINT ( 'NONE', #38325 ) ;
#14657 = ORIENTED_EDGE ( 'NONE', *, *, #3341, .T. ) ;
#14659 = CARTESIAN_POINT ( 'NONE',  ( 0.1312036698469882245, -1.353276179866121032, -0.7088635643309191270 ) ) ;
#14660 = EDGE_LOOP ( 'NONE', ( #2986, #3839, #31931, #98 ) ) ;
#14661 = DIRECTION ( 'NONE',  ( 1.000000000000000000, 2.403560570595280416E-31, 1.417484439069005150E-31 ) ) ;
#14662 = CARTESIAN_POINT ( 'NONE',  ( -0.2399999999999999079, -2.809880844172510272, -0.2480969101616946337 ) ) ;
#14663 = PERSON_AND_ORGANIZATION_ROLE ( 'classification_officer' ) ;
#14664 = VECTOR ( 'NONE', #4566, 39.37007874015748143 ) ;
#14665 = DIRECTION ( 'NONE',  ( 0.000000000000000000, 0.8438867430782092116, 0.5365213554527465956 ) ) ;
#14666 = ORIENTED_EDGE ( 'NONE', *, *, #5882, .T. ) ;
#14667 = CARTESIAN_POINT ( 'NONE',  ( 0.1199147042866572366, -1.258787245233497387, 0.6044491403675849028 ) ) ;
#14668 = EDGE_CURVE ( 'NONE', #33002, #30450, #19218, .T. ) ;
#14669 = CARTESIAN_POINT ( 'NONE',  ( 0.09122731847452461573, -0.7321966631737302222, 0.2618906540905704405 ) ) ;
#14670 = EDGE_CURVE ( 'NONE', #13846, #13090, #37782, .T. ) ;
#14671 = CONICAL_SURFACE ( 'NONE', #19938, 0.1946589359789743512, 1.047197551196599186 ) ;
#14672 = CARTESIAN_POINT ( 'NONE',  ( 0.1822742746219855603, -1.224115163224249736, 1.025352947117986080 ) ) ;
#14673 = AXIS2_PLACEMENT_3D ( 'NONE', #18252, #21358, #33465 ) ;
#14674 = CARTESIAN_POINT ( 'NONE',  ( 0.4973887099434665116, -1.542487569279054505, 0.5723575042553348258 ) ) ;
#14676 = CARTESIAN_POINT ( 'NONE',  ( 0.4712917872827126486, -1.037483146682964819, -0.3984834965322623379 ) ) ;
#14675 = CARTESIAN_POINT ( 'NONE',  ( -0.1533385355407300699, 0.4750492940987078305, 0.3599999999999999867 ) ) ;
#14677 = CARTESIAN_POINT ( 'NONE',  ( 0.02088642212014098221, -0.9663541300412515911, 0.3981965082845343451 ) ) ;
#14678 = EDGE_LOOP ( 'NONE', ( #31632, #10715, #2954 ) ) ;
#14679 = VERTEX_POINT ( 'NONE', #35256 ) ;
#14680 = EDGE_CURVE ( 'NONE', #38085, #38511, #28050, .T. ) ;
#14681 = CARTESIAN_POINT ( 'NONE',  ( 0.05283102792148691718, -0.4560693389104585882, -0.1064538768722001622 ) ) ;
#14682 = CARTESIAN_POINT ( 'NONE',  ( 0.4796154630067505087, -1.077685692966938502, 0.8624841813652754929 ) ) ;
#14683 = EDGE_CURVE ( 'NONE', #9809, #33422, #16334, .T. ) ;
#14684 = VECTOR ( 'NONE', #39793, 39.37007874015748143 ) ;
#14685 = PLANE ( 'NONE',  #20710 ) ;
#14686 = AXIS2_PLACEMENT_3D ( 'NONE', #7842, #8049, #1510 ) ;
#14687 = CYLINDRICAL_SURFACE ( 'NONE', #20591, 0.1000000000000000194 ) ;
#14688 =( LENGTH_UNIT ( ) NAMED_UNIT ( * ) SI_UNIT ( $, .METRE. ) );
#14689 = CARTESIAN_POINT ( 'NONE',  ( 0.3668746095265688067, -1.158496670723085931, 0.4182417262808776903 ) ) ;
#14690 = B_SPLINE_CURVE_WITH_KNOTS ( 'NONE', 3,
 ( #10672, #38651, #7582, #29805, #1844, #30201 ),
 .UNSPECIFIED., .F., .F.,
 ( 4, 2, 4 ),
 ( 0.000000000000000000, 0.5000000000000000000, 1.000000000000000000 ),
 .UNSPECIFIED. ) ;
#14691 = CARTESIAN_POINT ( 'NONE',  ( 0.3872487238088446748, -1.838325393793988516, -0.4833546249010213236 ) ) ;
#14692 = CARTESIAN_POINT ( 'NONE',  ( 0.3097005752544714774, -1.188690221295249039, 0.5001884091346039396 ) ) ;
#14693 = CARTESIAN_POINT ( 'NONE',  ( 0.1906860423535042259, -0.5845769100630294757, 0.1622375173579828633 ) ) ;
#14694 = PERSON_AND_ORGANIZATION ( #28500, #32463 ) ;
#14695 = CARTESIAN_POINT ( 'NONE',  ( 0.4419048264408250715, -1.686280600454902245, 0.4284299735159858291 ) ) ;
#14696 = EDGE_CURVE ( 'NONE', #16266, #5057, #14116, .T. ) ;
#14697 = APPROVAL ( #31358, 'UNSPECIFIED' ) ;
#14698 = B_SPLINE_CURVE_WITH_KNOTS ( 'NONE', 3,
 ( #3297, #19155, #40338, #18532, #12167, #24729, #24922, #22060 ),
 .UNSPECIFIED., .F., .F.,
 ( 4, 2, 2, 4 ),
 ( 0.000000000000000000, 0.0003093940741824799281, 0.0006187881483649598563, 0.001237576296729922098 ),
 .UNSPECIFIED. ) ;
#14699 = VECTOR ( 'NONE', #32628, 39.37007874015748143 ) ;
#14700 = CARTESIAN_POINT ( 'NONE',  ( 0.4738546087217606062, -1.652018268363231845, -0.3975985852014427002 ) ) ;
#14701 = ORIENTED_EDGE ( 'NONE', *, *, #19648, .F. ) ;
#14702 = CARTESIAN_POINT ( 'NONE',  ( 0.4665196626547312708, -1.234810002811577379, 0.6252536019874470608 ) ) ;
#14703 = DIRECTION ( 'NONE',  ( 0.8660512985181142431, 0.4999551463232357884, 0.000000000000000000 ) ) ;
#14704 = CARTESIAN_POINT ( 'NONE',  ( -0.01896968469605425645, -0.3622774521524859126, -0.3730768833943127749 ) ) ;
#14705 = VECTOR ( 'NONE', #8064, 39.37007874015748854 ) ;
#14706 = AXIS2_PLACEMENT_3D ( 'NONE', #28381, #37237, #34139 ) ;
#14707 = ORIENTED_EDGE ( 'NONE', *, *, #22501, .T. ) ;
#14708 = CYLINDRICAL_SURFACE ( 'NONE', #4276, 0.04330708661417343591 ) ;
#14709 = LINE ( 'NONE', #21694, #31801 ) ;
#14710 = EDGE_CURVE ( 'NONE', #34890, #35716, #6441, .T. ) ;
#14711 = CIRCLE ( 'NONE', #957, 0.04500000000000033834 ) ;
#14712 = CARTESIAN_POINT ( 'NONE',  ( 0.2256051981446139942, -1.349927307554772415, 0.5923384359580952108 ) ) ;
#14713 = ORIENTED_EDGE ( 'NONE', *, *, #6921, .F. ) ;
#14714 = CARTESIAN_POINT ( 'NONE',  ( 0.05083665881508980799, 0.2375940621857689505, 0.4096919151850463847 ) ) ;
#14715 = CIRCLE ( 'NONE', #37707, 0.02499999999999993894 ) ;
#14716 = CARTESIAN_POINT ( 'NONE',  ( 0.04946426091937060343, -0.03515176265874975226, 0.4760065386269228260 ) ) ;
#14717 = CARTESIAN_POINT ( 'NONE',  ( 0.05634402396114716882, -0.4332356819307869866, -0.1516051145244172449 ) ) ;
#14718 = CARTESIAN_POINT ( 'NONE',  ( 0.2029880746140099723, -1.647471528829948184, -0.3289985474335726523 ) ) ;
#14719 = CARTESIAN_POINT ( 'NONE',  ( 0.4122725859440758978, -1.161157803837102431, 0.6802704944461144265 ) ) ;
#14721 = LINE ( 'NONE', #12044, #22741 ) ;
#14720 = CARTESIAN_POINT ( 'NONE',  ( 0.3409152363046967782, -1.516880185093673061, -0.4991292961807996531 ) ) ;
#14722 = CARTESIAN_POINT ( 'NONE',  ( 0.01548846960707271452, -0.3688619771572954065, -0.3775276577327018046 ) ) ;
#14723 = ORIENTED_EDGE ( 'NONE', *, *, #26252, .F. ) ;
#14724 = CARTESIAN_POINT ( 'NONE',  ( 0.4076976354719489271, -1.154888438488554270, 0.4182417262808778013 ) ) ;
#14725 = ORIENTED_EDGE ( 'NONE', *, *, #6473, .F. ) ;
#14726 = ADVANCED_BREP_SHAPE_REPRESENTATION ( '', ( #19057, #27819 ), #32382 ) ;
#14727 = EDGE_CURVE ( 'NONE', #22246, #19176, #9881, .T. ) ;
#14728 = DIRECTION ( 'NONE',  ( 1.000000000000000000, -7.000205099780415542E-17, -1.510243460696184374E-15 ) ) ;
#14729 = CARTESIAN_POINT ( 'NONE',  ( 0.06252399284434355387, -0.5703086016868591512, 0.2738859570674773702 ) ) ;
#14731 = CARTESIAN_POINT ( 'NONE',  ( 0.4650133494175291426, -1.133480851973431403, -0.6660426939124520773 ) ) ;
#14730 = DIRECTION ( 'NONE',  ( -1.188678714063518227E-15, 1.000000000000000000, 3.263080277421930985E-16 ) ) ;
#14732 = DIRECTION ( 'NONE',  ( 0.000000000000000000, 0.000000000000000000, -1.000000000000000000 ) ) ;
#14733 = ORIENTED_EDGE ( 'NONE', *, *, #6749, .F. ) ;
#14734 = AXIS2_PLACEMENT_3D ( 'NONE', #34088, #18452, #2827 ) ;
#14735 = ADVANCED_FACE ( 'NONE', ( #28679 ), #23836, .F. ) ;
#14736 = ORIENTED_EDGE ( 'NONE', *, *, #15454, .F. ) ;
#14737 = DIRECTION ( 'NONE',  ( 7.771561172376107616E-16, -7.170354002788761615E-17, 1.000000000000000000 ) ) ;
#14738 = EDGE_CURVE ( 'NONE', #4182, #16208, #20067, .T. ) ;
#14739 = CARTESIAN_POINT ( 'NONE',  ( 0.5686245264436429192, -1.473229231349149293, 0.7026948991434345260 ) ) ;
#14740 = CARTESIAN_POINT ( 'NONE',  ( 0.6611503302885902711, -1.574458991221895143, 0.6100450518719389148 ) ) ;
#14741 = CARTESIAN_POINT ( 'NONE',  ( 0.3178512907186139547, -1.645949601790900774, 0.6057417262800831592 ) ) ;
#14742 = CIRCLE ( 'NONE', #37722, 2.001674066779353556 ) ;
#14743 = VECTOR ( 'NONE', #23189, 39.37007874015748143 ) ;
#14744 = APPLIED_APPROVAL_ASSIGNMENT ( #3655, ( #4217 ) ) ;
#14745 = DIRECTION ( 'NONE',  ( 0.000000000000000000, 0.9901182710308658041, 0.1402348365095101024 ) ) ;
#14746 = CARTESIAN_POINT ( 'NONE',  ( 0.01054817777343857940, -0.5296544771352952319, 0.1457185332388703236 ) ) ;
#14747 = DIRECTION ( 'NONE',  ( -1.000000000000000000, 0.000000000000000000, 0.000000000000000000 ) ) ;
#14748 = VECTOR ( 'NONE', #33402, 39.37007874015748143 ) ;
#14749 = CARTESIAN_POINT ( 'NONE',  ( 0.7218807932984940834, -1.475040712527332376, 0.6299232363116300526 ) ) ;
#14750 = AXIS2_PLACEMENT_3D ( 'NONE', #7382, #4703, #14186 ) ;
#14751 = LINE ( 'NONE', #27096, #39788 ) ;
#14752 = EDGE_CURVE ( 'NONE', #34195, #19133, #25328, .T. ) ;
#14753 = CARTESIAN_POINT ( 'NONE',  ( 0.4849246598550199239, -1.680545844843553516, -0.4179233548962039690 ) ) ;
#14754 = EDGE_CURVE ( 'NONE', #6307, #3320, #13843, .T. ) ;
#14755 = CARTESIAN_POINT ( 'NONE',  ( 0.6367656802301012720, -1.590386864768770225, -0.5922886263717986877 ) ) ;
#14756 = CARTESIAN_POINT ( 'NONE',  ( 0.07358560013947622325, -1.491058954681647286, -0.6787182206095554449 ) ) ;
#14757 = CARTESIAN_POINT ( 'NONE',  ( 0.6013626892431855886, -1.610388389587162239, 0.5938553534641382026 ) ) ;
#14758 = CARTESIAN_POINT ( 'NONE',  ( 0.4040663996170131833, -1.731104159697559597, -0.4314341983484236698 ) ) ;
#14759 = DIRECTION ( 'NONE',  ( 0.4999999999999978351, -0.8322738431953016214, -0.2394164779895580630 ) ) ;
#14760 = CARTESIAN_POINT ( 'NONE',  ( 0.005216780649377962716, -0.5315740328921342295, 0.3610413699792206499 ) ) ;
#14761 = CARTESIAN_POINT ( 'NONE',  ( 0.4040535148563422774, -1.747957131225893246, -0.5919255406249457341 ) ) ;
#14762 = AXIS2_PLACEMENT_3D ( 'NONE', #519, #6413, #22481 ) ;
#14763 = CARTESIAN_POINT ( 'NONE',  ( 0.4162641013412031188, -1.591898979695081096, -0.6171349719147453117 ) ) ;
#14764 = CARTESIAN_POINT ( 'NONE',  ( 0.4124147183372396386, -1.717743792098087141, 0.6107278818000745346 ) ) ;
#14765 = TOROIDAL_SURFACE ( 'NONE', #1630, 1.971674066779348866, 0.02999999999999999889 ) ;
#14766 = AXIS2_PLACEMENT_3D ( 'NONE', #36398, #14583, #8213 ) ;
#14767 = VERTEX_POINT ( 'NONE', #23721 ) ;
#14768 = CARTESIAN_POINT ( 'NONE',  ( 0.4697623592636160361, -1.061459377010899541, -0.6056023639864148711 ) ) ;
#14769 = CIRCLE ( 'NONE', #15416, 0.5215209409081880132 ) ;
#14770 = CARTESIAN_POINT ( 'NONE',  ( 0.3442074111778197776, -1.154923315903912284, 0.6085910790176920493 ) ) ;
#14771 = APPLIED_APPROVAL_ASSIGNMENT ( #14192, ( #11166 ) ) ;
#14772 = CARTESIAN_POINT ( 'NONE',  ( 0.07496066467185190374, -0.5410121364700161140, 0.1458279059002116351 ) ) ;
#14773 = CARTESIAN_POINT ( 'NONE',  ( 0.6374494578080344143, -1.479249556658666087, -0.3955914010212834286 ) ) ;
#14774 = CARTESIAN_POINT ( 'NONE',  ( 0.3335272892300009118, -1.054689036592173945, 0.7480762832650960092 ) ) ;
#14776 = ORIENTED_EDGE ( 'NONE', *, *, #38648, .F. ) ;
#14775 = FACE_OUTER_BOUND ( 'NONE', #655, .T. ) ;
#14777 = CARTESIAN_POINT ( 'NONE',  ( 0.4556897805969272741, -1.061013212638954206, 0.6517789979982376858 ) ) ;
#14778 = VERTEX_POINT ( 'NONE', #17551 ) ;
#14779 = CIRCLE ( 'NONE', #17421, 0.1000000000000000194 ) ;
#14780 = CARTESIAN_POINT ( 'NONE',  ( 0.02999999999997891853, -2.097675824466501915, -0.7286991843995629381 ) ) ;
#14781 = ORIENTED_EDGE ( 'NONE', *, *, #38058, .F. ) ;
#14782 = DIRECTION ( 'NONE',  ( 5.551115123125797493E-17, -5.306893166658304503E-16, -1.000000000000000000 ) ) ;
#14783 = EDGE_LOOP ( 'NONE', ( #31832, #18946 ) ) ;
#14784 = CARTESIAN_POINT ( 'NONE',  ( 0.03572657310119726343, -0.5431789479654421937, 0.2057126367031107406 ) ) ;
#14786 = CARTESIAN_POINT ( 'NONE',  ( 0.1772721291538777444, -0.4572599737788377583, 0.1350242392045666873 ) ) ;
#14785 = CARTESIAN_POINT ( 'NONE',  ( 0.6849494496261877563, -1.512191847840882453, 0.4544522245954892292 ) ) ;
#14787 = DIRECTION ( 'NONE',  ( 0.4999551463232377313, -0.8660512985181132439, -0.000000000000000000 ) ) ;
#14788 = EDGE_CURVE ( 'NONE', #26649, #1394, #8423, .T. ) ;
#14789 = VERTEX_POINT ( 'NONE', #26624 ) ;
#14790 = CARTESIAN_POINT ( 'NONE',  ( 0.4826283266143189810, -1.073631714458713970, 0.6135120272222409632 ) ) ;
#14791 = ORIENTED_EDGE ( 'NONE', *, *, #17013, .T. ) ;
#14792 = FACE_OUTER_BOUND ( 'NONE', #24338, .T. ) ;
#14793 = DIRECTION ( 'NONE',  ( -1.000000000000000000, -0.000000000000000000, -0.000000000000000000 ) ) ;
#14794 = CARTESIAN_POINT ( 'NONE',  ( 0.2812000348737145328, -1.206196182835379993, 0.7249378850271948060 ) ) ;
#14795 = LINE ( 'NONE', #4907, #21826 ) ;
#14796 = CYLINDRICAL_SURFACE ( 'NONE', #25269, 0.08749999999977554899 ) ;
#14797 = CIRCLE ( 'NONE', #38424, 0.09999999999999996392 ) ;
#14798 = VECTOR ( 'NONE', #3967, 39.37007874015748854 ) ;
#14799 = CARTESIAN_POINT ( 'NONE',  ( 0.3917590551332735815, -1.108679468675640933, 0.6260960277489386883 ) ) ;
#14800 = CARTESIAN_POINT ( 'NONE',  ( -1.019575837292303166, -0.04310840302197994911, 0.09999999999999879818 ) ) ;
#14801 = CARTESIAN_POINT ( 'NONE',  ( 0.05283710938261071410, 0.3063690517300499683, -0.3541964274677632529 ) ) ;
#14802 = DIRECTION ( 'NONE',  ( 0.4999551463232372317, -0.8660512985181134660, 0.000000000000000000 ) ) ;
#14803 = CARTESIAN_POINT ( 'NONE',  ( 0.0008242595369169036616, -0.9534780057342879811, 0.2825590231195395652 ) ) ;
#14804 = APPROVAL_STATUS ( 'not_yet_approved' ) ;
#14805 = LOCAL_TIME ( 0, 53, 7.000000000000000000, #38115 ) ;
#14806 = EDGE_CURVE ( 'NONE', #2065, #29183, #5314, .T. ) ;
#14807 = ADVANCED_FACE ( 'NONE', ( #35654 ), #7455, .T. ) ;
#14808 = CARTESIAN_POINT ( 'NONE',  ( 0.4795168759268733649, -1.133137350430038826, 0.4754588475104733480 ) ) ;
#14809 = CARTESIAN_POINT ( 'NONE',  ( 0.5536755335287484314, -1.186494592434074402, 0.6057417262809811076 ) ) ;
#14810 = AXIS2_PLACEMENT_3D ( 'NONE', #2912, #22261, #9878 ) ;
#14811 = LINE ( 'NONE', #5928, #26489 ) ;
#14812 = CARTESIAN_POINT ( 'NONE',  ( 0.01198934593465751479, -0.4904157440881893870, -0.02331765030193806015 ) ) ;
#14813 = DIRECTION ( 'NONE',  ( -1.000000000000000000, -0.000000000000000000, -0.000000000000000000 ) ) ;
#14814 = CARTESIAN_POINT ( 'NONE',  ( 0.2842326993136328195, -1.549395603922531617, -0.7208999815284821144 ) ) ;
#14815 = CARTESIAN_POINT ( 'NONE',  ( 0.4010150227249208443, -1.731699465864716236, -0.5966698157887416754 ) ) ;
#14816 = EDGE_CURVE ( 'NONE', #35064, #1249, #17132, .T. ) ;
#14817 = ORIENTED_EDGE ( 'NONE', *, *, #28069, .T. ) ;
#14818 = ORIENTED_EDGE ( 'NONE', *, *, #31189, .T. ) ;
#14819 = CARTESIAN_POINT ( 'NONE',  ( -0.1081053389377021196, -0.4929871184168310161, 0.1128267017629508567 ) ) ;
#14820 = ORIENTED_EDGE ( 'NONE', *, *, #19696, .T. ) ;
#14821 = PLANE ( 'NONE',  #11853 ) ;
#14822 = CARTESIAN_POINT ( 'NONE',  ( -0.1210148435730082073, -0.5061394519557015359, 0.1438724812235057382 ) ) ;
#14824 = VERTEX_POINT ( 'NONE', #14044 ) ;
#14823 = CARTESIAN_POINT ( 'NONE',  ( -0.0001009439540302022357, -0.6986278422313487724, -0.02210014490066574203 ) ) ;
#14825 = AXIS2_PLACEMENT_3D ( 'NONE', #31996, #16363, #9584 ) ;
#14826 = ORIENTED_EDGE ( 'NONE', *, *, #12521, .T. ) ;
#14827 = DIRECTION ( 'NONE',  ( 1.000000000000000000, 2.280301054154495132E-31, -1.664003471950577689E-31 ) ) ;
#14828 = ORIENTED_EDGE ( 'NONE', *, *, #7706, .F. ) ;
#14829 = CARTESIAN_POINT ( 'NONE',  ( 0.2631915173570256172, -1.522375190849774684, 0.8868596689731271798 ) ) ;
#14831 = CARTESIAN_POINT ( 'NONE',  ( 0.2015425829111033018, -1.236709817947498458, 0.5758929572549138509 ) ) ;
#14830 = CARTESIAN_POINT ( 'NONE',  ( -0.02869942827333538810, -0.4519168387192256664, -0.2102852866807496113 ) ) ;
#14832 = APPLIED_APPROVAL_ASSIGNMENT ( #23717, ( #445 ) ) ;
#14833 = CARTESIAN_POINT ( 'NONE',  ( 0.01548846960707511190, 0.09061086148575973886, 0.5171215251571029681 ) ) ;
#14834 = PERSON_AND_ORGANIZATION ( #11806, #15569 ) ;
#14835 = ADVANCED_FACE ( 'NONE', ( #4768 ), #14439, .T. ) ;
#14836 = EDGE_CURVE ( 'NONE', #38684, #15024, #35393, .T. ) ;
#14837 = DIRECTION ( 'NONE',  ( 0.4999999999999967248, 0.4897188143951006767, -0.7142656948415344598 ) ) ;
#14839 = ORIENTED_EDGE ( 'NONE', *, *, #22051, .F. ) ;
#14838 = ORIENTED_EDGE ( 'NONE', *, *, #12982, .F. ) ;
#14840 = CARTESIAN_POINT ( 'NONE',  ( 0.4191100986681001173, -1.701672718972385701, 0.4233639548768205474 ) ) ;
#14841 = CIRCLE ( 'NONE', #35221, 0.01499999999999999424 ) ;
#14842 = CARTESIAN_POINT ( 'NONE',  ( 0.08108118076421688691, -1.187912308584602616, 0.7629475175450785018 ) ) ;
#14843 = CARTESIAN_POINT ( 'NONE',  ( 0.3061189101312851712, -1.032064364196468631, 0.7779705550342140841 ) ) ;
#14844 = CARTESIAN_POINT ( 'NONE',  ( 0.1874366911980140937, -0.6909370189385394267, 0.04366226709255235927 ) ) ;
#14845 = CYLINDRICAL_SURFACE ( 'NONE', #25135, 0.09249999999977555343 ) ;
#14846 = CARTESIAN_POINT ( 'NONE',  ( -0.01548846960707524721, 0.000000000000000000, 0.000000000000000000 ) ) ;
#14847 = CARTESIAN_POINT ( 'NONE',  ( 0.4030327056923162510, -1.680968334469415737, -0.4031266960524318987 ) ) ;
#14848 = CARTESIAN_POINT ( 'NONE',  ( 0.3866587253291882686, -1.756046511159857770, -0.5714736483329494465 ) ) ;
#14849 = CARTESIAN_POINT ( 'NONE',  ( 0.3672875303838387673, -1.616970901354834789, -0.6123576500872188744 ) ) ;
#14850 = DIRECTION ( 'NONE',  ( -7.771561172376107616E-16, 7.170354002788761615E-17, -1.000000000000000000 ) ) ;
#14851 = CARTESIAN_POINT ( 'NONE',  ( 0.3943456310756559002, -1.717985633627846287, 0.3157417262808776548 ) ) ;
#14852 = CARTESIAN_POINT ( 'NONE',  ( 0.07497864282572899719, -1.322056043867073427, 0.4862695133534066794 ) ) ;
#14853 = CARTESIAN_POINT ( 'NONE',  ( 0.3461375923906637730, -1.629180363267989984, -0.4316302822133540884 ) ) ;
#14854 = CLOSED_SHELL ( 'NONE', ( #187, #2508, #11990, #8397, #31606, #26616, #14311, #30700, #1468, #29761, #10256, #36791, #5139, #20446, #30580, #23117, #1622, #12231, #3651, #21797, #27456, #129, #7923, #8407, #66, #6680, #12497, #9143, #30014, #10202, #29767, #14051, #32416, #15436, #15556, #38884, #7991, #36880, #5618 ) ) ;
#14855 = VECTOR ( 'NONE', #31354, 39.37007874015748143 ) ;
#14856 = CARTESIAN_POINT ( 'NONE',  ( 0.02872242845530403876, -0.2464193076120092529, 0.4721747535844879051 ) ) ;
#14857 = CARTESIAN_POINT ( 'NONE',  ( 0.2890670123411187564, -1.729633309587475187, 0.5682417262808785452 ) ) ;
#14858 = CARTESIAN_POINT ( 'NONE',  ( 0.004642268657786469133, -0.8873649503241693992, 0.4600736514407574029 ) ) ;
#14859 = APPROVAL_STATUS ( 'not_yet_approved' ) ;
#14860 = CARTESIAN_POINT ( 'NONE',  ( 0.4993356427094534644, -1.110845742389603430, 0.8468575151840780357 ) ) ;
#14861 = SECURITY_CLASSIFICATION ( '', '', #31514 ) ;
#14862 = EDGE_CURVE ( 'NONE', #39495, #6499, #39481, .T. ) ;
#14863 = CARTESIAN_POINT ( 'NONE',  ( 0.3740960844805631957, -1.108072201694596526, 0.5182417262812423209 ) ) ;
#14864 = CIRCLE ( 'NONE', #36567, 0.9087847906030128708 ) ;
#14865 = CARTESIAN_POINT ( 'NONE',  ( 0.05279755784604349411, -0.03988345070377457419, -0.4667183143801711398 ) ) ;
#14866 = CARTESIAN_POINT ( 'NONE',  ( 0.4867251962510119045, -1.680960026995096612, -0.6125153944539966089 ) ) ;
#14867 = VERTEX_POINT ( 'NONE', #39953 ) ;
#14868 = CARTESIAN_POINT ( 'NONE',  ( 0.6505987497515465234, -1.453420545349225712, 0.4198196556257698941 ) ) ;
#14869 = CARTESIAN_POINT ( 'NONE',  ( 0.1737062342642059776, -1.287475063264992503, 0.9337216465431702472 ) ) ;
#14870 = CARTESIAN_POINT ( 'NONE',  ( 0.5876579976468534472, -1.491161407508044157, 0.5680417111487973125 ) ) ;
#14871 = CARTESIAN_POINT ( 'NONE',  ( 0.3812071769896464013, -1.763750790280049996, -0.4536492913030988894 ) ) ;
#14873 = ORIENTED_EDGE ( 'NONE', *, *, #17074, .F. ) ;
#14872 = CARTESIAN_POINT ( 'NONE',  ( 0.5264113014007612001, -1.640729993778266893, -0.5166151207188711680 ) ) ;
#14874 = CARTESIAN_POINT ( 'NONE',  ( 0.5008076730341156635, -1.117067070538257489, 0.7495569431474730093 ) ) ;
#14876 = ORIENTED_EDGE ( 'NONE', *, *, #10472, .F. ) ;
#14875 = ORIENTED_EDGE ( 'NONE', *, *, #38667, .T. ) ;
#14877 = CARTESIAN_POINT ( 'NONE',  ( 0.6867278559859741893, -1.412191411537361274, 0.7037197479575562076 ) ) ;
#14878 = CARTESIAN_POINT ( 'NONE',  ( 0.1499999999999996336, -0.09061086148575810129, -0.5171215251571033011 ) ) ;
#14879 = DIRECTION ( 'NONE',  ( 0.8660512985181136880, 0.4999551463232368431, 0.000000000000000000 ) ) ;
#14880 = COORDINATED_UNIVERSAL_TIME_OFFSET ( 0, 0, .AHEAD. ) ;
#14881 = PLANE ( 'NONE',  #36226 ) ;
#14882 = ORIENTED_EDGE ( 'NONE', *, *, #11247, .F. ) ;
#14883 = AXIS2_PLACEMENT_3D ( 'NONE', #14567, #9202, #37200 ) ;
#14884 = CARTESIAN_POINT ( 'NONE',  ( 0.2472658003028177509, -0.9389390588893103962, 0.6883636664316881149 ) ) ;
#14885 = CARTESIAN_POINT ( 'NONE',  ( 0.3871723776641498027, -1.623769666286883462, -0.3715740632108985864 ) ) ;
#14886 = CARTESIAN_POINT ( 'NONE',  ( 0.4981291757010007371, -1.537019023564916820, 0.6523613731338329114 ) ) ;
#14888 = CARTESIAN_POINT ( 'NONE',  ( -0.2399999999999999079, -4.056386786973173564, -0.6915988348251679296 ) ) ;
#14887 = CARTESIAN_POINT ( 'NONE',  ( 0.3305348052992108654, -1.762648515960067330, 0.4809830086422206552 ) ) ;
#14889 = CARTESIAN_POINT ( 'NONE',  ( 0.09805242145838187484, -1.310054031134214814, 0.5767050436540001046 ) ) ;
#14890 = FACE_OUTER_BOUND ( 'NONE', #19623, .T. ) ;
#14891 = VERTEX_POINT ( 'NONE', #27822 ) ;
#14892 = EDGE_LOOP ( 'NONE', ( #28386, #9613, #35657, #15036 ) ) ;
#14893 = FACE_OUTER_BOUND ( 'NONE', #2038, .T. ) ;
#14894 = CARTESIAN_POINT ( 'NONE',  ( 0.2142115587710679836, -0.7293689487072348987, 0.6843368706038465143 ) ) ;
#14895 = VECTOR ( 'NONE', #39134, 39.37007874015748143 ) ;
#14896 = CARTESIAN_POINT ( 'NONE',  ( 0.4052030310269085223, -1.718765290342715080, -0.6036971404997847346 ) ) ;
#14897 = DIRECTION ( 'NONE',  ( 0.4999999999999982792, 0.4254978411528176907, 0.7542887956043713427 ) ) ;
#14898 = CARTESIAN_POINT ( 'NONE',  ( 0.3994099251164126563, -1.146822512724485765, 0.4244458817396841166 ) ) ;
#14899 = CARTESIAN_POINT ( 'NONE',  ( 0.02910065466421945385, -1.575914851856258014, -0.6367838632993687575 ) ) ;
#14900 = CARTESIAN_POINT ( 'NONE',  ( 0.3219460272232844700, -1.170076428657419454, 0.4747704893780865798 ) ) ;
#14901 = CARTESIAN_POINT ( 'NONE',  ( 0.5537997781288683807, -1.186498928682228504, 0.6031466697272260813 ) ) ;
#14902 = DATE_AND_TIME ( #15305, #24689 ) ;
#14903 = DIRECTION ( 'NONE',  ( 0.000000000000000000, 0.000000000000000000, -1.000000000000000000 ) ) ;
#14904 = AXIS2_PLACEMENT_3D ( 'NONE', #34272, #9787, #12466 ) ;
#14905 = CARTESIAN_POINT ( 'NONE',  ( 0.1971914821640197435, -2.028516189135913361, -0.6778075598240375088 ) ) ;
#14906 = ADVANCED_FACE ( 'NONE', ( #11771 ), #2327, .F. ) ;
#14907 = CARTESIAN_POINT ( 'NONE',  ( 0.4459262886234038326, -1.207765542572133421, 0.6882926990457565175 ) ) ;
#14908 = EDGE_CURVE ( 'NONE', #29794, #24718, #1402, .T. ) ;
#14909 = DIRECTION ( 'NONE',  ( 0.000000000000000000, 2.106022274728121591E-16, 1.000000000000000000 ) ) ;
#14910 = CIRCLE ( 'NONE', #29720, 0.01499999999999995955 ) ;
#14911 = VERTEX_POINT ( 'NONE', #31323 ) ;
#14912 = CARTESIAN_POINT ( 'NONE',  ( 0.4434255849441152142, -1.139149627293542189, 0.4381544910599347586 ) ) ;
#14913 = ADVANCED_FACE ( 'NONE', ( #24331 ), #21654, .F. ) ;
#14914 = DIRECTION ( 'NONE',  ( 1.000000000000000000, 0.000000000000000000, 0.000000000000000000 ) ) ;
#14915 = VERTEX_POINT ( 'NONE', #2718 ) ;
#14916 = CARTESIAN_POINT ( 'NONE',  ( -0.05616044724337275473, -0.01023656896654600613, -0.4592816919116775587 ) ) ;
#14917 = ADVANCED_FACE ( 'NONE', ( #30898 ), #19790, .F. ) ;
#14918 = CARTESIAN_POINT ( 'NONE',  ( 0.02310847749635362366, -0.8913551796067988864, 0.5089986389165233049 ) ) ;
#14919 = VERTEX_POINT ( 'NONE', #18151 ) ;
#14920 = CARTESIAN_POINT ( 'NONE',  ( -0.01895884884825269415, 0.2428741539084925405, 0.4598572020609172362 ) ) ;
#14921 = CARTESIAN_POINT ( 'NONE',  ( 0.05268932808079455909, 0.009140209359766384919, 0.4686105243965638656 ) ) ;
#14922 = CARTESIAN_POINT ( 'NONE',  ( 0.04575185649130682902, -0.4390455249589713116, -0.2110526333698215518 ) ) ;
#14923 = FACE_OUTER_BOUND ( 'NONE', #11337, .T. ) ;
#14924 = CARTESIAN_POINT ( 'NONE',  ( 0.4084052577889880076, -1.157625084686668693, 0.6947072065425384801 ) ) ;
#14926 = CARTESIAN_POINT ( 'NONE',  ( 0.2059273467974225835, -1.283046334493782359, -0.2869361388274796476 ) ) ;
#14925 = DIRECTION ( 'NONE',  ( -6.162975822039154730E-33, 0.000000000000000000, -1.000000000000000000 ) ) ;
#14927 = CARTESIAN_POINT ( 'NONE',  ( -0.03654364704248898310, -0.3642884434512972947, -0.3592365245254302009 ) ) ;
#14928 = VERTEX_POINT ( 'NONE', #5990 ) ;
#14929 = ORIENTED_EDGE ( 'NONE', *, *, #17641, .T. ) ;
#14930 = CARTESIAN_POINT ( 'NONE',  ( -0.05464101615137786222, -2.321277022828569958, -0.5785054236952983375 ) ) ;
#14931 = VERTEX_POINT ( 'NONE', #24748 ) ;
#14932 = LINE ( 'NONE', #33635, #25971 ) ;
#14933 = CARTESIAN_POINT ( 'NONE',  ( 0.4421500455968371268, -1.573867983067024356, 0.5805441873791059582 ) ) ;
#14934 = EDGE_CURVE ( 'NONE', #14004, #14616, #5592, .T. ) ;
#14936 = CARTESIAN_POINT ( 'NONE',  ( 0.5792545670597167851, -1.619325922623725988, 0.4680594544321094452 ) ) ;
#14935 = DIRECTION ( 'NONE',  ( 1.000000000000000000, -0.000000000000000000, -0.000000000000000000 ) ) ;
#14937 = DIRECTION ( 'NONE',  ( 1.000000000000000000, 0.000000000000000000, 0.000000000000000000 ) ) ;
#14938 = APPLIED_PERSON_AND_ORGANIZATION_ASSIGNMENT ( #3350, #35437, ( #36468 ) ) ;
#14939 = ORIENTED_EDGE ( 'NONE', *, *, #33344, .T. ) ;
#14940 = CARTESIAN_POINT ( 'NONE',  ( -0.1743922129835737966, -0.5166151207188712791, 0.08499999999999977018 ) ) ;
#14941 = ORIENTED_EDGE ( 'NONE', *, *, #16235, .F. ) ;
#14942 = CARTESIAN_POINT ( 'NONE',  ( 0.4053854983667099510, -1.732300422170438559, -0.5284674333234674615 ) ) ;
#14943 = CARTESIAN_POINT ( 'NONE',  ( 0.5738275230768540291, -1.499242471352824069, 0.5716642358389814049 ) ) ;
#14944 = CARTESIAN_POINT ( 'NONE',  ( 0.4880938837017151366, -1.659832216460053189, 0.5158750058761750745 ) ) ;
#14945 = CYLINDRICAL_SURFACE ( 'NONE', #22011, 0.06249999999999997918 ) ;
#14946 = CARTESIAN_POINT ( 'NONE',  ( -0.01548846960721204577, 0.5203207976464816475, 0.08861466064783131424 ) ) ;
#14947 = CARTESIAN_POINT ( 'NONE',  ( 0.2059273467974223892, -1.283046334493782137, -0.3614788220720648870 ) ) ;
#14948 = CARTESIAN_POINT ( 'NONE',  ( 0.2989471840069001241, -1.160067769014730521, -0.5155029497116575543 ) ) ;
#14949 = DIRECTION ( 'NONE',  ( -1.000000000000000000, 0.000000000000000000, 0.000000000000000000 ) ) ;
#14950 = CIRCLE ( 'NONE', #33353, 0.2499999999999999445 ) ;
#14951 = CARTESIAN_POINT ( 'NONE',  ( 0.2433107440384445208, -0.6632537007949954599, 0.5455544552538778014 ) ) ;
#14952 = CARTESIAN_POINT ( 'NONE',  ( -0.05078493045284410146, 0.3164574661091585361, 0.3525385122722583531 ) ) ;
#14953 = CARTESIAN_POINT ( 'NONE',  ( 0.007094984414204748985, -0.9940037754512424106, 0.4883039338829347487 ) ) ;
#14954 = CARTESIAN_POINT ( 'NONE',  ( 0.6418861098210334459, -1.577688375363704099, -0.6007762697806591223 ) ) ;
#14955 = CARTESIAN_POINT ( 'NONE',  ( 0.4259519167603003642, -1.697610851774717267, -0.6162422480182934148 ) ) ;
#14956 = LINE ( 'NONE', #11471, #4361 ) ;
#14957 = FACE_BOUND ( 'NONE', #20264, .T. ) ;
#14958 = CARTESIAN_POINT ( 'NONE',  ( -0.2746410161513776482, -3.941790907013290823, -0.4709369376873030477 ) ) ;
#14959 = EDGE_CURVE ( 'NONE', #4497, #7711, #27094, .T. ) ;
#14960 = ORIENTED_EDGE ( 'NONE', *, *, #35682, .T. ) ;
#14961 = DIRECTION ( 'NONE',  ( -0.9378410757839563683, -0.2807814858886553133, -0.2039996905746434552 ) ) ;
#14962 = EDGE_CURVE ( 'NONE', #9596, #16265, #8672, .T. ) ;
#14963 = CARTESIAN_POINT ( 'NONE',  ( 0.1176586183174064548, -1.298913320427260265, 0.5281503409082900502 ) ) ;
#14964 = EDGE_CURVE ( 'NONE', #18164, #38792, #21250, .T. ) ;
#14965 = CARTESIAN_POINT ( 'NONE',  ( 0.4781934768423681814, -1.682642038360963710, -0.6151431148613258904 ) ) ;
#14966 = EDGE_CURVE ( 'NONE', #14101, #1197, #5377, .T. ) ;
#14968 = ORIENTED_EDGE ( 'NONE', *, *, #7672, .F. ) ;
#14967 = B_SPLINE_SURFACE_WITH_KNOTS ( 'NONE', 3, 3, ( 
 ( #16869, #12472, #25027, #21560 ),
 ( #398, #22176, #21963, #18874 ),
 ( #31413, #3216, #34689, #6494 ),
 ( #12896, #34079, #39569, #5817 ),
 ( #15297, #5624, #30731, #18376 ),
 ( #1955, #27038, #12217, #33597 ),
 ( #18180, #23970, #39783, #30531 ) ),
 .UNSPECIFIED., .F., .F., .F.,
 ( 4, 3, 4 ),
 ( 4, 4 ),
 ( 0.7035562186971585641, 0.8517781093485792265, 1.000000000000000000 ),
 ( 0.4463408799211898148, 0.5556952876593606039 ),
 .UNSPECIFIED. ) ;
#14969 = CARTESIAN_POINT ( 'NONE',  ( 0.1826134026666640375, -1.261648033191452578, 0.4282186462236585722 ) ) ;
#14970 = CYLINDRICAL_SURFACE ( 'NONE', #19090, 0.1000000000000000194 ) ;
#14971 = CARTESIAN_POINT ( 'NONE',  ( -0.2300000000000004818, 0.5182417262804733804, 0.3599999999999999867 ) ) ;
#14972 = LINE ( 'NONE', #14158, #2233 ) ;
#14973 = CARTESIAN_POINT ( 'NONE',  ( 0.5093083032388259213, -1.308138162599655541, 0.6666047094510684223 ) ) ;
#14975 = ORIENTED_EDGE ( 'NONE', *, *, #34844, .F. ) ;
#14974 = DIRECTION ( 'NONE',  ( -1.000000000000000000, -6.779273404243070203E-32, -4.314083075427408311E-32 ) ) ;
#14976 = CARTESIAN_POINT ( 'NONE',  ( 0.4829770732687932999, -1.083865320555347678, 0.6394302686688468906 ) ) ;
#14977 = ORIENTED_EDGE ( 'NONE', *, *, #2377, .T. ) ;
#14978 = APPROVAL_DATE_TIME ( #37578, #28494 ) ;
#14979 = AXIS2_PLACEMENT_3D ( 'NONE', #421, #25470, #32426 ) ;
#14980 = CARTESIAN_POINT ( 'NONE',  ( -0.2399999999999999079, -2.253314830856113726, -0.6753616220517687507 ) ) ;
#14981 = VERTEX_POINT ( 'NONE', #40145 ) ;
#14982 = CARTESIAN_POINT ( 'NONE',  ( 0.3560528695691858592, -1.750603236759655568, -0.5461972732282710519 ) ) ;
#14983 = CARTESIAN_POINT ( 'NONE',  ( 0.3067833816315509443, -1.474156006046335676, 0.8783781600432545300 ) ) ;
#14984 = EDGE_CURVE ( 'NONE', #11891, #6348, #30705, .T. ) ;
#14986 = CARTESIAN_POINT ( 'NONE',  ( 0.1142304224324458134, -0.5268503339532456531, -0.03412200579080372498 ) ) ;
#14985 = CARTESIAN_POINT ( 'NONE',  ( 0.06603965020215776804, -0.7527310131072945110, 0.01289759490777755632 ) ) ;
#14987 = CARTESIAN_POINT ( 'NONE',  ( 0.4909801108973092520, -1.199306193601649362, -0.5155029497116575543 ) ) ;
#14988 = EDGE_LOOP ( 'NONE', ( #31762, #6726, #20042, #13400, #8682, #19538, #38207, #5480, #17881, #20801, #11075, #12954 ) ) ;
#14989 = ORIENTED_EDGE ( 'NONE', *, *, #25537, .F. ) ;
#14990 = CARTESIAN_POINT ( 'NONE',  ( 0.3256465291941874063, -0.9849688007361252495, 0.5834247550187220410 ) ) ;
#14991 = CARTESIAN_POINT ( 'NONE',  ( 0.3411737120602144624, -1.136299044918231527, 0.8205066405080015945 ) ) ;
#14992 = ORIENTED_EDGE ( 'NONE', *, *, #1175, .F. ) ;
#14993 = CARTESIAN_POINT ( 'NONE',  ( 0.3299395734357897791, -1.474170237420246332, -0.3144976166544465324 ) ) ;
#14994 = CARTESIAN_POINT ( 'NONE',  ( -0.01548846960707517956, -0.2306506793134055211, -0.4716198300880352634 ) ) ;
#14995 = CARTESIAN_POINT ( 'NONE',  ( 0.3280405094088094109, -1.284529511138909230, 0.6184389781141244047 ) ) ;
#14996 = CARTESIAN_POINT ( 'NONE',  ( 0.5755462064585110671, -1.567046512275164671, -0.4467185635149386047 ) ) ;
#14997 = CARTESIAN_POINT ( 'NONE',  ( -0.1044436713285788743, -0.4741860147766047695, 0.3472338286680826669 ) ) ;
#14998 = CARTESIAN_POINT ( 'NONE',  ( 5.463695987328526437E-16, -0.2899999999999993694, -7.171100983368691195E-16 ) ) ;
#14999 = CARTESIAN_POINT ( 'NONE',  ( 0.7472019744968698696, -1.513150647243692637, 0.5707417262808793801 ) ) ;
#15000 = CARTESIAN_POINT ( 'NONE',  ( 0.1399999999999994582, -3.326417233800878524E-17, -0.1250000000000000000 ) ) ;
#15001 = DIRECTION ( 'NONE',  ( -1.000000000000000000, -0.000000000000000000, -0.000000000000000000 ) ) ;
#15002 = DIRECTION ( 'NONE',  ( 0.000000000000000000, 0.000000000000000000, -1.000000000000000000 ) ) ;
#15003 = CALENDAR_DATE ( 2026, 13, 10 ) ;
#15004 = CARTESIAN_POINT ( 'NONE',  ( 0.4681739163933527070, -1.133581507510084796, 0.4638371986610853592 ) ) ;
#15005 = CARTESIAN_POINT ( 'NONE',  ( 0.03868649100028075105, -0.4624880946332521336, 0.1149381524902348961 ) ) ;
#15006 = TOROIDAL_SURFACE ( 'NONE', #24862, 0.05330708661417342398, 0.01000000000000000021 ) ;
#15007 = CARTESIAN_POINT ( 'NONE',  ( -0.2343922129835735724, -0.5166151207188712791, 0.09999999999999967248 ) ) ;
#15008 = EDGE_CURVE ( 'NONE', #33383, #32917, #22162, .T. ) ;
#15009 = CARTESIAN_POINT ( 'NONE',  ( 8.003345398980878371E-06, -0.5705062560190085064, -0.08785543567291767553 ) ) ;
#15010 = DIRECTION ( 'NONE',  ( 1.972152263052529514E-31, 0.4685245517976875940, -0.8834504764630422002 ) ) ;
#15011 = ADVANCED_FACE ( 'NONE', ( #2926 ), #15480, .F. ) ;
#15012 = CARTESIAN_POINT ( 'NONE',  ( 0.3105533536971931685, -1.758467965264669752, 0.5220181958261356225 ) ) ;
#15013 = CARTESIAN_POINT ( 'NONE',  ( 0.3884081897485042734, -1.743572994024308764, -0.5875882558984819592 ) ) ;
#15014 = EDGE_CURVE ( 'NONE', #17181, #37380, #17165, .T. ) ;
#15015 = ORIENTED_EDGE ( 'NONE', *, *, #31218, .F. ) ;
#15016 = ORIENTED_EDGE ( 'NONE', *, *, #12180, .F. ) ;
#15017 =( BOUNDED_SURFACE ( )  B_SPLINE_SURFACE ( 3, 2, ( 
 ( #33442, #13900, #14731 ),
 ( #5250, #30163, #1990 ),
 ( #27298, #17803, #4445 ),
 ( #14513, #1806, #39413 ),
 ( #17007, #29550, #26473 ),
 ( #35933, #10844, #23606 ) ),
 .UNSPECIFIED., .F., .F., .F. ) 
 B_SPLINE_SURFACE_WITH_KNOTS ( ( 4, 2, 4 ),
 ( 3, 3 ),
 ( 0.000000000000000000, 0.0006500322046037510827, 0.001300064409207502165 ),
 ( 0.000000000000000000, 1.000000000000000000 ),
 .UNSPECIFIED. ) 
 GEOMETRIC_REPRESENTATION_ITEM ( )  RATIONAL_B_SPLINE_SURFACE ( (
 ( 1.000000000000000000, 0.7071067811865482389, 1.000000000000000000),
 ( 1.000000000000000000, 0.7294884244153418962, 1.000000000000000000),
 ( 1.000000000000000000, 0.7497986155812718101, 1.000000000000000000),
 ( 1.000000000000000000, 0.7883845046990943795, 1.000000000000000000),
 ( 1.000000000000000000, 0.8056655519482062155, 1.000000000000000000),
 ( 1.000000000000000000, 0.8219793159978240338, 1.000000000000000000) ) ) 
 REPRESENTATION_ITEM ( '' )  SURFACE ( )  );
#15018 = CARTESIAN_POINT ( 'NONE',  ( 0.1614573949321077284, -0.7569534866611321577, 0.1932149833450299559 ) ) ;
#15019 = VERTEX_POINT ( 'NONE', #34600 ) ;
#15020 = EDGE_CURVE ( 'NONE', #2801, #10878, #19171, .T. ) ;
#15021 = DIRECTION ( 'NONE',  ( -1.000000000000000000, -0.000000000000000000, -0.000000000000000000 ) ) ;
#15022 = DIRECTION ( 'NONE',  ( 1.000000000000000000, 0.000000000000000000, 0.000000000000000000 ) ) ;
#15024 = VERTEX_POINT ( 'NONE', #37893 ) ;
#15023 = CARTESIAN_POINT ( 'NONE',  ( 0.002170355132208537634, -0.5205946845004905121, 0.1266085954518501588 ) ) ;
#15025 = ORIENTED_EDGE ( 'NONE', *, *, #39400, .T. ) ;
#15026 = DIRECTION ( 'NONE',  ( -7.771561172376107616E-16, 7.170354002788761615E-17, -1.000000000000000000 ) ) ;
#15027 = ORIENTED_EDGE ( 'NONE', *, *, #33305, .T. ) ;
#15028 = EDGE_CURVE ( 'NONE', #13059, #36473, #22585, .T. ) ;
#15029 = CARTESIAN_POINT ( 'NONE',  ( 0.2671426166548651615, -1.675561005867882258, 0.5833829581153555655 ) ) ;
#15031 = CARTESIAN_POINT ( 'NONE',  ( 0.5051063752723966571, -1.605425671313008174, -0.4055270845263394541 ) ) ;
#15030 = CARTESIAN_POINT ( 'NONE',  ( 0.4055497041687889936, -1.192612325472327983, 0.6891132521580926040 ) ) ;
#15032 = CARTESIAN_POINT ( 'NONE',  ( 0.2923286432308245808, -1.660243258845594649, -0.3694143330441917450 ) ) ;
#15033 = EDGE_CURVE ( 'NONE', #37863, #37734, #12794, .T. ) ;
#15034 = PERSON_AND_ORGANIZATION_ROLE ( 'classification_officer' ) ;
#15035 = CARTESIAN_POINT ( 'NONE',  ( 0.1909291033137781868, -1.257065507333533727, -0.7137147910549515029 ) ) ;
#15037 = EDGE_LOOP ( 'NONE', ( #3840, #37333, #8226, #37513 ) ) ;
#15036 = ORIENTED_EDGE ( 'NONE', *, *, #18557, .T. ) ;
#15038 = EDGE_CURVE ( 'NONE', #12111, #17741, #21123, .T. ) ;
#15039 = DIRECTION ( 'NONE',  ( 0.000000000000000000, 0.000000000000000000, 1.000000000000000000 ) ) ;
#15040 = DIRECTION ( 'NONE',  ( 0.4999551463232373427, -0.8660512985181134660, 0.000000000000000000 ) ) ;
#15041 = DIRECTION ( 'NONE',  ( -0.9378410757839558132, 0.3470650033817760383, -5.691349986800563656E-16 ) ) ;
#15042 = CARTESIAN_POINT ( 'NONE',  ( 0.4229144610190289089, -1.180059474700835498, 0.8097779815502904599 ) ) ;
#15043 = CARTESIAN_POINT ( 'NONE',  ( 0.1857669404175232297, -0.8054308633438567178, 0.07733745057108264154 ) ) ;
#15044 = CARTESIAN_POINT ( 'NONE',  ( 0.03113248654051816583, 0.2954784694557334168, 0.05188905557145093855 ) ) ;
#15045 = CARTESIAN_POINT ( 'NONE',  ( 0.1864168460039302422, -0.7346540591771211215, 0.08921340677137505615 ) ) ;
#15046 = CARTESIAN_POINT ( 'NONE',  ( 0.4104533603378005546, -1.744126031043197411, -0.4329192950746086899 ) ) ;
#15047 = CARTESIAN_POINT ( 'NONE',  ( 0.4168791804701151293, -1.706510454905088237, 0.4274202794507407366 ) ) ;
#15048 = DIRECTION ( 'NONE',  ( 1.000000000000000000, 6.779273404243070203E-32, 4.314083075427408311E-32 ) ) ;
#15049 = CARTESIAN_POINT ( 'NONE',  ( -0.3000000000000000999, -3.705001275441084818, -0.3950781284944321903 ) ) ;
#15050 = CARTESIAN_POINT ( 'NONE',  ( 0.2801809802548146933, -0.9759768125023459140, 0.7245117847987158077 ) ) ;
#15051 = CARTESIAN_POINT ( 'NONE',  ( 0.4142910187529088017, -1.110460457557075564, 0.6154625682581813528 ) ) ;
#15052 = CARTESIAN_POINT ( 'NONE',  ( 0.4356476796531106310, -1.231215465721436697, 0.5833139271779056445 ) ) ;
#15053 = DIRECTION ( 'NONE',  ( 0.9999999999999997780, -6.162975822039154730E-33, -1.232595164407830946E-32 ) ) ;
#15054 = B_SPLINE_CURVE_WITH_KNOTS ( 'NONE', 3,
 ( #20097, #32626, #32813, #29958, #4435, #39596, #36527, #4235, #29535, #7727, #26460, #1794, #29738, #20293 ),
 .UNSPECIFIED., .F., .F.,
 ( 4, 2, 2, 2, 2, 2, 4 ),
 ( 3.332294980281255979E-17, 0.0007771933352389642172, 0.001554386670477895258, 0.001942983338097360128, 0.002331580005716824781, 0.002720176673336289867, 0.003108773340955754520 ),
 .UNSPECIFIED. ) ;
#15055 = CARTESIAN_POINT ( 'NONE',  ( -0.3000000000000000999, -2.292669950144801572, -0.8383185228372386222 ) ) ;
#15056 = CARTESIAN_POINT ( 'NONE',  ( 0.01179864804857342665, -0.6562760587974182380, 0.4561945812754703011 ) ) ;
#15057 = CARTESIAN_POINT ( 'NONE',  ( 0.09497277601810472092, -1.273348885617128889, 0.7438579102249397446 ) ) ;
#15058 = COORDINATED_UNIVERSAL_TIME_OFFSET ( 0, 0, .AHEAD. ) ;
#15059 = CARTESIAN_POINT ( 'NONE',  ( 0.4897931935426230177, -1.095389100717072850, 0.8439147301884563079 ) ) ;
#15060 = ADVANCED_FACE ( 'NONE', ( #85 ), #25551, .T. ) ;
#15061 = CARTESIAN_POINT ( 'NONE',  ( 0.7009476147591743311, -1.525393810516090909, 0.5735417758099603525 ) ) ;
#15062 = EDGE_CURVE ( 'NONE', #20255, #9760, #30298, .T. ) ;
#15063 = CARTESIAN_POINT ( 'NONE',  ( 0.02953079040095728247, 0.000000000000000000, 0.000000000000000000 ) ) ;
#15064 = EDGE_LOOP ( 'NONE', ( #30669, #27576, #17655, #39916 ) ) ;
#15065 = CARTESIAN_POINT ( 'NONE',  ( -0.0004431470427073231017, -0.9367128829938298207, 0.1457185332388704069 ) ) ;
#15066 = CARTESIAN_POINT ( 'NONE',  ( 0.2599175140567103193, -1.619495788301735351, 0.8180271650695088992 ) ) ;
#15067 = CARTESIAN_POINT ( 'NONE',  ( 0.1289590727735309694, -0.5712154984990630568, 0.2405744295037446634 ) ) ;
#15069 = ORIENTED_EDGE ( 'NONE', *, *, #28018, .T. ) ;
#15068 = CARTESIAN_POINT ( 'NONE',  ( 0.3839222738949826241, -1.728173381748683957, 0.4282780629211213053 ) ) ;
#15070 = CARTESIAN_POINT ( 'NONE',  ( 0.3520862261316686226, -0.8866190960188533587, 0.7137788081797863393 ) ) ;
#15072 = EDGE_LOOP ( 'NONE', ( #22841, #1983, #28431, #32910 ) ) ;
#15071 = ORIENTED_EDGE ( 'NONE', *, *, #2043, .T. ) ;
#15073 = CARTESIAN_POINT ( 'NONE',  ( 0.2132597674873976390, -0.6354326468627278235, 0.4153990741051870605 ) ) ;
#15074 = CARTESIAN_POINT ( 'NONE',  ( 0.3586646726171237032, -1.755266051717878195, -0.5357449245709422492 ) ) ;
#15075 = DIRECTION ( 'NONE',  ( 0.4999551463232373427, -0.8660512985181134660, 0.000000000000000000 ) ) ;
#15076 = DATE_AND_TIME ( #2538, #29314 ) ;
#15077 = CARTESIAN_POINT ( 'NONE',  ( 0.4841487358689927634, -1.673745430023940717, 0.5182417262823179049 ) ) ;
#15078 = ORIENTED_EDGE ( 'NONE', *, *, #13427, .T. ) ;
#15079 = CARTESIAN_POINT ( 'NONE',  ( 0.1070314971879695043, -0.7548214689483502271, 0.3798963362569547364 ) ) ;
#15080 = CARTESIAN_POINT ( 'NONE',  ( 0.3134922297020871773, -1.766968131109182050, 0.6133363199024374213 ) ) ;
#15081 = CARTESIAN_POINT ( 'NONE',  ( 0.4974254930090974969, -1.542500022935912485, 0.5729870860315193770 ) ) ;
#15082 = CARTESIAN_POINT ( 'NONE',  ( 0.07666882145575558416, -1.311286108063837164, 0.5563055692900464866 ) ) ;
#15083 = CARTESIAN_POINT ( 'NONE',  ( 0.1712463865401376573, -1.267487284506117584, 0.5765326934465192510 ) ) ;
#15084 = ORIENTED_EDGE ( 'NONE', *, *, #8277, .T. ) ;
#15085 = ORIENTED_EDGE ( 'NONE', *, *, #10405, .F. ) ;
#15086 = LINE ( 'NONE', #107, #12133 ) ;
#15087 = CARTESIAN_POINT ( 'NONE',  ( 0.4904781775425864909, -1.197665561882578888, 0.9014511766705987084 ) ) ;
#15088 = CARTESIAN_POINT ( 'NONE',  ( 0.4038347882558627200, -1.728811102478955419, -0.5994564538103192008 ) ) ;
#15089 = FACE_OUTER_BOUND ( 'NONE', #18157, .T. ) ;
#15090 = CARTESIAN_POINT ( 'NONE',  ( -0.1304423469995336093, -0.5262799683630393632, 0.3749999999999998335 ) ) ;
#15091 = CARTESIAN_POINT ( 'NONE',  ( 0.005216039386364625628, -1.801454245091123063, -0.6400404412376492491 ) ) ;
#15092 = CARTESIAN_POINT ( 'NONE',  ( 0.3269603303531253835, -1.178766071222939527, 0.4747738120598547495 ) ) ;
#15093 = CARTESIAN_POINT ( 'NONE',  ( 0.5544140612800516621, -1.190962001057203956, 0.5445415982692776158 ) ) ;
#15094 = APPROVAL_DATE_TIME ( #5415, #22019 ) ;
#15095 = CARTESIAN_POINT ( 'NONE',  ( 0.3559771861491330958, -1.881699356250711164, -0.5088919887031481126 ) ) ;
#15096 = CARTESIAN_POINT ( 'NONE',  ( 0.1359911470193229943, -1.231045907863504763, -0.5155029497116575543 ) ) ;
#15097 = DIRECTION ( 'NONE',  ( 5.551115123125774690E-17, 0.000000000000000000, -1.000000000000000000 ) ) ;
#15098 = CARTESIAN_POINT ( 'NONE',  ( -0.04762200653274584888, -0.3170437565186433049, -0.3633076762442132845 ) ) ;
#15099 = VERTEX_POINT ( 'NONE', #9498 ) ;
#15100 = CARTESIAN_POINT ( 'NONE',  ( 0.4841277252458648928, -1.120042291950998248, 0.5405469610105025913 ) ) ;
#15101 = CARTESIAN_POINT ( 'NONE',  ( -0.05616044724337315719, -0.2616774468955898048, 0.3775835982344368791 ) ) ;
#15102 = VECTOR ( 'NONE', #24072, 39.37007874015748143 ) ;
#15103 = ORIENTED_EDGE ( 'NONE', *, *, #17031, .F. ) ;
#15104 = CARTESIAN_POINT ( 'NONE',  ( -0.04087116408467048739, -0.02106952151319366195, -0.4712677373718183738 ) ) ;
#15105 = CARTESIAN_POINT ( 'NONE',  ( 0.03743165412374005463, -0.9419925036766105819, 0.6214317009962998517 ) ) ;
#15107 = EDGE_LOOP ( 'NONE', ( #17682, #795, #12101, #15221, #33475 ) ) ;
#15106 = ORIENTED_EDGE ( 'NONE', *, *, #20623, .F. ) ;
#15108 = DIRECTION ( 'NONE',  ( 0.000000000000000000, -0.3090169943749375148, 0.9510565162951567508 ) ) ;
#15109 = AXIS2_PLACEMENT_3D ( 'NONE', #25499, #19330, #25300 ) ;
#15110 = CARTESIAN_POINT ( 'NONE',  ( 0.03170953572519026598, -0.05433194795445580455, 0.4888234031312632122 ) ) ;
#15111 = CARTESIAN_POINT ( 'NONE',  ( 0.05634206451479344818, -0.4396230623831607343, -0.1319606688783178661 ) ) ;
#15112 = CARTESIAN_POINT ( 'NONE',  ( 0.1916844733273856960, -1.960004612374577793, -0.3277737872114317996 ) ) ;
#15113 = CARTESIAN_POINT ( 'NONE',  ( -0.2746410161513779258, -2.595429044015121534, -0.5484989581857646623 ) ) ;
#15115 = CARTESIAN_POINT ( 'NONE',  ( 0.1909286924077255032, -1.257064795538239022, -0.2869361388274796476 ) ) ;
#15114 = LINE ( 'NONE', #18404, #34471 ) ;
#15116 = CARTESIAN_POINT ( 'NONE',  ( 0.03643058821097030359, -0.3645913838654561978, -0.3593578898915239517 ) ) ;
#15117 = ORIENTED_EDGE ( 'NONE', *, *, #16498, .F. ) ;
#15118 = VERTEX_POINT ( 'NONE', #31502 ) ;
#15119 = CARTESIAN_POINT ( 'NONE',  ( 0.08531374436275271367, -1.317707820694483445, 0.5634626972692623470 ) ) ;
#15120 = ORIENTED_EDGE ( 'NONE', *, *, #35638, .F. ) ;
#15121 =( BOUNDED_SURFACE ( )  B_SPLINE_SURFACE ( 3, 2, ( 
 ( #9553, #4178, #28264 ),
 ( #37938, #34835, #19220 ),
 ( #31759, #20038, #23132 ),
 ( #8288, #35658, #23545 ),
 ( #17138, #7861, #36474 ),
 ( #1532, #29689, #20432 ) ),
 .UNSPECIFIED., .F., .F., .F. ) 
 B_SPLINE_SURFACE_WITH_KNOTS ( ( 4, 2, 4 ),
 ( 3, 3 ),
 ( 0.000000000000000000, 0.0004914683366409194638, 0.0009829366732818389275 ),
 ( 0.000000000000000000, 1.000000000000000000 ),
 .UNSPECIFIED. ) 
 GEOMETRIC_REPRESENTATION_ITEM ( )  RATIONAL_B_SPLINE_SURFACE ( (
 ( 1.000000000000000000, 0.9411999499705835381, 1.000000000000000000),
 ( 1.000000000000000000, 0.9445899725874141728, 1.000000000000000000),
 ( 1.000000000000000000, 0.9471079876882634307, 1.000000000000000000),
 ( 1.000000000000000000, 0.9513946071237538993, 1.000000000000000000),
 ( 1.000000000000000000, 0.9531191815715883697, 1.000000000000000000),
 ( 1.000000000000000000, 0.9544113358811291414, 1.000000000000000000) ) ) 
 REPRESENTATION_ITEM ( '' )  SURFACE ( )  );
#15122 = CARTESIAN_POINT ( 'NONE',  ( 0.02953079040095687308, 0.09152108205202803826, 0.5223162075576412988 ) ) ;
#15123 = CARTESIAN_POINT ( 'NONE',  ( 0.06506191882387997449, -0.5885835149343405792, 0.3205912525364184584 ) ) ;
#15125 = CARTESIAN_POINT ( 'NONE',  ( 0.5643309268556270242, -1.618135655174819609, 0.5416644041066450699 ) ) ;
#15124 = CARTESIAN_POINT ( 'NONE',  ( -0.03309057659885162456, -0.4608882367397833524, 0.2425133248664026742 ) ) ;
#15126 = DIRECTION ( 'NONE',  ( -1.000000000000000000, -2.341930812374887555E-31, 1.664003471950578127E-31 ) ) ;
#15127 = CARTESIAN_POINT ( 'NONE',  ( 0.3700000000046924642, -2.091145340040783562, -0.6943969493414033911 ) ) ;
#15128 = ORIENTED_EDGE ( 'NONE', *, *, #8220, .T. ) ;
#15129 = CARTESIAN_POINT ( 'NONE',  ( -0.02953079040095693900, -0.3810518745593889922, -0.3687679460475752902 ) ) ;
#15130 = CARTESIAN_POINT ( 'NONE',  ( -2.070754768975505034, -0.09959325338431362917, 0.09999999999999933942 ) ) ;
#15131 = CARTESIAN_POINT ( 'NONE',  ( 0.5738848579949621387, -1.499255142838190169, 0.5726899272605390223 ) ) ;
#15132 = CARTESIAN_POINT ( 'NONE',  ( 0.4671578922472904849, -1.051416226764902762, -0.5155029497116575543 ) ) ;
#15133 = DIRECTION ( 'NONE',  ( 0.7951751656451613304, 0.5387332766908925485, -0.2783215991027008784 ) ) ;
#15134 = ORIENTED_EDGE ( 'NONE', *, *, #39124, .F. ) ;
#15135 = DIRECTION ( 'NONE',  ( 0.000000000000000000, 0.8585432690668223232, -0.5127411190260187102 ) ) ;
#15136 = CARTESIAN_POINT ( 'NONE',  ( 0.2207932373118511316, -1.227997198505421217, 0.5267332555179391473 ) ) ;
#15137 = AXIS2_PLACEMENT_3D ( 'NONE', #30051, #26956, #39489 ) ;
#15138 = DIRECTION ( 'NONE',  ( 0.8660512985181133550, 0.4999551463232372317, 0.000000000000000000 ) ) ;
#15139 = CARTESIAN_POINT ( 'NONE',  ( 0.2322584854342325811, -1.232969341141011865, 0.4942330146944146629 ) ) ;
#15140 = CARTESIAN_POINT ( 'NONE',  ( 0.6761021464639213052, -1.407442781842621171, 0.4761751337611269674 ) ) ;
#15141 = VECTOR ( 'NONE', #36809, 39.37007874015748854 ) ;
#15142 = CARTESIAN_POINT ( 'NONE',  ( -0.02238765564325659319, 0.2417679119117849829, 0.4518160092940282091 ) ) ;
#15143 = CARTESIAN_POINT ( 'NONE',  ( 0.02191839362513907027, -1.011983551195656972, 0.5361064874689737136 ) ) ;
#15144 = VECTOR ( 'NONE', #1503, 39.37007874015748854 ) ;
#15145 = CARTESIAN_POINT ( 'NONE',  ( 0.6626570520036878520, -1.467463602353352936, -0.4130250948898684937 ) ) ;
#15146 = CARTESIAN_POINT ( 'NONE',  ( 0.06555721432897218537, -1.525479238971202633, -0.6748405168658114794 ) ) ;
#15147 = CARTESIAN_POINT ( 'NONE',  ( 0.5801239525038842659, -1.611124500691150541, 0.5902727294267513525 ) ) ;
#15148 = DIRECTION ( 'NONE',  ( 0.4999551463232373427, -0.8660512985181134660, 0.000000000000000000 ) ) ;
#15149 = CARTESIAN_POINT ( 'NONE',  ( 0.3699999999999786793, -2.120723258816476609, -0.4622723469118392714 ) ) ;
#15150 = B_SPLINE_CURVE_WITH_KNOTS ( 'NONE', 3,
 ( #36427, #8239, #32525, #26174 ),
 .UNSPECIFIED., .F., .F.,
 ( 4, 4 ),
 ( 0.01480563966802933389, 0.01646152871071565604 ),
 .UNSPECIFIED. ) ;
#15151 = EDGE_CURVE ( 'NONE', #12338, #40387, #34870, .T. ) ;
#15152 = VERTEX_POINT ( 'NONE', #10110 ) ;
#15153 = APPLIED_PERSON_AND_ORGANIZATION_ASSIGNMENT ( #33389, #40159, ( #24074 ) ) ;
#15154 = CARTESIAN_POINT ( 'NONE',  ( 0.3659513052091539209, -1.747039640913286451, -0.4990343722649543956 ) ) ;
#15155 = CARTESIAN_POINT ( 'NONE',  ( 0.6158309935355448239, -1.474965975646107763, -0.6185374182054230729 ) ) ;
#15156 = CARTESIAN_POINT ( 'NONE',  ( 0.1543608876718505218, -1.277530715710694098, 0.5557375578266802174 ) ) ;
#15157 = CARTESIAN_POINT ( 'NONE',  ( 0.3351195522891313172, -1.762354232558481337, 0.5631496603913015431 ) ) ;
#15158 = ORIENTED_EDGE ( 'NONE', *, *, #1219, .F. ) ;
#15159 = CARTESIAN_POINT ( 'NONE',  ( -2.070754768975509030, -0.09959325338431662678, 0.3382895567580819218 ) ) ;
#15160 = CARTESIAN_POINT ( 'NONE',  ( 0.3270026267580349311, -1.166750842916578712, 0.5707716670974642970 ) ) ;
#15161 = FACE_OUTER_BOUND ( 'NONE', #16162, .T. ) ;
#15162 = CARTESIAN_POINT ( 'NONE',  ( 0.02953079040094806068, 0.3810518745594044798, -0.3687679460475901116 ) ) ;
#15163 = CARTESIAN_POINT ( 'NONE',  ( 0.5135225295332491724, -1.315059133140256353, 0.6560163138962351592 ) ) ;
#15164 = CIRCLE ( 'NONE', #3324, 0.05000000000000000971 ) ;
#15166 = CARTESIAN_POINT ( 'NONE',  ( 0.4829308845308043496, -1.609609321180353714, -0.6424438852754091878 ) ) ;
#15165 = CARTESIAN_POINT ( 'NONE',  ( 0.1864644430607921566, -0.7573173996488720139, 0.1022963476796171639 ) ) ;
#15167 = CARTESIAN_POINT ( 'NONE',  ( 0.2669631944262408907, -0.9256872934665847374, 0.5220607882127416000 ) ) ;
#15168 = VERTEX_POINT ( 'NONE', #20341 ) ;
#15169 = APPROVAL_ROLE ( '' ) ;
#15170 = LINE ( 'NONE', #33914, #27008 ) ;
#15171 = ORIENTED_EDGE ( 'NONE', *, *, #23355, .T. ) ;
#15172 = CARTESIAN_POINT ( 'NONE',  ( 0.01016927536616487118, -0.5376657146052628011, 0.09484175047482117094 ) ) ;
#15173 = ORIENTED_EDGE ( 'NONE', *, *, #27502, .T. ) ;
#15174 = AXIS2_PLACEMENT_3D ( 'NONE', #13946, #7776, #20344 ) ;
#15175 = CARTESIAN_POINT ( 'NONE',  ( 0.06622580637515929070, -0.7619978381091805364, 0.6157077979737474172 ) ) ;
#15176 = CARTESIAN_POINT ( 'NONE',  ( 0.1855093845756445592, -0.7772764304750825470, 0.005262776399236719464 ) ) ;
#15177 = CARTESIAN_POINT ( 'NONE',  ( -0.1743922129835729085, -0.5166151207188712791, 0.3750000000000001110 ) ) ;
#15178 = VECTOR ( 'NONE', #34284, 39.37007874015748854 ) ;
#15179 = VECTOR ( 'NONE', #21467, 39.37007874015748143 ) ;
#15180 = ORIENTED_EDGE ( 'NONE', *, *, #11510, .F. ) ;
#15181 = ORIENTED_EDGE ( 'NONE', *, *, #32769, .F. ) ;
#15182 = CARTESIAN_POINT ( 'NONE',  ( 0.2697801010412542722, -1.019695529454659688, 0.6051538852367689403 ) ) ;
#15183 = CARTESIAN_POINT ( 'NONE',  ( 0.4007831926871883721, -1.251710563967610712, 0.8405983782434964802 ) ) ;
#15184 = ORIENTED_EDGE ( 'NONE', *, *, #7367, .T. ) ;
#15185 = CARTESIAN_POINT ( 'NONE',  ( 0.4356662251172991329, -1.610775558009423847, -0.3686272921855576756 ) ) ;
#15186 = EDGE_CURVE ( 'NONE', #17370, #9161, #15875, .T. ) ;
#15187 = DIRECTION ( 'NONE',  ( 0.4999551463232372317, -0.8660512985181135770, 0.000000000000000000 ) ) ;
#15188 = CARTESIAN_POINT ( 'NONE',  ( 0.5699416983924746605, -1.576656387088807509, -0.4662384028606618158 ) ) ;
#15189 = ADVANCED_FACE ( 'NONE', ( #19385, #6590 ), #26511, .F. ) ;
#15190 = CARTESIAN_POINT ( 'NONE',  ( -0.1045574869087419617, -0.4741643323009803734, 0.09813923389047396473 ) ) ;
#15191 = EDGE_CURVE ( 'NONE', #6763, #3822, #36325, .T. ) ;
#15192 = ADVANCED_FACE ( 'NONE', ( #36358 ), #25053, .F. ) ;
#15193 = DIRECTION ( 'NONE',  ( -0.4999551463232372317, 0.8660512985181134660, 6.869252350113302335E-17 ) ) ;
#15194 = CARTESIAN_POINT ( 'NONE',  ( 0.5705082898449433948, -1.615108203520839947, 0.3157417262808777658 ) ) ;
#15195 = CARTESIAN_POINT ( 'NONE',  ( 0.04293317454820642920, 0.3457449726441622073, -0.3536934093827128756 ) ) ;
#15196 = DIRECTION ( 'NONE',  ( -0.4413459890218813797, -0.8973370147131440877, 0.000000000000000000 ) ) ;
#15197 = CARTESIAN_POINT ( 'NONE',  ( 0.08075236803977006717, -1.368778601871594836, 0.5682417262808778791 ) ) ;
#15198 = CALENDAR_DATE ( 2026, 13, 10 ) ;
#15199 = CARTESIAN_POINT ( 'NONE',  ( 0.4807229719322908545, -1.126383887635181047, 0.4906570977974250569 ) ) ;
#15200 = AXIS2_PLACEMENT_3D ( 'NONE', #34311, #18687, #18285 ) ;
#15201 = CARTESIAN_POINT ( 'NONE',  ( 0.5246395073518916874, -1.203093073328722840, 0.6057417262809805525 ) ) ;
#15202 = CARTESIAN_POINT ( 'NONE',  ( 0.1999999999999789169, -2.097675824466503247, -0.2588528740066096678 ) ) ;
#15203 = CIRCLE ( 'NONE', #7278, 0.1946589359789743512 ) ;
#15204 = EDGE_CURVE ( 'NONE', #2287, #4624, #20754, .T. ) ;
#15205 = VECTOR ( 'NONE', #1047, 39.37007874015748143 ) ;
#15206 = CARTESIAN_POINT ( 'NONE',  ( 0.07670545266435074838, -1.210239791498856521, 0.7644951083879507614 ) ) ;
#15207 = DIRECTION ( 'NONE',  ( 0.000000000000000000, -0.7071067811865475727, 0.7071067811865475727 ) ) ;
#15208 = CIRCLE ( 'NONE', #5350, 2.001674066779353556 ) ;
#15209 = CARTESIAN_POINT ( 'NONE',  ( 0.4038347882558627200, -1.728811102478955419, -0.5994564538103192008 ) ) ;
#15210 = CARTESIAN_POINT ( 'NONE',  ( 0.2026546822922886959, -1.284935582237593854, -0.2885605078203434259 ) ) ;
#15211 = ORIENTED_EDGE ( 'NONE', *, *, #10636, .T. ) ;
#15212 = VERTEX_POINT ( 'NONE', #5084 ) ;
#15213 = CARTESIAN_POINT ( 'NONE',  ( -0.1089540792635268068, -0.4972110540766704889, 0.1150843967103426929 ) ) ;
#15214 = ORIENTED_EDGE ( 'NONE', *, *, #5982, .T. ) ;
#15215 = DIRECTION ( 'NONE',  ( 0.4999551463232372317, -0.8660512985181134660, 0.000000000000000000 ) ) ;
#15216 = CARTESIAN_POINT ( 'NONE',  ( -0.1150001097501708036, -0.4761628310996438018, 0.1178658437130112729 ) ) ;
#15218 = ORIENTED_EDGE ( 'NONE', *, *, #7672, .T. ) ;
#15217 = CARTESIAN_POINT ( 'NONE',  ( 0.002081379308398287331, -0.5326384292413223198, 0.1067899420028262103 ) ) ;
#15219 = VECTOR ( 'NONE', #1500, 39.37007874015748143 ) ;
#15220 = EDGE_CURVE ( 'NONE', #39658, #38602, #11244, .T. ) ;
#15221 = ORIENTED_EDGE ( 'NONE', *, *, #40072, .F. ) ;
#15222 = DIRECTION ( 'NONE',  ( 0.000000000000000000, 0.000000000000000000, 1.000000000000000000 ) ) ;
#15223 = ORIENTED_EDGE ( 'NONE', *, *, #22119, .T. ) ;
#15224 = CARTESIAN_POINT ( 'NONE',  ( 0.2664752076017231075, -1.675363658809308820, 0.5749620007053757309 ) ) ;
#15226 = CARTESIAN_POINT ( 'NONE',  ( 0.09592468290264696829, -1.296997100857483209, 0.6045289538570212118 ) ) ;
#15225 = CARTESIAN_POINT ( 'NONE',  ( 0.4878806933278804214, -1.547354733665422311, -0.5155029497116575543 ) ) ;
#15227 = CARTESIAN_POINT ( 'NONE',  ( 0.3882495962481228857, -1.143537762327198948, 0.4808272649735114701 ) ) ;
#15228 = CONTEXT_DEPENDENT_SHAPE_REPRESENTATION ( #13736, #20316 ) ;
#15229 = CIRCLE ( 'NONE', #7302, 0.06250000000000000000 ) ;
#15230 = DIRECTION ( 'NONE',  ( 0.4999999999999963918, 0.3085698060533155762, 0.8091876635195464074 ) ) ;
#15232 = ORIENTED_EDGE ( 'NONE', *, *, #10452, .F. ) ;
#15231 = ORIENTED_EDGE ( 'NONE', *, *, #27044, .F. ) ;
#15233 = CARTESIAN_POINT ( 'NONE',  ( 0.3691166938341062242, -1.174453341100101689, 0.5182417262812423209 ) ) ;
#15234 = CARTESIAN_POINT ( 'NONE',  ( -0.08000000000000000167, -2.230494317742474308, -0.6487310457122437146 ) ) ;
#15235 = CARTESIAN_POINT ( 'NONE',  ( -0.04140212552917654776, -0.4420250499596332094, 0.1614397576335104834 ) ) ;
#15236 = ADVANCED_FACE ( 'NONE', ( #2431 ), #8380, .T. ) ;
#15237 = CARTESIAN_POINT ( 'NONE',  ( 0.4406491928701437022, -1.207141337522043667, 0.7963399545800788903 ) ) ;
#15238 = VECTOR ( 'NONE', #14837, 39.37007874015748854 ) ;
#15239 = CIRCLE ( 'NONE', #6028, 0.03999999999999933470 ) ;
#15240 = CARTESIAN_POINT ( 'NONE',  ( -0.3000000000000000999, -4.162452804151155483, -0.5855328176471856771 ) ) ;
#15241 = CARTESIAN_POINT ( 'NONE',  ( 0.2718953302849530518, -1.636696295107877841, 0.7785526595467455735 ) ) ;
#15242 = CIRCLE ( 'NONE', #7971, 0.08000000000000002942 ) ;
#15243 = EDGE_CURVE ( 'NONE', #199, #30962, #20947, .T. ) ;
#15244 = CARTESIAN_POINT ( 'NONE',  ( -0.1151536691905419157, -0.5265970617445885349, 0.3290111518013588143 ) ) ;
#15245 = CARTESIAN_POINT ( 'NONE',  ( 0.4226000438817401061, -1.709616762427843550, 0.4282184315516496809 ) ) ;
#15246 = ADVANCED_FACE ( 'NONE', ( #20540 ), #10091, .T. ) ;
#15247 = CARTESIAN_POINT ( 'NONE',  ( 0.4112031682589459836, -1.245393622654190846, 0.5280675622111803413 ) ) ;
#15248 = CARTESIAN_POINT ( 'NONE',  ( -0.01548846960707504251, -0.09061086148575973886, 0.5171215251571027460 ) ) ;
#15249 = CARTESIAN_POINT ( 'NONE',  ( 0.4256878781885970464, -1.117437563897770936, 0.5966076842664922442 ) ) ;
#15250 = DIRECTION ( 'NONE',  ( 0.000000000000000000, 5.978086547377980964E-31, 1.000000000000000000 ) ) ;
#15251 = FACE_OUTER_BOUND ( 'NONE', #28224, .T. ) ;
#15252 = CARTESIAN_POINT ( 'NONE',  ( 0.002391669266185704034, -0.4944279760261894308, 0.2539263035736906149 ) ) ;
#15253 = CARTESIAN_POINT ( 'NONE',  ( 0.08035207416351047849, -1.251254375864937707, 0.7454261770637490292 ) ) ;
#15254 = PERSON_AND_ORGANIZATION ( #28500, #32463 ) ;
#15255 = CARTESIAN_POINT ( 'NONE',  ( 0.3337757566908341467, -0.8338946305499669309, 0.7209303476996544724 ) ) ;
#15256 = EDGE_CURVE ( 'NONE', #20453, #29444, #36759, .T. ) ;
#15257 = TOROIDAL_SURFACE ( 'NONE', #2105, 0.9237847906030132172, 0.01499999999999999944 ) ;
#15258 = EDGE_CURVE ( 'NONE', #35163, #30248, #5976, .T. ) ;
#15259 = CARTESIAN_POINT ( 'NONE',  ( 0.6672263256166638401, -1.559577713309558744, 0.6159734170043972279 ) ) ;
#15260 = CARTESIAN_POINT ( 'NONE',  ( -0.02000000000000000042, -2.579110126769056599, -0.2778638008585438413 ) ) ;
#15261 = AXIS2_PLACEMENT_3D ( 'NONE', #10130, #19409, #3551 ) ;
#15262 = VECTOR ( 'NONE', #9737, 39.37007874015748143 ) ;
#15263 = CARTESIAN_POINT ( 'NONE',  ( 0.3929308436705500340, -1.654878899977479723, -0.4107462969406636688 ) ) ;
#15264 = EDGE_LOOP ( 'NONE', ( #38986, #2877, #36977, #251 ) ) ;
#15265 = DIRECTION ( 'NONE',  ( 1.000000000000000000, 2.403560570595279103E-31, -1.725633230170969455E-31 ) ) ;
#15266 = CARTESIAN_POINT ( 'NONE',  ( 0.1905612331079999666, -1.343658964144449408, 0.9374431420955621208 ) ) ;
#15267 = CIRCLE ( 'NONE', #32318, 0.03000000000000022787 ) ;
#15269 = VERTEX_POINT ( 'NONE', #33904 ) ;
#15268 = CARTESIAN_POINT ( 'NONE',  ( 0.1284636661404361391, -0.5523917827180000462, 0.1701582641825293007 ) ) ;
#15271 = VERTEX_POINT ( 'NONE', #14969 ) ;
#15270 = DIRECTION ( 'NONE',  ( -1.000000000000000000, -6.779273404243070203E-32, -4.314083075427407763E-32 ) ) ;
#15272 = ADVANCED_FACE ( 'NONE', ( #14154 ), #27661, .T. ) ;
#15273 = CARTESIAN_POINT ( 'NONE',  ( 0.2980752164830456907, -0.8471807121723260448, 0.6106271213134966125 ) ) ;
#15275 = VERTEX_POINT ( 'NONE', #39253 ) ;
#15274 = ORIENTED_EDGE ( 'NONE', *, *, #32447, .T. ) ;
#15276 = CARTESIAN_POINT ( 'NONE',  ( 0.6830109224318547945, -1.405801553408178917, 0.7155230334201035935 ) ) ;
#15277 = DIRECTION ( 'NONE',  ( 1.000000000000000000, -0.000000000000000000, -0.000000000000000000 ) ) ;
#15278 = CARTESIAN_POINT ( 'NONE',  ( -0.2399999999999999079, -3.941790907013290823, -0.009415996779116623042 ) ) ;
#15279 = SECURITY_CLASSIFICATION_LEVEL ( 'unclassified' ) ;
#15280 = CARTESIAN_POINT ( 'NONE',  ( -0.03674260963082490866, 0.4430101671189254908, -0.1867880763203697836 ) ) ;
#15281 = EDGE_LOOP ( 'NONE', ( #20747, #34104, #209, #26567 ) ) ;
#15282 = CARTESIAN_POINT ( 'NONE',  ( 0.08866166269403266686, -0.7282185591720891082, 0.2282637218580873539 ) ) ;
#15283 = CARTESIAN_POINT ( 'NONE',  ( 0.1909286924077255032, -1.257064795538239022, -0.2869361388274796476 ) ) ;
#15284 = CARTESIAN_POINT ( 'NONE',  ( 0.1059692563321519704, -0.5739410805619210576, 0.2614456175893158929 ) ) ;
#15286 = CARTESIAN_POINT ( 'NONE',  ( 0.0003868712903910354398, -0.6441692727094081583, -0.01675880997169623687 ) ) ;
#15285 = CARTESIAN_POINT ( 'NONE',  ( 0.3219725102672574280, -1.761030903391374913, 0.4946895397007664008 ) ) ;
#15287 = CARTESIAN_POINT ( 'NONE',  ( 0.05376019824564439581, -1.293160722896381953, 0.6314177507418043955 ) ) ;
#15288 = B_SPLINE_CURVE_WITH_KNOTS ( 'NONE', 3,
 ( #29481, #16530, #31964, #13451, #38729, #35040 ),
 .UNSPECIFIED., .F., .F.,
 ( 4, 2, 4 ),
 ( 0.005298961318757118392, 0.006215189799740191909, 0.007131418280723266293 ),
 .UNSPECIFIED. ) ;
#15289 = B_SPLINE_CURVE_WITH_KNOTS ( 'NONE', 3,
 ( #22254, #15045, #34365, #24919 ),
 .UNSPECIFIED., .F., .F.,
 ( 4, 4 ),
 ( 3.832980274770707779E-05, 0.002032193406424597382 ),
 .UNSPECIFIED. ) ;
#15290 = ORIENTED_EDGE ( 'NONE', *, *, #15742, .F. ) ;
#15291 = AXIS2_PLACEMENT_3D ( 'NONE', #25008, #5461, #8762 ) ;
#15292 = EDGE_CURVE ( 'NONE', #23093, #11923, #34225, .T. ) ;
#15293 = CARTESIAN_POINT ( 'NONE',  ( 0.4518247747909678869, -1.695278170436179233, 0.5936431579880691034 ) ) ;
#15294 = CARTESIAN_POINT ( 'NONE',  ( 0.3798098266300030112, -0.9371975009833265480, 0.7311052114496043863 ) ) ;
#15295 = CARTESIAN_POINT ( 'NONE',  ( -0.01548846960712763066, 0.2450655194479529619, 0.4674710490748108516 ) ) ;
#15296 = VECTOR ( 'NONE', #13871, 39.37007874015748854 ) ;
#15297 = CARTESIAN_POINT ( 'NONE',  ( 0.3690044633497405746, -2.059848083720738021, -0.4704986862936899605 ) ) ;
#15299 = EDGE_CURVE ( 'NONE', #19668, #17694, #16505, .T. ) ;
#15298 =( NAMED_UNIT ( * ) SI_UNIT ( $, .STERADIAN. ) SOLID_ANGLE_UNIT ( ) );
#15300 = TOROIDAL_SURFACE ( 'NONE', #27786, 0.05000000000000000971, 0.1700000000000000400 ) ;
#15301 = CARTESIAN_POINT ( 'NONE',  ( 0.3717218693272927865, -1.759037576843597073, -0.4317987013060715640 ) ) ;
#15302 = CARTESIAN_POINT ( 'NONE',  ( -0.2746410161513779258, -2.154189217240303655, -0.3012881438978376458 ) ) ;
#15303 = CARTESIAN_POINT ( 'NONE',  ( 0.3296273898434592398, -1.177227151265824556, 0.4697822230349337769 ) ) ;
#15304 = CARTESIAN_POINT ( 'NONE',  ( 0.5549519752308349485, -1.188726111083455939, 0.5935319974400015131 ) ) ;
#15305 = CALENDAR_DATE ( 2026, 13, 10 ) ;
#15306 = CARTESIAN_POINT ( 'NONE',  ( 0.5680013577321684215, -1.617641779642786215, 0.5731888350583983494 ) ) ;
#15307 = AXIS2_PLACEMENT_3D ( 'NONE', #39516, #33759, #36835 ) ;
#15308 = ADVANCED_FACE ( 'NONE', ( #5889 ), #31363, .T. ) ;
#15309 = CARTESIAN_POINT ( 'NONE',  ( 0.3649451899893845219, -1.762153390321482549, -0.4829678164902960757 ) ) ;
#15310 = EDGE_CURVE ( 'NONE', #9709, #51, #32904, .T. ) ;
#15311 = CARTESIAN_POINT ( 'NONE',  ( 0.5376480657271666130, -1.519209816999901985, 0.5607234942562306923 ) ) ;
#15312 = CARTESIAN_POINT ( 'NONE',  ( -0.1167294259372886750, -0.5331983348239499598, 0.3084771640796422632 ) ) ;
#15313 = ORIENTED_EDGE ( 'NONE', *, *, #24228, .T. ) ;
#15314 = DIRECTION ( 'NONE',  ( 0.4999551463232372317, -0.8660512985181134660, 0.000000000000000000 ) ) ;
#15315 = CARTESIAN_POINT ( 'NONE',  ( 0.000000000000000000, -0.4700000000000001954, 0.04000000000000000777 ) ) ;
#15316 = AXIS2_PLACEMENT_3D ( 'NONE', #26152, #13163, #25729 ) ;
#15317 = CARTESIAN_POINT ( 'NONE',  ( -2.112273405726188513E-14, -2.097675824466503691, -0.2907077406111384099 ) ) ;
#15318 = ORIENTED_EDGE ( 'NONE', *, *, #3181, .F. ) ;
#15319 = CARTESIAN_POINT ( 'NONE',  ( -0.03874953289574976228, 0.03331175461110465197, -0.4752512399555730016 ) ) ;
#15320 = CARTESIAN_POINT ( 'NONE',  ( 0.1576789310610952621, -1.193613890868073790, 0.7517759638675417522 ) ) ;
#15322 = ORIENTED_EDGE ( 'NONE', *, *, #38550, .T. ) ;
#15321 = ORIENTED_EDGE ( 'NONE', *, *, #16734, .T. ) ;
#15323 = DIRECTION ( 'NONE',  ( -0.9378410757839562573, 0.2807814858886506504, 0.2039996905746501998 ) ) ;
#15324 = VECTOR ( 'NONE', #31211, 39.37007874015748143 ) ;
#15325 = VECTOR ( 'NONE', #21496, 39.37007874015748143 ) ;
#15326 = DIRECTION ( 'NONE',  ( 1.000000000000000000, 2.280301054154495132E-31, -1.664003471950577689E-31 ) ) ;
#15327 = CARTESIAN_POINT ( 'NONE',  ( 0.05201840200954526566, -0.4527058363063625190, -0.1280872907206782041 ) ) ;
#15328 = CARTESIAN_POINT ( 'NONE',  ( 0.000000000000000000, 0.09520121321898405986, -0.1758883992810029440 ) ) ;
#15329 = CARTESIAN_POINT ( 'NONE',  ( 3.466477128667603047, -1.051097370103299733, 0.4182417262808778013 ) ) ;
#15331 = CARTESIAN_POINT ( 'NONE',  ( 0.1757500541653520820, -1.230771478115229245, -0.4400554600884079570 ) ) ;
#15330 = CARTESIAN_POINT ( 'NONE',  ( -0.1383891728403244537, 0.05441343863104586287, 0.01030292142312777375 ) ) ;
#15332 = CARTESIAN_POINT ( 'NONE',  ( 0.04285640132273934449, -0.3459922227646587412, -0.3537374076363848374 ) ) ;
#15333 = ORIENTED_EDGE ( 'NONE', *, *, #10518, .F. ) ;
#15334 = CARTESIAN_POINT ( 'NONE',  ( 0.1882806112850526625, -0.7844922771024498420, 0.6463987001619690975 ) ) ;
#15335 = EDGE_LOOP ( 'NONE', ( #6461, #21107, #31465, #30764, #23741 ) ) ;
#15336 = CIRCLE ( 'NONE', #14645, 0.5302738246768107233 ) ;
#15337 = CARTESIAN_POINT ( 'NONE',  ( -0.2136509456379322158, -0.4946207598421927254, 0.3599999999999998757 ) ) ;
#15338 = CARTESIAN_POINT ( 'NONE',  ( 0.07485732638563033503, -0.5697853684528622065, 0.2660001439021964509 ) ) ;
#15340 = CARTESIAN_POINT ( 'NONE',  ( 0.5953197980378827081, -1.599064723402610300, 0.4311035055375515013 ) ) ;
#15339 = DIRECTION ( 'NONE',  ( -0.9378410757839558132, -0.3470650033817761493, -5.691349986800565628E-16 ) ) ;
#15341 = CARTESIAN_POINT ( 'NONE',  ( 0.4980091573394558324, -1.195248457127482400, 0.4182417262808778013 ) ) ;
#15342 = CARTESIAN_POINT ( 'NONE',  ( 0.1810766014996237627, -1.262752222553218395, -0.2917159793182508842 ) ) ;
#15343 = EDGE_CURVE ( 'NONE', #6598, #17659, #12476, .T. ) ;
#15344 = CARTESIAN_POINT ( 'NONE',  ( 0.3999999999999786504, -2.143487347927110598, -0.5325376609221695867 ) ) ;
#15345 = CARTESIAN_POINT ( 'NONE',  ( 0.1983600803612964869, -2.021069303733847189, -0.2825292762747920183 ) ) ;
#15346 = CARTESIAN_POINT ( 'NONE',  ( 0.5410910530678962882, -1.436320634972935828, 0.7616694271696782259 ) ) ;
#15347 = CARTESIAN_POINT ( 'NONE',  ( 0.4693410224259870200, -1.672534098797133328, 0.5641912338472405697 ) ) ;
#15348 = CARTESIAN_POINT ( 'NONE',  ( -0.1669433606228592770, 0.5138636982738122860, 0.3032895567580813356 ) ) ;
#15349 = CARTESIAN_POINT ( 'NONE',  ( -0.03159140494780132702, 0.4482517543799769411, 0.2030416442520433795 ) ) ;
#15350 = CARTESIAN_POINT ( 'NONE',  ( 0.5360537876065293306, -1.620675796450378181, 0.4182417262808775793 ) ) ;
#15351 = FACE_OUTER_BOUND ( 'NONE', #6664, .T. ) ;
#15352 = CARTESIAN_POINT ( 'NONE',  ( 0.3509329672325016136, -1.164895094812919973, 0.4278180645112279468 ) ) ;
#15353 = CARTESIAN_POINT ( 'NONE',  ( 0.5753152089321617035, -1.233008725051026655, 0.8518361925389578149 ) ) ;
#15354 = AXIS2_PLACEMENT_3D ( 'NONE', #4765, #7239, #23538 ) ;
#15355 = CIRCLE ( 'NONE', #29158, 0.01499999999999994393 ) ;
#15356 = CARTESIAN_POINT ( 'NONE',  ( -0.03642997641689365435, 0.2291049489869432521, 0.4577964116453020482 ) ) ;
#15357 = CARTESIAN_POINT ( 'NONE',  ( -0.0004424791517057791407, -0.9367167128783578933, 0.1808097727947970967 ) ) ;
#15358 = CARTESIAN_POINT ( 'NONE',  ( 0.6412634316914778143, -1.498276373346698165, -0.4128329508740462561 ) ) ;
#15359 = CARTESIAN_POINT ( 'NONE',  ( 0.6465835049539127022, -1.539613817736325441, 0.4282417262808769221 ) ) ;
#15360 = CARTESIAN_POINT ( 'NONE',  ( 0.06676919707949596772, -0.8365002846677066506, 0.2371296666657259078 ) ) ;
#15361 = CARTESIAN_POINT ( 'NONE',  ( 0.04229956186878635477, 0.2825373843407185115, -0.3739591931584693718 ) ) ;
#15362 = AXIS2_PLACEMENT_3D ( 'NONE', #37225, #27763, #2273 ) ;
#15363 = DIRECTION ( 'NONE',  ( 0.000000000000000000, 0.000000000000000000, -1.000000000000000000 ) ) ;
#15364 = AXIS2_PLACEMENT_3D ( 'NONE', #2093, #40547, #18136 ) ;
#15365 = EDGE_LOOP ( 'NONE', ( #26304, #38350, #32360, #12475 ) ) ;
#15366 = DIRECTION ( 'NONE',  ( -0.8374990061932787722, -0.4718101308923743353, 0.2756639530526091564 ) ) ;
#15367 = CARTESIAN_POINT ( 'NONE',  ( 0.3121344959780879558, -1.175754444927441300, 0.5182417262812437642 ) ) ;
#15368 = CARTESIAN_POINT ( 'NONE',  ( 0.6636790156337686319, -1.488637877925755637, 0.4182417262808777458 ) ) ;
#15369 = EDGE_CURVE ( 'NONE', #2187, #23858, #21637, .T. ) ;
#15370 = CARTESIAN_POINT ( 'NONE',  ( 0.4675494560575759184, -1.684665788739993619, -0.6179439388203937789 ) ) ;
#15371 = ORIENTED_EDGE ( 'NONE', *, *, #34575, .F. ) ;
#15372 = CARTESIAN_POINT ( 'NONE',  ( 0.5304177574979601628, -1.660704847279741214, -0.5790554921387824905 ) ) ;
#15373 =( BOUNDED_SURFACE ( )  B_SPLINE_SURFACE ( 3, 2, ( 
 ( #27485, #15119, #40428 ),
 ( #30358, #8347, #15546 ),
 ( #36535, #6054, #2186 ),
 ( #2582, #24204, #34049 ),
 ( #40010, #18622, #31180 ),
 ( #17798, #2998, #39605 ) ),
 .UNSPECIFIED., .F., .F., .T. ) 
 B_SPLINE_SURFACE_WITH_KNOTS ( ( 4, 2, 4 ),
 ( 3, 3 ),
 ( -1.028582925126330799E-05, 0.0008016497212322824285, 0.001613585271715828069 ),
 ( 0.000000000000000000, 1.000000000000000000 ),
 .UNSPECIFIED. ) 
 GEOMETRIC_REPRESENTATION_ITEM ( )  RATIONAL_B_SPLINE_SURFACE ( (
 ( 1.000000000000000000, 0.7092489947169868802, 1.000000000000000000),
 ( 1.000000000000000000, 0.7095858694734782368, 1.000000000000000000),
 ( 1.000000000000000000, 0.7098079294007280104, 1.000000000000000000),
 ( 1.000000000000000000, 0.7100340289643065628, 1.000000000000000000),
 ( 1.000000000000000000, 0.7100334978315825385, 1.000000000000000000),
 ( 1.000000000000000000, 0.7099595931732594067, 1.000000000000000000) ) ) 
 REPRESENTATION_ITEM ( '' )  SURFACE ( )  );
#15374 = DIRECTION ( 'NONE',  ( -0.4999551463232373427, 0.8660512985181134660, -0.000000000000000000 ) ) ;
#15375 = CARTESIAN_POINT ( 'NONE',  ( 0.3984114568195522010, -1.599003643269838904, -0.5155029497116575543 ) ) ;
#15376 = FACE_OUTER_BOUND ( 'NONE', #24556, .T. ) ;
#15377 = B_SPLINE_CURVE_WITH_KNOTS ( 'NONE', 3,
 ( #13089, #10001, #22573, #6698, #16195, #7097, #6905, #16377, #13290, #10215 ),
 .UNSPECIFIED., .F., .F.,
 ( 4, 2, 2, 2, 4 ),
 ( 4.336808689942017736E-19, 0.0006631238949667744636, 0.001326247789933548494, 0.001989371684900322415, 0.002652495579867096553 ),
 .UNSPECIFIED. ) ;
#15378 = AXIS2_PLACEMENT_3D ( 'NONE', #9800, #1192, #22373 ) ;
#15379 = CARTESIAN_POINT ( 'NONE',  ( 0.4227732138525802652, -1.178737739220398595, 0.7256702507413027581 ) ) ;
#15381 = EDGE_LOOP ( 'NONE', ( #33339, #36826 ) ) ;
#15380 = DIRECTION ( 'NONE',  ( 0.4999551463232372317, -0.8660512985181135770, 0.000000000000000000 ) ) ;
#15382 = CARTESIAN_POINT ( 'NONE',  ( 0.3170172301852910435, -0.9601440561661597206, 0.5902234374070133294 ) ) ;
#15383 = ORIENTED_EDGE ( 'NONE', *, *, #36623, .F. ) ;
#15384 = PERSON_AND_ORGANIZATION ( #28500, #32463 ) ;
#15385 = CARTESIAN_POINT ( 'NONE',  ( 0.1831853279715622285, -1.261726972505375910, -0.3225413305835142519 ) ) ;
#15386 = EDGE_LOOP ( 'NONE', ( #35166, #29394, #34305, #28428 ) ) ;
#15387 = ORIENTED_EDGE ( 'NONE', *, *, #30387, .T. ) ;
#15388 = AXIS2_PLACEMENT_3D ( 'NONE', #33909, #11687, #37377 ) ;
#15389 = CARTESIAN_POINT ( 'NONE',  ( 0.3286955653016211953, -1.530979031070108354, 0.8411537230885318683 ) ) ;
#15391 = CARTESIAN_POINT ( 'NONE',  ( 0.1123234024242402845, -0.8095807605550189301, -0.06225138739832922902 ) ) ;
#15390 = CARTESIAN_POINT ( 'NONE',  ( 0.1637585665034339832, -0.5994899851647166322, 0.1022936816274461203 ) ) ;
#15392 = FACE_OUTER_BOUND ( 'NONE', #1750, .T. ) ;
#15393 = ORIENTED_EDGE ( 'NONE', *, *, #9733, .T. ) ;
#15394 = CARTESIAN_POINT ( 'NONE',  ( 0.3859036440852527394, -1.104769981098987275, 0.6297154657313602799 ) ) ;
#15395 = CARTESIAN_POINT ( 'NONE',  ( 0.5367984847559414963, -1.480828653130701555, 0.7264103812508763136 ) ) ;
#15396 = ORIENTED_EDGE ( 'NONE', *, *, #13928, .T. ) ;
#15397 = CIRCLE ( 'NONE', #20664, 0.1000000000000000194 ) ;
#15398 = DIRECTION ( 'NONE',  ( -1.000000000000000000, -2.341930812374887555E-31, 1.664003471950578127E-31 ) ) ;
#15399 = FACE_OUTER_BOUND ( 'NONE', #17249, .T. ) ;
#15400 = AXIS2_PLACEMENT_3D ( 'NONE', #8210, #11710, #33308 ) ;
#15401 = CARTESIAN_POINT ( 'NONE',  ( 0.5623860021574346169, -1.585002265747556871, -0.5017772603597512315 ) ) ;
#15402 = CARTESIAN_POINT ( 'NONE',  ( -0.1210148435730249716, -0.5061394519557904648, 0.3122829191279362093 ) ) ;
#15403 = DIRECTION ( 'NONE',  ( 0.000000000000000000, 0.000000000000000000, -1.000000000000000000 ) ) ;
#15404 = CARTESIAN_POINT ( 'NONE',  ( 0.4814184380812144282, -1.664799897621735303, 0.3157417262808778213 ) ) ;
#15405 = CARTESIAN_POINT ( 'NONE',  ( 0.5908959048872449715, -1.601544548465861473, 0.4282886817583849703 ) ) ;
#15406 = DIRECTION ( 'NONE',  ( -0.4999551463232359549, 0.8660512985181140211, 0.000000000000000000 ) ) ;
#15407 = CARTESIAN_POINT ( 'NONE',  ( 0.07959189571600921997, -1.355556588927695927, 0.6171934786799392336 ) ) ;
#15408 = SECURITY_CLASSIFICATION_LEVEL ( 'unclassified' ) ;
#15409 = VECTOR ( 'NONE', #31513, 39.37007874015748854 ) ;
#15410 = CARTESIAN_POINT ( 'NONE',  ( 0.3026114960654325836, -0.9782852559307895213, 0.5634791713200563157 ) ) ;
#15411 = VECTOR ( 'NONE', #25944, 39.37007874015748143 ) ;
#15412 = CARTESIAN_POINT ( 'NONE',  ( 0.4873759665769543115, -1.128466840950351768, 0.5006193672520922178 ) ) ;
#15413 = CARTESIAN_POINT ( 'NONE',  ( 0.4509040138740343928, -1.222352207351879105, 0.6057417262810296243 ) ) ;
#15414 = DIRECTION ( 'NONE',  ( -1.000000000000000000, -0.000000000000000000, -0.000000000000000000 ) ) ;
#15415 = CIRCLE ( 'NONE', #6215, 0.1600000000000006972 ) ;
#15416 = AXIS2_PLACEMENT_3D ( 'NONE', #851, #38457, #28797 ) ;
#15417 = LOCAL_TIME ( 0, 53, 7.000000000000000000, #37408 ) ;
#15418 = CARTESIAN_POINT ( 'NONE',  ( 0.01373823669757498131, -0.9963338274435274977, 0.5786879937691099540 ) ) ;
#15419 = DIRECTION ( 'NONE',  ( 1.000000000000000000, 0.000000000000000000, 0.000000000000000000 ) ) ;
#15420 = DIRECTION ( 'NONE',  ( 0.000000000000000000, 0.000000000000000000, -1.000000000000000000 ) ) ;
#15421 = CARTESIAN_POINT ( 'NONE',  ( 0.3693979415174998282, -1.758566222085671704, -0.5866259412024878994 ) ) ;
#15422 = EDGE_CURVE ( 'NONE', #33790, #2621, #38165, .T. ) ;
#15423 = EDGE_CURVE ( 'NONE', #4341, #7054, #30933, .T. ) ;
#15424 = AXIS2_PLACEMENT_3D ( 'NONE', #1164, #3994, #26652 ) ;
#15425 = ORIENTED_EDGE ( 'NONE', *, *, #25229, .T. ) ;
#15426 = EDGE_CURVE ( 'NONE', #28841, #27374, #31592, .T. ) ;
#15427 = ORIENTED_EDGE ( 'NONE', *, *, #36315, .T. ) ;
#15428 = DIRECTION ( 'NONE',  ( 1.000000000000000000, 0.000000000000000000, 0.000000000000000000 ) ) ;
#15429 = ORIENTED_EDGE ( 'NONE', *, *, #38178, .F. ) ;
#15430 = CARTESIAN_POINT ( 'NONE',  ( 0.2709623010280027278, -1.672610760848568967, 0.4891849873696615392 ) ) ;
#15431 = CYLINDRICAL_SURFACE ( 'NONE', #22596, 0.5399999999999999245 ) ;
#15432 = EDGE_CURVE ( 'NONE', #23563, #28743, #12566, .T. ) ;
#15433 = CARTESIAN_POINT ( 'NONE',  ( 0.5704759322846583158, -1.412223342220865652, 0.6612748060004949302 ) ) ;
#15435 = ORIENTED_EDGE ( 'NONE', *, *, #31276, .F. ) ;
#15434 = CARTESIAN_POINT ( 'NONE',  ( 0.001117283261919534186, -0.5756253649193824318, 0.02022279314256347771 ) ) ;
#15436 = ADVANCED_FACE ( 'NONE', ( #13507 ), #39511, .T. ) ;
#15437 = ORIENTED_EDGE ( 'NONE', *, *, #24778, .T. ) ;
#15438 = DIRECTION ( 'NONE',  ( 0.000000000000000000, 0.5877852522924756906, 0.8090169943749455639 ) ) ;
#15439 = VERTEX_POINT ( 'NONE', #35708 ) ;
#15440 = CARTESIAN_POINT ( 'NONE',  ( 0.06122518135456767735, -0.8600918236809148576, 0.7294040382890789598 ) ) ;
#15442 = CARTESIAN_POINT ( 'NONE',  ( 0.3224586748600002384, -1.296590453040780799, 0.4182417262808783009 ) ) ;
#15441 = CARTESIAN_POINT ( 'NONE',  ( 0.3229932430035513113, -1.082493911471395620, 0.7408616947465277436 ) ) ;
#15443 = CARTESIAN_POINT ( 'NONE',  ( 0.3763421349350077327, -1.150419605846286331, 0.4856841184440788273 ) ) ;
#15444 = CIRCLE ( 'NONE', #25285, 0.01500000000000005669 ) ;
#15445 = CARTESIAN_POINT ( 'NONE',  ( 0.4203826191881492313, -1.700944664958275343, -0.4172566670736511107 ) ) ;
#15447 = ORIENTED_EDGE ( 'NONE', *, *, #20885, .T. ) ;
#15446 = ORIENTED_EDGE ( 'NONE', *, *, #10810, .T. ) ;
#15448 = AXIS2_PLACEMENT_3D ( 'NONE', #1718, #23107, #3950 ) ;
#15449 = CARTESIAN_POINT ( 'NONE',  ( 0.3853645080447097304, -1.799773605325351467, -0.4824436846277732061 ) ) ;
#15450 = CARTESIAN_POINT ( 'NONE',  ( 0.1109049718728797040, -0.9286333055842316275, 0.1397141703224096809 ) ) ;
#15451 = CARTESIAN_POINT ( 'NONE',  ( -0.05186792262757054101, -0.4530091620765513416, 0.1282979832840831225 ) ) ;
#15452 = AXIS2_PLACEMENT_3D ( 'NONE', #12234, #21299, #33840 ) ;
#15453 = CARTESIAN_POINT ( 'NONE',  ( 0.5435548342818103951, -1.369150181482250872, 0.7844560790062110600 ) ) ;
#15454 = EDGE_CURVE ( 'NONE', #5500, #26101, #123, .T. ) ;
#15455 = DIRECTION ( 'NONE',  ( 0.000000000000000000, 0.000000000000000000, -1.000000000000000000 ) ) ;
#15456 = APPROVAL_PERSON_ORGANIZATION ( #444, #906, #19318 ) ;
#15457 = CARTESIAN_POINT ( 'NONE',  ( 0.5030897102885044658, -1.688833090636736145, -0.4393626443944793625 ) ) ;
#15458 = APPLIED_PERSON_AND_ORGANIZATION_ASSIGNMENT ( #39791, #541, ( #27300 ) ) ;
#15459 = CARTESIAN_POINT ( 'NONE',  ( 0.2297839753664799867, -1.355407543777841228, 1.031615039705529480 ) ) ;
#15460 = CIRCLE ( 'NONE', #30549, 0.01500000000000000291 ) ;
#15461 = CARTESIAN_POINT ( 'NONE',  ( 0.4103531506980909738, -1.245885523118785532, 0.5231355499499931172 ) ) ;
#15462 = CARTESIAN_POINT ( 'NONE',  ( 0.6596209037232241279, -1.565455939274822184, 0.3157417262808776548 ) ) ;
#15463 = CARTESIAN_POINT ( 'NONE',  ( 0.3406212661944226228, -1.061315175790578547, 0.7613082687028679407 ) ) ;
#15464 = CARTESIAN_POINT ( 'NONE',  ( -0.3000000000000000999, -3.525450504378606187, -0.1357627943591874498 ) ) ;
#15465 = CARTESIAN_POINT ( 'NONE',  ( 0.5622475518571767861, -1.322773533229203435, -0.5166151207188712791 ) ) ;
#15466 = DIRECTION ( 'NONE',  ( -7.771561172376107616E-16, 7.170354002788761615E-17, -1.000000000000000000 ) ) ;
#15467 = EDGE_CURVE ( 'NONE', #27640, #36370, #32387, .T. ) ;
#15468 = CARTESIAN_POINT ( 'NONE',  ( 0.05999999999999990757, 0.1477392347278677909, 0.02594452778572553867 ) ) ;
#15469 = CARTESIAN_POINT ( 'NONE',  ( 0.05825259049622175112, -1.116031997329672620, 0.7479867058011834269 ) ) ;
#15470 = PERSON_AND_ORGANIZATION_ROLE ( 'design_owner' ) ;
#15471 = CARTESIAN_POINT ( 'NONE',  ( 0.5405998635167484911, -1.177347015163466182, 0.8538091603066587654 ) ) ;
#15472 = VECTOR ( 'NONE', #26148, 39.37007874015748143 ) ;
#15473 = CARTESIAN_POINT ( 'NONE',  ( -0.08000000000000000167, -2.183180860297908144, -0.4937760292030871079 ) ) ;
#15474 = VECTOR ( 'NONE', #24832, 39.37007874015748143 ) ;
#15475 = DIRECTION ( 'NONE',  ( 0.8660512985181133550, 0.4999551463232371207, 1.536967049004847180E-15 ) ) ;
#15476 = CARTESIAN_POINT ( 'NONE',  ( 0.05634307799789363413, -0.2614070397638400545, 0.3772863199289458458 ) ) ;
#15477 = EDGE_CURVE ( 'NONE', #29445, #8808, #13091, .T. ) ;
#15478 = CARTESIAN_POINT ( 'NONE',  ( 0.3787673471718397966, -1.665243962817426704, -0.4196842139337432775 ) ) ;
#15479 = VERTEX_POINT ( 'NONE', #2174 ) ;
#15480 = CYLINDRICAL_SURFACE ( 'NONE', #34877, 0.1000000000000000194 ) ;
#15481 = LOCAL_TIME ( 0, 53, 7.000000000000000000, #14639 ) ;
#15482 = CARTESIAN_POINT ( 'NONE',  ( 0.1961652843398811463, -1.362277586928017037, 0.9373159428213221345 ) ) ;
#15483 = EDGE_CURVE ( 'NONE', #34692, #32978, #39396, .T. ) ;
#15484 = CARTESIAN_POINT ( 'NONE',  ( 0.5887134414239101332, -1.491024950170938945, 0.5921876951808361378 ) ) ;
#15486 = ORIENTED_EDGE ( 'NONE', *, *, #12296, .F. ) ;
#15485 = FACE_OUTER_BOUND ( 'NONE', #17211, .T. ) ;
#15487 = EDGE_CURVE ( 'NONE', #26211, #15711, #31691, .T. ) ;
#15488 = AXIS2_PLACEMENT_3D ( 'NONE', #34586, #9693, #28206 ) ;
#15489 = CARTESIAN_POINT ( 'NONE',  ( 0.3057296174425681579, -0.8572510462883253801, 0.6221769111833096444 ) ) ;
#15491 = VERTEX_POINT ( 'NONE', #17996 ) ;
#15490 = ORIENTED_EDGE ( 'NONE', *, *, #29736, .F. ) ;
#15492 = CARTESIAN_POINT ( 'NONE',  ( 0.6989129671518158338, -1.435640316137777983, 0.6243391198283677612 ) ) ;
#15493 = FACE_OUTER_BOUND ( 'NONE', #31166, .T. ) ;
#15494 = DIRECTION ( 'NONE',  ( 0.000000000000000000, -0.3090169943749375148, 0.9510565162951567508 ) ) ;
#15495 = SECURITY_CLASSIFICATION_LEVEL ( 'unclassified' ) ;
#15496 = LINE ( 'NONE', #28231, #157 ) ;
#15497 = ORIENTED_EDGE ( 'NONE', *, *, #14224, .T. ) ;
#15498 = CARTESIAN_POINT ( 'NONE',  ( 0.1524884462945051700, -0.8417431550776262039, 0.5307603544456596101 ) ) ;
#15499 = FACE_OUTER_BOUND ( 'NONE', #29069, .T. ) ;
#15500 = CARTESIAN_POINT ( 'NONE',  ( 0.4053429200396714283, -1.311055352502511484, 0.8450935282451459418 ) ) ;
#15502 = CARTESIAN_POINT ( 'NONE',  ( -0.0007964796033632633252, -0.7717706572747778937, 0.0001241267463302354434 ) ) ;
#15501 = CARTESIAN_POINT ( 'NONE',  ( -0.1304423469995336093, -0.5262799683630393632, 0.08500000000000018652 ) ) ;
#15503 = EDGE_CURVE ( 'NONE', #15646, #15099, #14494, .T. ) ;
#15504 = CARTESIAN_POINT ( 'NONE',  ( -0.1665325656947821142, 0.5173663872579682410, 0.1272034666820740234 ) ) ;
#15505 = VERTEX_POINT ( 'NONE', #39592 ) ;
#15506 = CARTESIAN_POINT ( 'NONE',  ( 0.4751225739783559998, -1.681097010791106516, 0.5628964895538534075 ) ) ;
#15507 = CLOSED_SHELL ( 'NONE', ( #17310, #28649, #935, #24846, #33006, #6495, #20956, #2911, #25363, #40189, #1610, #3393, #36604, #39072, #14436, #37964, #31924, #18995, #13312, #11153, #10639, #21903, #17184, #17530, #29031, #2699, #25242, #39618, #26083, #27056, #10299, #16623, #26245, #31031, #31282, #9536, #33070, #882, #992, #459, #25344, #6914, #9886, #9665, #14735, #36930, #7138, #12921, #9146, #30801, #14267, #39746, #37930, #21236, #35961, #32821, #33615, #39853, #27003, #39905, #762, #22860, #31582, #5366, #38157, #2612, #3260, #11437, #20006, #11268, #6860, #16674, #10045, #27735, #34939, #30068, #39924, #31599, #33612, #24880, #26201, #14476, #39342, #28585, #10009, #438, #38355, #23375, #10020, #4423, #4700, #17790, #36384, #1869, #31362, #11586, #36561, #7851, #23302, #5369, #34797, #12932, #35421, #21541, #1387, #13230, #7762, #28674, #15246, #1133, #20739, #29885, #15955, #10401, #36447, #19699, #10006, #7076, #26477, #33821, #26113, #27277, #29374, #21629, #34627, #15308, #20910, #35034, #40121, #30648, #33317, #2214, #13977, #25218, #23592, #3703, #37559, #6383, #35511, #19952, #19600, #3629, #22235, #35376, #35360, #17477, #9188, #24265, #3857, #37193, #4127, #13586, #21294, #37411, #12696, #40438 ) ) ;
#15508 = CARTESIAN_POINT ( 'NONE',  ( 0.7179022346679152511, -1.464906623875073644, 0.7581280492328499321 ) ) ;
#15509 = AXIS2_PLACEMENT_3D ( 'NONE', #17328, #1315, #13822 ) ;
#15510 = CARTESIAN_POINT ( 'NONE',  ( 0.4833848602004494621, -1.629403264803032547, -0.6020753396110556377 ) ) ;
#15511 = CARTESIAN_POINT ( 'NONE',  ( 0.05634301242525654313, -0.4396003943662976643, 0.1320237143668786528 ) ) ;
#15512 = LOCAL_TIME ( 0, 53, 7.000000000000000000, #22068 ) ;
#15513 = CARTESIAN_POINT ( 'NONE',  ( 0.1678804100208123595, -0.8181538232278317002, 0.2820814646259393044 ) ) ;
#15514 = CARTESIAN_POINT ( 'NONE',  ( -0.2746410161513782033, -2.376910030844113564, -0.7058185084100425666 ) ) ;
#15515 = AXIS2_PLACEMENT_3D ( 'NONE', #7279, #6685, #32190 ) ;
#15516 = CARTESIAN_POINT ( 'NONE',  ( 0.3137245967586478335, -1.174875666623787840, 0.5369163431172392364 ) ) ;
#15517 = CARTESIAN_POINT ( 'NONE',  ( 0.4199047739250627576, -1.021165802582503890, 0.6853183793762346321 ) ) ;
#15518 = APPROVAL_STATUS ( 'not_yet_approved' ) ;
#15519 = CARTESIAN_POINT ( 'NONE',  ( 0.3544453792448893359, -1.829125709028288194, -0.5151468183741818585 ) ) ;
#15520 = CARTESIAN_POINT ( 'NONE',  ( 0.4042633028793005678, -1.711240744073932563, 0.4220515681607865388 ) ) ;
#15521 = CARTESIAN_POINT ( 'NONE',  ( -0.05137569054209013830, -0.02238181648184470185, 0.4716086671401685804 ) ) ;
#15522 = B_SPLINE_CURVE_WITH_KNOTS ( 'NONE', 3,
 ( #12522, #634, #22215, #38219, #18918, #9647, #16028, #34733, #37610, #31454 ),
 .UNSPECIFIED., .F., .F.,
 ( 4, 2, 2, 2, 4 ),
 ( 0.000000000000000000, 0.0005856409713472994797, 0.001171281942694598959, 0.001756922914041898331, 0.002342563885389197919 ),
 .UNSPECIFIED. ) ;
#15523 = EDGE_CURVE ( 'NONE', #24870, #3369, #13733, .T. ) ;
#15524 = ORIENTED_EDGE ( 'NONE', *, *, #7670, .T. ) ;
#15525 = LINE ( 'NONE', #12423, #12160 ) ;
#15526 = CARTESIAN_POINT ( 'NONE',  ( -0.01548846960707447352, -0.2450655194479842147, 0.4674710490749294789 ) ) ;
#15527 = EDGE_CURVE ( 'NONE', #9403, #14602, #30370, .T. ) ;
#15528 = CARTESIAN_POINT ( 'NONE',  ( 0.2687203115727492264, -1.674044157977605529, 0.5754666865148680976 ) ) ;
#15529 = EDGE_LOOP ( 'NONE', ( #32931, #30677, #12618, #1531, #13358, #5495, #37322, #34034, #7119, #38390, #15084 ) ) ;
#15530 = AXIS2_PLACEMENT_3D ( 'NONE', #38244, #34565, #16446 ) ;
#15531 = CARTESIAN_POINT ( 'NONE',  ( -0.05076541221973657203, 0.04887304573182831707, -0.4712631214448597672 ) ) ;
#15532 = CARTESIAN_POINT ( 'NONE',  ( 0.1730569967621003735, -1.381888235275370080, 0.5682417262808804326 ) ) ;
#15534 = ORIENTED_EDGE ( 'NONE', *, *, #32123, .F. ) ;
#15533 = ORIENTED_EDGE ( 'NONE', *, *, #34325, .F. ) ;
#15535 = CARTESIAN_POINT ( 'NONE',  ( -0.2746410161513779258, -2.068584980338025847, -0.2731141320652226145 ) ) ;
#15536 = CARTESIAN_POINT ( 'NONE',  ( 0.01548846960707528191, 0.2306506793134049660, -0.4716198300880325434 ) ) ;
#15537 = APPROVAL_PERSON_ORGANIZATION ( #12910, #19454, #415 ) ;
#15538 = EDGE_CURVE ( 'NONE', #28751, #11876, #25040, .T. ) ;
#15539 = CARTESIAN_POINT ( 'NONE',  ( 0.3669548114133807659, -2.020640157311806462, -0.3128670423345359941 ) ) ;
#15540 = DIRECTION ( 'NONE',  ( 0.000000000000000000, 0.000000000000000000, 1.000000000000000000 ) ) ;
#15542 = CARTESIAN_POINT ( 'NONE',  ( 0.001045174848116913347, -0.9423331098586125165, 0.1457102695410935345 ) ) ;
#15541 = CARTESIAN_POINT ( 'NONE',  ( 0.02881302694829601663, 0.4889319715862826543, 0.09562644460326606699 ) ) ;
#15543 = CARTESIAN_POINT ( 'NONE',  ( 0.05201840200954449545, -0.2909588945328518417, -0.3697186091640858319 ) ) ;
#15544 = ORIENTED_EDGE ( 'NONE', *, *, #5096, .T. ) ;
#15545 = AXIS2_PLACEMENT_3D ( 'NONE', #19619, #726, #25797 ) ;
#15546 = CARTESIAN_POINT ( 'NONE',  ( 0.07601207264773035543, -1.311676598773741764, 0.5551002690229728254 ) ) ;
#15547 = ORIENTED_EDGE ( 'NONE', *, *, #29125, .T. ) ;
#15548 = CARTESIAN_POINT ( 'NONE',  ( 0.6864989062074844384, -1.545408043237719964, 0.6047936410314285194 ) ) ;
#15549 = CARTESIAN_POINT ( 'NONE',  ( 0.07292080638518497193, -0.5442452056136308780, 0.1818665249886239066 ) ) ;
#15550 = EDGE_CURVE ( 'NONE', #32833, #28034, #2795, .T. ) ;
#15552 = CARTESIAN_POINT ( 'NONE',  ( 0.6252338399778394340, -1.468100857423625838, 0.5182417262812428760 ) ) ;
#15551 = DIRECTION ( 'NONE',  ( -1.000000000000000000, 0.000000000000000000, 0.000000000000000000 ) ) ;
#15553 = CARTESIAN_POINT ( 'NONE',  ( 0.3519337645836231876, -1.625834341939006222, -0.3689444309192750904 ) ) ;
#15554 = EDGE_CURVE ( 'NONE', #5749, #12702, #21115, .T. ) ;
#15555 = DIRECTION ( 'NONE',  ( -1.000000000000000000, -0.000000000000000000, -0.000000000000000000 ) ) ;
#15556 = ADVANCED_FACE ( 'NONE', ( #11636 ), #17424, .T. ) ;
#15557 = CARTESIAN_POINT ( 'NONE',  ( 0.3962551329634386721, -2.018354224907537464, -0.4857151794559766422 ) ) ;
#15558 = CARTESIAN_POINT ( 'NONE',  ( 0.1252279186956127277, -0.5551208408591088439, 0.1884588093939131292 ) ) ;
#15559 = CARTESIAN_POINT ( 'NONE',  ( 0.4608582512679273435, -1.674906425203495530, 0.4445187640073551827 ) ) ;
#15560 = FACE_OUTER_BOUND ( 'NONE', #19662, .T. ) ;
#15561 = CARTESIAN_POINT ( 'NONE',  ( -0.02869712619511932336, 0.4892154842446466700, 0.09550911579581937427 ) ) ;
#15562 = DIRECTION ( 'NONE',  ( 0.000000000000000000, 0.6595282642760668113, 0.7516797646744247663 ) ) ;
#15563 = CARTESIAN_POINT ( 'NONE',  ( -2.112273405726188513E-14, -2.183180860297921466, -0.7137760292030871367 ) ) ;
#15564 = DIRECTION ( 'NONE',  ( -0.4999551463232372317, 0.8660512985181135770, -0.000000000000000000 ) ) ;
#15565 = TOROIDAL_SURFACE ( 'NONE', #22163, 0.5250000000000000222, 0.01499999999999999944 ) ;
#15566 = CARTESIAN_POINT ( 'NONE',  ( 0.1895831464430141888, -0.5047047246472139426, 0.1503823323309240734 ) ) ;
#15567 = CARTESIAN_POINT ( 'NONE',  ( -0.05491348488830515018, 0.2919908616877288088, 0.3589493610278767788 ) ) ;
#15568 = CARTESIAN_POINT ( 'NONE',  ( 0.04836495276552613132, -1.258574261489486812, 0.6520114206213487584 ) ) ;
#15569 = ORGANIZATION ( 'NAUO-ORG17', 'UNSPECIFIED', 'UNSPECIFIED' ) ;
#15570 = CARTESIAN_POINT ( 'NONE',  ( 0.6100990983602245787, -1.580768839995616126, -0.4597541041496203129 ) ) ;
#15571 = CARTESIAN_POINT ( 'NONE',  ( 0.1614573949321077284, -0.7569534866611321577, 0.1932149833450299559 ) ) ;
#15572 = CARTESIAN_POINT ( 'NONE',  ( 0.1645591421022416789, -0.8833852852294274971, 0.5507895711055610377 ) ) ;
#15573 = CARTESIAN_POINT ( 'NONE',  ( 0.04154009738085474857, 0.2622554993748598684, -0.3904256972020298533 ) ) ;
#15574 = VECTOR ( 'NONE', #27083, 39.37007874015748143 ) ;
#15575 = CARTESIAN_POINT ( 'NONE',  ( -0.2746410161513782033, -2.461298705151934829, -0.7594706439553173816 ) ) ;
#15576 = EDGE_LOOP ( 'NONE', ( #13192, #1019, #10079, #36679 ) ) ;
#15577 = CARTESIAN_POINT ( 'NONE',  ( 0.05999999999999990757, 0.000000000000000000, 0.000000000000000000 ) ) ;
#15578 = FACE_OUTER_BOUND ( 'NONE', #33858, .T. ) ;
#15579 = CARTESIAN_POINT ( 'NONE',  ( 0.000000000000000000, -0.02999999999999995379, 0.000000000000000000 ) ) ;
#15580 = EDGE_CURVE ( 'NONE', #30555, #27179, #37792, .T. ) ;
#15581 = CARTESIAN_POINT ( 'NONE',  ( -2.070754768975505034, -0.09959325338431362917, 0.3606502365330779836 ) ) ;
#15582 = CARTESIAN_POINT ( 'NONE',  ( 0.3640014500131175113, -1.990332505625297843, -0.4924098530529640860 ) ) ;
#15583 = EDGE_CURVE ( 'NONE', #11795, #26731, #14585, .T. ) ;
#15584 = ORIENTED_EDGE ( 'NONE', *, *, #3635, .T. ) ;
#15585 = CARTESIAN_POINT ( 'NONE',  ( 0.5450221536532190436, -1.653079618865306299, -0.5489132167387396066 ) ) ;
#15586 = CARTESIAN_POINT ( 'NONE',  ( 0.1802237425427333228, -0.5041004908202411094, 0.1773551390588752052 ) ) ;
#15587 = DIRECTION ( 'NONE',  ( 0.1565050148243877226, -0.9876771640241653882, 0.000000000000000000 ) ) ;
#15588 = CARTESIAN_POINT ( 'NONE',  ( 0.04946288932099957708, 0.2513464261306859737, -0.4057664802068605692 ) ) ;
#15589 = CARTESIAN_POINT ( 'NONE',  ( 0.5012889143793337610, -1.295578934310636976, 0.5940465434816246670 ) ) ;
#15591 = VERTEX_POINT ( 'NONE', #15926 ) ;
#15590 = DIRECTION ( 'NONE',  ( 0.9378410757839553691, 0.2807814858886550913, -0.2039996905746478406 ) ) ;
#15592 = CARTESIAN_POINT ( 'NONE',  ( 0.2471460726071840197, -0.9121693139129607442, 0.4829066783201274027 ) ) ;
#15593 = CIRCLE ( 'NONE', #38570, 0.2499999999999999722 ) ;
#15594 = EDGE_LOOP ( 'NONE', ( #21362, #3479, #2678, #13024 ) ) ;
#15595 = PERSON_AND_ORGANIZATION_ROLE ( 'design_owner' ) ;
#15596 = LINE ( 'NONE', #37195, #14516 ) ;
#15597 = ORIENTED_EDGE ( 'NONE', *, *, #19748, .F. ) ;
#15598 = ORIENTED_EDGE ( 'NONE', *, *, #10901, .T. ) ;
#15599 = CARTESIAN_POINT ( 'NONE',  ( 0.3549369896887015763, -1.516628842544784472, 0.8323203099904163960 ) ) ;
#15601 = CARTESIAN_POINT ( 'NONE',  ( 0.1115015552682263461, -0.8978746070190919415, 0.02774221936830248078 ) ) ;
#15600 = LINE ( 'NONE', #2447, #39725 ) ;
#15602 = DIRECTION ( 'NONE',  ( 0.4999551463232372317, -0.8660512985181133550, 0.000000000000000000 ) ) ;
#15603 = ORIENTED_EDGE ( 'NONE', *, *, #35075, .F. ) ;
#15604 = ORIENTED_EDGE ( 'NONE', *, *, #5882, .F. ) ;
#15605 = ORIENTED_EDGE ( 'NONE', *, *, #32047, .T. ) ;
#15606 = CARTESIAN_POINT ( 'NONE',  ( 0.3621525574119358049, -1.086908716195545743, 0.6383390412752412146 ) ) ;
#15607 = CARTESIAN_POINT ( 'NONE',  ( 0.1617007434535638888, -0.7254083217123186156, 0.5341668825669240173 ) ) ;
#15608 = ORIENTED_EDGE ( 'NONE', *, *, #26845, .F. ) ;
#15609 = CARTESIAN_POINT ( 'NONE',  ( 0.2046676961208400425, -1.998811770563726720, -0.3203772732607386708 ) ) ;
#15610 = CARTESIAN_POINT ( 'NONE',  ( 0.01548846960706681299, -0.09061086148575756005, 0.5171215251571267268 ) ) ;
#15611 = DIRECTION ( 'NONE',  ( 1.000000000000000000, 1.188678714063518030E-15, -6.695352868347822093E-17 ) ) ;
#15612 = CARTESIAN_POINT ( 'NONE',  ( 0.3666666666666453800, -2.097675824466503691, -0.2588528740066097233 ) ) ;
#15613 = CARTESIAN_POINT ( 'NONE',  ( 0.4343863265072839264, -1.688740028300337981, 0.4182417262807859859 ) ) ;
#15614 = CARTESIAN_POINT ( 'NONE',  ( 0.07014435923142441076, -1.325199841737237261, 0.5075297796642793680 ) ) ;
#15615 = DIRECTION ( 'NONE',  ( -4.419165872103955473E-15, 0.3420201433256692680, -0.9396926207859082059 ) ) ;
#15616 = PLANE ( 'NONE',  #11524 ) ;
#15617 = CARTESIAN_POINT ( 'NONE',  ( 0.4115766028365042128, -1.733048369835246794, 0.5182417262812423209 ) ) ;
#15618 = CALENDAR_DATE ( 2026, 13, 10 ) ;
#15619 = CARTESIAN_POINT ( 'NONE',  ( 0.3310978894898223834, -0.9939147606493616838, 0.5922533870212514095 ) ) ;
#15620 = CARTESIAN_POINT ( 'NONE',  ( 0.7521323256515352051, -1.545065466920227282, -0.5155029497116575543 ) ) ;
#15621 = CARTESIAN_POINT ( 'NONE',  ( 0.5434173516999434295, -1.168945995238640068, 0.6057417262810176339 ) ) ;
#15622 = CARTESIAN_POINT ( 'NONE',  ( 0.01548846960707524721, 0.5198120922912040642, 0.07362328916749247276 ) ) ;
#15623 =( BOUNDED_SURFACE ( )  B_SPLINE_SURFACE ( 3, 2, ( 
 ( #21671, #24350, #24955 ),
 ( #21485, #27636, #2740 ),
 ( #40166, #24167, #34006 ),
 ( #5810, #5398, #30309 ),
 ( #30521, #30916, #15285 ),
 ( #14887, #27844, #24768 ),
 ( #27446, #28055, #8304 ),
 ( #20875, #33396, #39971 ),
 ( #37291, #34200, #11792 ),
 ( #6011, #18576, #31134 ) ),
 .UNSPECIFIED., .F., .F., .T. ) 
 B_SPLINE_SURFACE_WITH_KNOTS ( ( 4, 2, 2, 2, 4 ),
 ( 3, 3 ),
 ( 0.0007871759377455164221, 0.001415437681796649161, 0.002043699425847781900, 0.002671961169898914856, 0.003300222913950047812 ),
 ( 0.000000000000000000, 0.6905130149310136911 ),
 .UNSPECIFIED. ) 
 GEOMETRIC_REPRESENTATION_ITEM ( )  RATIONAL_B_SPLINE_SURFACE ( (
 ( 1.000000000000000000, 0.7888811462077213177, 0.8693229248972149659),
 ( 1.000000000000000000, 0.8426938665563540320, 0.9026315980553327734),
 ( 1.000000000000000000, 0.8781792394491754195, 0.9245961201966287346),
 ( 1.000000000000000000, 0.9251411795240688241, 0.9536643386901670905),
 ( 1.000000000000000000, 0.9360575408707458855, 0.9604212822123805449),
 ( 1.000000000000000000, 0.9355106661221218589, 0.9600827809780565492),
 ( 1.000000000000000000, 0.9241077274843783051, 0.9530246587782127410),
 ( 1.000000000000000000, 0.8766085888055522579, 0.9236239283320455407),
 ( 1.000000000000000000, 0.8402078199309059858, 0.9010927999056310700),
 ( 1.000000000000000000, 0.7857264936582148973, 0.8673702770842413035) ) ) 
 REPRESENTATION_ITEM ( '' )  SURFACE ( )  );
#15624 = CARTESIAN_POINT ( 'NONE',  ( 0.1872829031602858685, -1.532932250049839906, 0.6789365607098191147 ) ) ;
#15625 = CARTESIAN_POINT ( 'NONE',  ( 0.2713753197625269342, -1.672371506024731724, 0.4877530470170145516 ) ) ;
#15626 = CARTESIAN_POINT ( 'NONE',  ( 0.6646178349955912390, -1.445333687840241410, 0.4440966220229920491 ) ) ;
#15627 = CIRCLE ( 'NONE', #28757, 0.08000000000000002942 ) ;
#15628 = ORIENTED_EDGE ( 'NONE', *, *, #8372, .F. ) ;
#15629 = VERTEX_POINT ( 'NONE', #6044 ) ;
#15630 = CARTESIAN_POINT ( 'NONE',  ( -0.1210148435730069999, -0.5061394519556974281, 0.1438724812235067374 ) ) ;
#15631 = ORIENTED_EDGE ( 'NONE', *, *, #31371, .T. ) ;
#15632 = CARTESIAN_POINT ( 'NONE',  ( -0.02235124290213174117, 0.07000983313419843757, 0.5077112423787081275 ) ) ;
#15633 = CARTESIAN_POINT ( 'NONE',  ( 0.03158843595483476485, 0.2432919444504248463, 0.4277514783322106662 ) ) ;
#15634 = CARTESIAN_POINT ( 'NONE',  ( 0.5767692940198798635, -1.426262227725163090, 0.5925100300099771511 ) ) ;
#15636 = ORIENTED_EDGE ( 'NONE', *, *, #38154, .T. ) ;
#15635 = CARTESIAN_POINT ( 'NONE',  ( 0.01043330323478177529, -0.5303232461374860485, 0.1276616220108156841 ) ) ;
#15637 = VERTEX_POINT ( 'NONE', #18612 ) ;
#15638 = CARTESIAN_POINT ( 'NONE',  ( 0.01548846960712810944, 0.4730347584885798429, -0.2341461249029115899 ) ) ;
#15639 = VERTEX_POINT ( 'NONE', #9336 ) ;
#15640 = CARTESIAN_POINT ( 'NONE',  ( 0.01139561368625759304, -0.5503006985288143582, 0.2442491123753702531 ) ) ;
#15642 = DIRECTION ( 'NONE',  ( 0.8660512985181134660, 0.4999551463232372317, 0.000000000000000000 ) ) ;
#15641 = CARTESIAN_POINT ( 'NONE',  ( 0.5030897103603338971, -1.688833090595270425, -0.4393626442577572844 ) ) ;
#15643 = CARTESIAN_POINT ( 'NONE',  ( 0.01208307744763006952, -0.4513789697288763669, 0.03872339057219081199 ) ) ;
#15644 = CARTESIAN_POINT ( 'NONE',  ( -0.1167294260180219145, -0.5331983351046741815, 0.3082670712250488720 ) ) ;
#15646 = VERTEX_POINT ( 'NONE', #40615 ) ;
#15645 = ORIENTED_EDGE ( 'NONE', *, *, #4851, .T. ) ;
#15647 = CARTESIAN_POINT ( 'NONE',  ( 0.3925301276612754298, -1.756377271995033684, -0.4843757382520948451 ) ) ;
#15648 = CARTESIAN_POINT ( 'NONE',  ( -0.02000000000000000042, -2.124839267114085217, -0.6708880114557002061 ) ) ;
#15649 = CARTESIAN_POINT ( 'NONE',  ( -0.05634490452572756686, -0.4348542811545100251, 0.1466173361067427960 ) ) ;
#15650 = CARTESIAN_POINT ( 'NONE',  ( 0.2475591123417469619, -0.9465702229060155570, 0.7371952982553420242 ) ) ;
#15651 = CARTESIAN_POINT ( 'NONE',  ( 0.2702137124954268610, -0.9931619662810967641, 0.7111678352231335376 ) ) ;
#15652 = CARTESIAN_POINT ( 'NONE',  ( 0.2702327675951550767, -1.674551853183180894, 0.5944435164687253970 ) ) ;
#15653 = CARTESIAN_POINT ( 'NONE',  ( -0.1071618391680910221, -0.4882221650595575113, 0.3591756789878951528 ) ) ;
#15654 = CIRCLE ( 'NONE', #38635, 0.1600000000000006417 ) ;
#15655 = CARTESIAN_POINT ( 'NONE',  ( 0.07779920321647403048, -1.322114474344633583, 0.5682417262808776570 ) ) ;
#15656 = DIRECTION ( 'NONE',  ( 0.4108529743908185816, -0.9117016142544761559, 0.000000000000000000 ) ) ;
#15657 = FACE_OUTER_BOUND ( 'NONE', #31973, .T. ) ;
#15658 = CARTESIAN_POINT ( 'NONE',  ( -0.2550000000000000044, -3.941790907013290823, -0.4709369376873033253 ) ) ;
#15659 = CARTESIAN_POINT ( 'NONE',  ( 0.04157143636675726672, -0.2624507507128635564, 0.3902120892151791365 ) ) ;
#15660 = DIRECTION ( 'NONE',  ( 0.000000000000000000, 0.6595282642760672553, 0.7516797646744243222 ) ) ;
#15661 = CARTESIAN_POINT ( 'NONE',  ( 0.08861282632252902303, -1.303734040091387714, 0.7233710302893093802 ) ) ;
#15662 = PERSON_AND_ORGANIZATION_ROLE ( 'design_supplier' ) ;
#15663 = CARTESIAN_POINT ( 'NONE',  ( 0.7167626400851214719, -1.479603991551655895, 0.4558490598962456342 ) ) ;
#15664 = CARTESIAN_POINT ( 'NONE',  ( -0.04946288932099660030, 0.4418470831553492073, 0.1805342557390142155 ) ) ;
#15665 = DIRECTION ( 'NONE',  ( 1.000000000000000000, 6.779273404243070203E-32, 4.314083075427408311E-32 ) ) ;
#15666 = LINE ( 'NONE', #37675, #8115 ) ;
#15667 = ADVANCED_FACE ( 'NONE', ( #5650 ), #37324, .T. ) ;
#15668 = DIRECTION ( 'NONE',  ( 0.000000000000000000, 0.9901182710308679136, -0.1402348365094949756 ) ) ;
#15669 = ORIENTED_EDGE ( 'NONE', *, *, #35522, .T. ) ;
#15670 = CARTESIAN_POINT ( 'NONE',  ( 0.05999999999999990757, -0.3458405862425447119, -0.1052451372150005060 ) ) ;
#15671 = APPLIED_DATE_AND_TIME_ASSIGNMENT ( #36459, #14431, ( #35536 ) ) ;
#15672 = CARTESIAN_POINT ( 'NONE',  ( 0.2544140537756520715, -1.595280948316114999, 0.8480660740215214544 ) ) ;
#15674 = VERTEX_POINT ( 'NONE', #28472 ) ;
#15673 = CARTESIAN_POINT ( 'NONE',  ( 0.5766093525687170374, -1.458620651149859171, 0.7164759587684025322 ) ) ;
#15676 = ORIENTED_EDGE ( 'NONE', *, *, #34653, .F. ) ;
#15675 = DIRECTION ( 'NONE',  ( 0.000000000000000000, 0.000000000000000000, -1.000000000000000000 ) ) ;
#15677 = CARTESIAN_POINT ( 'NONE',  ( 0.3484275328463246058, -0.9131724924592886650, 0.6749714385622568313 ) ) ;
#15679 = VERTEX_POINT ( 'NONE', #24382 ) ;
#15678 = ORIENTED_EDGE ( 'NONE', *, *, #29544, .F. ) ;
#15680 = CARTESIAN_POINT ( 'NONE',  ( 0.6762931815487975840, -1.394502623830513155, 0.7319977833246720245 ) ) ;
#15681 = CARTESIAN_POINT ( 'NONE',  ( 0.3733765242244403426, -1.670306735275899568, -0.6070209750880516397 ) ) ;
#15682 = LINE ( 'NONE', #33800, #16069 ) ;
#15683 = DIRECTION ( 'NONE',  ( 1.000000000000000000, -0.000000000000000000, -0.000000000000000000 ) ) ;
#15684 = ORIENTED_EDGE ( 'NONE', *, *, #9267, .T. ) ;
#15685 = CARTESIAN_POINT ( 'NONE',  ( 0.2245517771038092192, -0.9157708072603734095, 0.6589336320736243202 ) ) ;
#15686 = CARTESIAN_POINT ( 'NONE',  ( 0.1757500541653520820, -1.230771478115229245, -0.4400554600884079570 ) ) ;
#15687 = CARTESIAN_POINT ( 'NONE',  ( 0.5264717665343396913, -1.526446698549486891, 0.6019642009783892078 ) ) ;
#15688 = EDGE_CURVE ( 'NONE', #13751, #4342, #28457, .T. ) ;
#15689 = DIRECTION ( 'NONE',  ( 7.771561172376107616E-16, -7.170354002788761615E-17, 1.000000000000000000 ) ) ;
#15690 = CARTESIAN_POINT ( 'NONE',  ( -0.1656815030311168946, 0.4813244629265746033, 0.1225468705240551348 ) ) ;
#15691 = ORIENTED_EDGE ( 'NONE', *, *, #10399, .F. ) ;
#15692 = CARTESIAN_POINT ( 'NONE',  ( 0.4697787318353889852, -1.672242315053772854, 0.5632612846970690423 ) ) ;
#15693 = CARTESIAN_POINT ( 'NONE',  ( 0.7441773965511153666, -1.515035653583309827, 0.6063620325133788347 ) ) ;
#15694 = EDGE_CURVE ( 'NONE', #36543, #28382, #6260, .T. ) ;
#15695 = DIRECTION ( 'NONE',  ( 1.000000000000000000, 6.779273404243070203E-32, 4.314083075427408311E-32 ) ) ;
#15696 = EDGE_CURVE ( 'NONE', #30207, #20390, #39535, .T. ) ;
#15697 = FACE_OUTER_BOUND ( 'NONE', #11135, .T. ) ;
#15698 =( NAMED_UNIT ( * ) PLANE_ANGLE_UNIT ( ) SI_UNIT ( $, .RADIAN. ) );
#15699 = EDGE_CURVE ( 'NONE', #2068, #16485, #21181, .T. ) ;
#15700 = CARTESIAN_POINT ( 'NONE',  ( 0.5779297624755960205, -1.623152544610868109, 0.5629341535590222101 ) ) ;
#15701 = CARTESIAN_POINT ( 'NONE',  ( 0.2710216717077167936, -1.672577861558078416, 0.4888899872315822237 ) ) ;
#15702 = EDGE_CURVE ( 'NONE', #25927, #433, #24472, .T. ) ;
#15703 = CARTESIAN_POINT ( 'NONE',  ( 0.04206944528682795420, -1.152159445897246393, 0.6964886360393780507 ) ) ;
#15704 = CARTESIAN_POINT ( 'NONE',  ( 0.5130887424854349010, -1.117175276521638505, 0.5842416974757255188 ) ) ;
#15705 = CALENDAR_DATE ( 2026, 13, 10 ) ;
#15706 = CARTESIAN_POINT ( 'NONE',  ( 0.3616412802241143476, -1.759290408630900693, -0.5212859374495405484 ) ) ;
#15707 = ORIENTED_EDGE ( 'NONE', *, *, #28760, .F. ) ;
#15708 = CARTESIAN_POINT ( 'NONE',  ( 0.5612712793085452567, -1.506471590370649372, 0.5726843098148547417 ) ) ;
#15709 = CARTESIAN_POINT ( 'NONE',  ( -0.04087116408467007800, 0.02106952151319393951, 0.4712677373718177076 ) ) ;
#15710 = EDGE_CURVE ( 'NONE', #26723, #19496, #2116, .T. ) ;
#15711 = VERTEX_POINT ( 'NONE', #37514 ) ;
#15712 = LINE ( 'NONE', #28259, #6242 ) ;
#15713 = PRODUCT_RELATED_PRODUCT_CATEGORY ( 'detail', '', ( #27114 ) ) ;
#15714 = CARTESIAN_POINT ( 'NONE',  ( -0.3000000000000000999, -3.985676108854518507, -0.6623095129438225648 ) ) ;
#15715 = ORIENTED_EDGE ( 'NONE', *, *, #19465, .F. ) ;
#15716 = CARTESIAN_POINT ( 'NONE',  ( -0.03301200226531962600, -0.08829440931814541704, -0.5134711413293201465 ) ) ;
#15717 = CARTESIAN_POINT ( 'NONE',  ( 0.02680226611402111714, -1.057819507791903257, 0.7331982514440371634 ) ) ;
#15719 = ORIENTED_EDGE ( 'NONE', *, *, #21595, .T. ) ;
#15718 = EDGE_LOOP ( 'NONE', ( #1205, #29248, #18560, #20352 ) ) ;
#15720 = DIRECTION ( 'NONE',  ( 0.000000000000000000, 0.000000000000000000, -1.000000000000000000 ) ) ;
#15721 = ORIENTED_EDGE ( 'NONE', *, *, #29866, .F. ) ;
#15722 = FACE_OUTER_BOUND ( 'NONE', #22532, .T. ) ;
#15723 = CARTESIAN_POINT ( 'NONE',  ( 0.3613124228137278293, -1.955507677535348376, -0.4996853815432704682 ) ) ;
#15725 = CARTESIAN_POINT ( 'NONE',  ( 0.1676694287369189240, -1.385544946528693089, 0.5182417262812420988 ) ) ;
#15724 = CARTESIAN_POINT ( 'NONE',  ( 0.05999999999999990757, 0.000000000000000000, 0.000000000000000000 ) ) ;
#15726 = CARTESIAN_POINT ( 'NONE',  ( -0.004088490883478934287, -1.369644552158580053, -0.6494983983435047570 ) ) ;
#15727 = VERTEX_POINT ( 'NONE', #21917 ) ;
#15728 = CARTESIAN_POINT ( 'NONE',  ( 0.1032975704182374083, -0.6446288055514268756, 0.3563257787039654234 ) ) ;
#15729 = ORIENTED_EDGE ( 'NONE', *, *, #31848, .T. ) ;
#15730 = CYLINDRICAL_SURFACE ( 'NONE', #2989, 0.01499999999999999424 ) ;
#15731 = CARTESIAN_POINT ( 'NONE',  ( 0.07376662319119976774, -0.5594476950009685812, 0.2363562539228321879 ) ) ;
#15733 = CARTESIAN_POINT ( 'NONE',  ( 0.5631207333134724546, -1.617530675893939174, 0.5006452510992012161 ) ) ;
#15732 = CARTESIAN_POINT ( 'NONE',  ( 0.4875928425406638733, -1.627410370986559940, -0.4328921880033906322 ) ) ;
#15734 = CARTESIAN_POINT ( 'NONE',  ( -1.496393162519607993E-15, -0.3899999999999999578, -0.04999999999999946848 ) ) ;
#15735 = CARTESIAN_POINT ( 'NONE',  ( 0.3754938372491893328, -1.052735747919861797, 0.6361273785642954648 ) ) ;
#15736 = VERTEX_POINT ( 'NONE', #34444 ) ;
#15737 = UNCERTAINTY_MEASURE_WITH_UNIT (LENGTH_MEASURE( 1.000000000000000082E-05 ), #1126, 'distance_accuracy_value', 'NONE');
#15738 = CARTESIAN_POINT ( 'NONE',  ( 0.3827394763927673971, -1.608088298394132254, 0.5182417262812428760 ) ) ;
#15739 = CARTESIAN_POINT ( 'NONE',  ( 0.1887415726803808591, -0.4595355292632672395, 0.1470298804553386296 ) ) ;
#15740 = CARTESIAN_POINT ( 'NONE',  ( 0.5808744538588486162, -1.495254402632689050, 0.5726140762454942079 ) ) ;
#15741 = CARTESIAN_POINT ( 'NONE',  ( -0.04308449196698704159, 0.3346410801914455058, -0.3638139224395092741 ) ) ;
#15742 = EDGE_CURVE ( 'NONE', #22474, #22431, #11307, .T. ) ;
#15743 = DIRECTION ( 'NONE',  ( -0.2929646265539834760, -0.1592115978499541173, 0.9427743074024396153 ) ) ;
#15744 = FACE_OUTER_BOUND ( 'NONE', #11983, .T. ) ;
#15745 = EDGE_CURVE ( 'NONE', #10169, #36413, #36251, .T. ) ;
#15746 = CARTESIAN_POINT ( 'NONE',  ( -0.1515422989582873303, 0.4690188198402805986, 0.3602693336111434386 ) ) ;
#15747 = CARTESIAN_POINT ( 'NONE',  ( 0.4315909263077353786, -1.207668101024179430, 0.5182417262812423209 ) ) ;
#15748 = EDGE_CURVE ( 'NONE', #9066, #1786, #18530, .T. ) ;
#15749 = CARTESIAN_POINT ( 'NONE',  ( 0.3234650319091952331, -0.8156164872106268504, 0.7066254915499745604 ) ) ;
#15750 = CARTESIAN_POINT ( 'NONE',  ( -0.01899468245560667276, 0.2428515268394236537, 0.4597785848521163676 ) ) ;
#15751 = CARTESIAN_POINT ( 'NONE',  ( 0.03483016372457843624, -1.090556708997785229, 0.6345047942266013319 ) ) ;
#15752 = CARTESIAN_POINT ( 'NONE',  ( 0.6283006780106592526, -1.606940092472771031, -0.4564006025841033098 ) ) ;
#15753 = ADVANCED_FACE ( 'NONE', ( #9557 ), #22134, .F. ) ;
#15754 = CARTESIAN_POINT ( 'NONE',  ( 0.1963401049631460227, -0.6876817530555039415, 0.3329214951892821017 ) ) ;
#15755 = CARTESIAN_POINT ( 'NONE',  ( 0.08509807014988972351, -0.8316410974579127036, 0.1457185332388699350 ) ) ;
#15756 = CARTESIAN_POINT ( 'NONE',  ( 0.4062230848227149638, -1.145582794160931117, 0.4248905050063955802 ) ) ;
#15757 = DIRECTION ( 'NONE',  ( 2.526820087036053001E-31, 0.1402348365095093807, -0.9901182710308659152 ) ) ;
#15758 = ADVANCED_FACE ( 'NONE', ( #9752 ), #10167, .T. ) ;
#15759 = ADVANCED_FACE ( 'NONE', ( #22737 ), #3976, .F. ) ;
#15760 = ORIENTED_EDGE ( 'NONE', *, *, #32319, .F. ) ;
#15761 = CARTESIAN_POINT ( 'NONE',  ( -0.08000000000000000167, -2.004218822785767795, -0.4035264592197354561 ) ) ;
#15762 = CARTESIAN_POINT ( 'NONE',  ( 0.4137599315576318548, -1.590143257116449105, -0.4137273532990809466 ) ) ;
#15763 = EDGE_CURVE ( 'NONE', #2769, #30547, #35265, .T. ) ;
#15764 = CARTESIAN_POINT ( 'NONE',  ( 0.6632759560342388339, -1.473865492997792570, 0.4224349526775863506 ) ) ;
#15765 = CARTESIAN_POINT ( 'NONE',  ( 0.07016588152529044942, -0.8342740451934566037, 0.1457185332388703236 ) ) ;
#15766 = CARTESIAN_POINT ( 'NONE',  ( -0.07908070219615623286, -0.09959325338431362917, 0.1178658435936968396 ) ) ;
#15767 = EDGE_CURVE ( 'NONE', #15491, #37479, #29715, .T. ) ;
#15768 = ORIENTED_EDGE ( 'NONE', *, *, #13695, .T. ) ;
#15769 = DIRECTION ( 'NONE',  ( -1.252096997096122269E-14, -0.9672079024912928480, 0.2539859707905023356 ) ) ;
#15770 = EDGE_CURVE ( 'NONE', #15212, #26023, #38902, .T. ) ;
#15771 = DIRECTION ( 'NONE',  ( 1.000000000000000000, 2.341930812374887555E-31, -1.664003471950578127E-31 ) ) ;
#15772 = CARTESIAN_POINT ( 'NONE',  ( 0.4749432869989659856, -1.666646186687757547, 0.4653120090430740707 ) ) ;
#15773 = CARTESIAN_POINT ( 'NONE',  ( 0.04762035657659002136, 0.3170509070583803490, -0.3633072608571736861 ) ) ;
#15774 = CARTESIAN_POINT ( 'NONE',  ( 0.4662960040860855138, -1.240302083570733016, 0.7040906853573337676 ) ) ;
#15776 = CARTESIAN_POINT ( 'NONE',  ( -0.1157923916715208196, -0.5295015842444287246, 0.3181161673586317962 ) ) ;
#15775 = DIRECTION ( 'NONE',  ( 0.8660254037844385966, 0.4219433715391051054, 0.2682606777263730202 ) ) ;
#15777 = CARTESIAN_POINT ( 'NONE',  ( 0.4737957855049246270, -1.072208190283344909, 0.6181471139717461538 ) ) ;
#15778 = ORIENTED_EDGE ( 'NONE', *, *, #30348, .T. ) ;
#15779 = COORDINATED_UNIVERSAL_TIME_OFFSET ( 0, 0, .AHEAD. ) ;
#15780 = CARTESIAN_POINT ( 'NONE',  ( 0.01749918469671574162, -0.9360414646517258852, 0.5901500853657657419 ) ) ;
#15781 = EDGE_LOOP ( 'NONE', ( #26953, #21423, #15940, #27828, #1601 ) ) ;
#15782 = ORIENTED_EDGE ( 'NONE', *, *, #19251, .F. ) ;
#15783 = CARTESIAN_POINT ( 'NONE',  ( 0.3878444664605486536, -1.599983213115868441, 0.6642460123331223043 ) ) ;
#15785 = CARTESIAN_POINT ( 'NONE',  ( 0.1848348008737195070, -0.8303121680794297577, 0.06024004532681473401 ) ) ;
#15784 = DIRECTION ( 'NONE',  ( -1.000000000000000000, -2.280301054154495132E-31, 1.664003471950577689E-31 ) ) ;
#15786 = CARTESIAN_POINT ( 'NONE',  ( 0.06840157109000070956, -0.5700798809208006412, 0.05578865808313797359 ) ) ;
#15787 = EDGE_LOOP ( 'NONE', ( #33987, #36585, #16596, #32963 ) ) ;
#15788 = AXIS2_PLACEMENT_3D ( 'NONE', #5940, #21809, #12533 ) ;
#15789 = EDGE_LOOP ( 'NONE', ( #10015, #40613, #7977, #4203 ) ) ;
#15790 = EDGE_LOOP ( 'NONE', ( #1347, #9796, #5835, #28845, #24627 ) ) ;
#15791 = ORIENTED_EDGE ( 'NONE', *, *, #11671, .F. ) ;
#15792 = CARTESIAN_POINT ( 'NONE',  ( 0.05999999999999990757, 0.000000000000000000, 0.000000000000000000 ) ) ;
#15793 = CARTESIAN_POINT ( 'NONE',  ( 0.5643467867757225864, -1.493973552341269162, 0.6681583330584175417 ) ) ;
#15794 = EDGE_LOOP ( 'NONE', ( #40624, #7935, #9658, #39549, #31470, #6324, #16121, #20144, #465 ) ) ;
#15795 = CARTESIAN_POINT ( 'NONE',  ( 0.1854530118307023689, -0.8267686003446883536, 0.1092990128771291342 ) ) ;
#15796 = CARTESIAN_POINT ( 'NONE',  ( 0.4713981431917049214, -1.069104614441775958, -0.6069517949360595521 ) ) ;
#15797 = DIRECTION ( 'NONE',  ( 1.000000000000000000, 0.000000000000000000, 0.000000000000000000 ) ) ;
#15798 = AXIS2_PLACEMENT_3D ( 'NONE', #35602, #19981, #4336 ) ;
#15799 = DIRECTION ( 'NONE',  ( -1.000000000000000000, 0.000000000000000000, 0.000000000000000000 ) ) ;
#15800 = VERTEX_POINT ( 'NONE', #19632 ) ;
#15801 = EDGE_CURVE ( 'NONE', #11795, #29903, #830, .T. ) ;
#15802 = CARTESIAN_POINT ( 'NONE',  ( 0.3159174789885340617, -1.473577620167767277, -0.2869361388274797586 ) ) ;
#15803 = FACE_OUTER_BOUND ( 'NONE', #2451, .T. ) ;
#15804 = ADVANCED_FACE ( 'NONE', ( #37942 ), #23158, .T. ) ;
#15805 = CARTESIAN_POINT ( 'NONE',  ( 0.3999999999999787059, -2.166079853131637645, -0.5407606602423824516 ) ) ;
#15806 = FACE_OUTER_BOUND ( 'NONE', #26258, .T. ) ;
#15807 = CARTESIAN_POINT ( 'NONE',  ( 0.2186326339716475331, -1.240032810101609373, 0.5763875373488478449 ) ) ;
#15808 = CARTESIAN_POINT ( 'NONE',  ( 0.2408414484411625089, -1.826577308757157958, -0.6567176230664488745 ) ) ;
#15809 = CARTESIAN_POINT ( 'NONE',  ( 0.3507599413761057772, -1.722433222888394289, -0.4396544696549837816 ) ) ;
#15810 = DATE_AND_TIME ( #25073, #34473 ) ;
#15811 = CARTESIAN_POINT ( 'NONE',  ( 0.2042269006659602204, -0.9243050108670398668, 0.3357924985444922794 ) ) ;
#15812 = CARTESIAN_POINT ( 'NONE',  ( 0.1802068938276927546, -1.378362688417822834, 0.4882610536917470490 ) ) ;
#15813 = CARTESIAN_POINT ( 'NONE',  ( -0.3000000000000000999, -1.835749455202394298, -0.2938319975228648739 ) ) ;
#15815 = ORIENTED_EDGE ( 'NONE', *, *, #36074, .T. ) ;
#15814 = CARTESIAN_POINT ( 'NONE',  ( 0.2923286432308245808, -1.660243258845594649, -0.6250000000000000000 ) ) ;
#15816 = CARTESIAN_POINT ( 'NONE',  ( -0.002083146443013338383, -0.8967360763018588088, 0.1457185332388704624 ) ) ;
#15817 = CARTESIAN_POINT ( 'NONE',  ( 0.0001225610919479534636, -0.5774639562824842587, -0.07786294252879151501 ) ) ;
#15818 = CARTESIAN_POINT ( 'NONE',  ( 0.2265531926702374077, -1.599072214040516249, -0.6987977643162676111 ) ) ;
#15819 = TOROIDAL_SURFACE ( 'NONE', #21726, 1.971674066779348866, 0.02999999999999999889 ) ;
#15820 = DIRECTION ( 'NONE',  ( 0.000000000000000000, 0.3306821564015692827, 0.9437421848352484099 ) ) ;
#15821 = EDGE_CURVE ( 'NONE', #12108, #39819, #13246, .T. ) ;
#15822 = ORIENTED_EDGE ( 'NONE', *, *, #19187, .F. ) ;
#15823 = VERTEX_POINT ( 'NONE', #3584 ) ;
#15824 = CONICAL_SURFACE ( 'NONE', #17779, 0.1946589359789742957, 1.047197551196600962 ) ;
#15825 = CARTESIAN_POINT ( 'NONE',  ( 0.05283102792148709759, -0.3063958269170704574, -0.3541938269410525031 ) ) ;
#15826 = EDGE_LOOP ( 'NONE', ( #20152, #18898, #18887, #2724 ) ) ;
#15827 = DIRECTION ( 'NONE',  ( 0.5794373887239167020, -0.8150167559926659866, -6.834394190886211068E-17 ) ) ;
#15828 = CARTESIAN_POINT ( 'NONE',  ( 0.03868264068766669866, 0.3066108573455321729, 0.3648330973802347832 ) ) ;
#15829 = AXIS2_PLACEMENT_3D ( 'NONE', #4197, #10572, #20260 ) ;
#15830 = CARTESIAN_POINT ( 'NONE',  ( 0.5400860642111662280, -1.363031247223201126, 0.7740706644004844428 ) ) ;
#15832 = ORIENTED_EDGE ( 'NONE', *, *, #34609, .F. ) ;
#15831 = CARTESIAN_POINT ( 'NONE',  ( 0.01027559747412087367, -0.5340578617728122257, 0.1070821439362245192 ) ) ;
#15833 = ORIENTED_EDGE ( 'NONE', *, *, #29326, .F. ) ;
#15834 = CARTESIAN_POINT ( 'NONE',  ( 0.2031772314465054019, -0.6986852483529358837, 0.3457875108286008192 ) ) ;
#15835 = ORIENTED_EDGE ( 'NONE', *, *, #23255, .T. ) ;
#15836 = CARTESIAN_POINT ( 'NONE',  ( 0.2061925047406416300, -1.267151160079532435, 0.9188585589093583028 ) ) ;
#15838 = CARTESIAN_POINT ( 'NONE',  ( -0.01895494625228095684, -0.4667936258712473419, 0.2292799240428166629 ) ) ;
#15837 = CARTESIAN_POINT ( 'NONE',  ( 0.1378772255622009446, -0.8829796579180423377, 0.5385982703296793295 ) ) ;
#15839 = DIRECTION ( 'NONE',  ( 1.000000000000000000, -0.000000000000000000, -0.000000000000000000 ) ) ;
#15840 = CARTESIAN_POINT ( 'NONE',  ( 0.01220508677664999299, -0.4284039737085656996, 0.1457185332388702959 ) ) ;
#15841 = COORDINATED_UNIVERSAL_TIME_OFFSET ( 0, 0, .AHEAD. ) ;
#15842 = CARTESIAN_POINT ( 'NONE',  ( -2.112273405726188513E-14, -2.097675824466503691, -0.7286991843995640483 ) ) ;
#15844 = ORIENTED_EDGE ( 'NONE', *, *, #35685, .T. ) ;
#15843 = VERTEX_POINT ( 'NONE', #6861 ) ;
#15845 = CARTESIAN_POINT ( 'NONE',  ( 0.3839874728425691219, -1.826195879522261700, -0.4830234552410120896 ) ) ;
#15846 = CARTESIAN_POINT ( 'NONE',  ( 0.3921301437161267556, -1.752887964102751051, -0.4509272787481405365 ) ) ;
#15847 = CARTESIAN_POINT ( 'NONE',  ( -0.03478556507499973999, -0.4639967941986908873, 0.2267627654641752033 ) ) ;
#15848 = DIRECTION ( 'NONE',  ( 1.000000000000000000, -2.325617669281430431E-12, -1.136734431350444160E-12 ) ) ;
#15849 = CYLINDRICAL_SURFACE ( 'NONE', #2787, 0.2200000000000000566 ) ;
#15850 = CARTESIAN_POINT ( 'NONE',  ( 0.5185821078323552547, -1.679889620551088258, -0.4521106403869140644 ) ) ;
#15851 = ADVANCED_FACE ( 'NONE', ( #19438 ), #4067, .F. ) ;
#15852 = CARTESIAN_POINT ( 'NONE',  ( 0.03043063305005027849, -0.5845788966253381291, 0.5517386709610753170 ) ) ;
#15853 = CIRCLE ( 'NONE', #21118, 0.1000000000000000194 ) ;
#15854 = APPLICATION_CONTEXT ( 'configuration controlled 3d designs of mechanical parts and assemblies' ) ;
#15855 = CARTESIAN_POINT ( 'NONE',  ( 0.3817504269947160078, -1.726033828776056378, 0.4251703030630522018 ) ) ;
#15856 = CIRCLE ( 'NONE', #20466, 0.1600000000000016964 ) ;
#15857 = DIRECTION ( 'NONE',  ( 5.879757087931980518E-34, 0.5877852522924756906, 0.8090169943749455639 ) ) ;
#15858 =( BOUNDED_SURFACE ( )  B_SPLINE_SURFACE ( 3, 2, ( 
 ( #31176, #37138, #2182 ),
 ( #5843, #2992, #24199 ),
 ( #40005, #18211, #30956 ),
 ( #15541, #39816, #24809 ),
 ( #40422, #36723, #18002 ),
 ( #27886, #33627, #8341 ),
 ( #2578, #8531, #20911 ),
 ( #30562, #12250, #36530 ),
 ( #2385, #12043, #37330 ),
 ( #27480, #27674, #11828 ),
 ( #24602, #21706, #28092 ),
 ( #8951, #28692, #28273 ),
 ( #17098, #13800, #28477 ),
 ( #559, #1293, #12631 ),
 ( #35823, #13054, #139 ),
 ( #25415, #25607, #34846 ),
 ( #24988, #3792, #26364 ),
 ( #28883, #25197, #12853 ),
 ( #31379, #6456, #20201 ),
 ( #16154, #32726, #16347 ),
 ( #18836, #9342, #31557 ),
 ( #38898, #4533, #10726 ) ),
 .UNSPECIFIED., .F., .F., .T. ) 
 B_SPLINE_SURFACE_WITH_KNOTS ( ( 4, 2, 2, 2, 2, 2, 2, 2, 2, 2, 4 ),
 ( 3, 3 ),
 ( 0.002013519961495849157, 0.002780892266055832833, 0.003548264570615816075, 0.004315636875175799317, 0.004699323027455791155, 0.005083009179735782992, 0.005466695332015774830, 0.005850381484295766668, 0.006617753788855749476, 0.007385126093415732285, 0.008152498397975715960 ),
 ( 0.000000000000000000, 1.000000000000000000 ),
 .UNSPECIFIED. ) 
 GEOMETRIC_REPRESENTATION_ITEM ( )  RATIONAL_B_SPLINE_SURFACE ( (
 ( 1.000000000000000000, 0.7283825911960482014, 1.000000000000000000),
 ( 1.000000000000000000, 0.7404375345927979302, 1.000000000000000000),
 ( 1.000000000000000000, 0.7521483142434933766, 1.000000000000000000),
 ( 1.000000000000000000, 0.7744460733777726036, 1.000000000000000000),
 ( 1.000000000000000000, 0.7845612039381349989, 1.000000000000000000),
 ( 1.000000000000000000, 0.8022035258263032764, 1.000000000000000000),
 ( 1.000000000000000000, 0.8093965293321971899, 1.000000000000000000),
 ( 1.000000000000000000, 0.8169028692725515128, 1.000000000000000000),
 ( 1.000000000000000000, 0.8188329634864320861, 1.000000000000000000),
 ( 1.000000000000000000, 0.8214004505363229347, 1.000000000000000000),
 ( 1.000000000000000000, 0.8220602406259858164, 1.000000000000000000),
 ( 1.000000000000000000, 0.8220736605436884670, 1.000000000000000000),
 ( 1.000000000000000000, 0.8214126668415180355, 1.000000000000000000),
 ( 1.000000000000000000, 0.8188520474558893536, 1.000000000000000000),
 ( 1.000000000000000000, 0.8169545908335051898, 1.000000000000000000),
 ( 1.000000000000000000, 0.8094771004218379584, 1.000000000000000000),
 ( 1.000000000000000000, 0.8022723753807513569, 1.000000000000000000),
 ( 1.000000000000000000, 0.7845733350637317249, 1.000000000000000000),
 ( 1.000000000000000000, 0.7744472902493032551, 1.000000000000000000),
 ( 1.000000000000000000, 0.7522916829163440733, 1.000000000000000000),
 ( 1.000000000000000000, 0.7403553004665507364, 1.000000000000000000),
 ( 1.000000000000000000, 0.7283825911960212229, 1.000000000000000000) ) ) 
 REPRESENTATION_ITEM ( '' )  SURFACE ( )  );
#15859 = CARTESIAN_POINT ( 'NONE',  ( 0.1626176757286639796, -0.6782218769987641283, 0.05683303076865411224 ) ) ;
#15860 = CARTESIAN_POINT ( 'NONE',  ( 0.3738055494968318682, -1.722068535337600848, -0.4175881411983431435 ) ) ;
#15861 = DIRECTION ( 'NONE',  ( -5.886781462978834834E-17, -0.1581525901458493422, 0.9874146840259967473 ) ) ;
#15862 = VECTOR ( 'NONE', #21038, 39.37007874015748143 ) ;
#15863 = AXIS2_PLACEMENT_3D ( 'NONE', #9288, #3134, #15675 ) ;
#15864 = FACE_OUTER_BOUND ( 'NONE', #2572, .T. ) ;
#15865 = CARTESIAN_POINT ( 'NONE',  ( 0.002083146443013488870, -0.4777046557262296100, 0.1283381445693447254 ) ) ;
#15866 = CARTESIAN_POINT ( 'NONE',  ( 0.1002285206263032746, -1.304924405955540934, 0.7288703187181188037 ) ) ;
#15867 = APPROVAL_DATE_TIME ( #3306, #27757 ) ;
#15868 = CARTESIAN_POINT ( 'NONE',  ( -0.03875523708677544588, 0.4416911308383500434, 0.1785246905291629493 ) ) ;
#15869 = B_SPLINE_CURVE_WITH_KNOTS ( 'NONE', 3,
 ( #37198, #11, #31432, #18894, #21769, #2639, #9018, #12697, #21161, #21579, #30622, #34101, #14985, #34302, #33691, #12493, #5505, #5718 ),
 .UNSPECIFIED., .F., .F.,
 ( 4, 2, 2, 2, 2, 2, 2, 2, 4 ),
 ( 0.000000000000000000, 0.0007429904698459527390, 0.001485980939691905478, 0.002228971409537858217, 0.002971961879383810956, 0.003714952349229763695, 0.004457942819075716434, 0.005200933288921669173, 0.005943923758767621912 ),
 .UNSPECIFIED. ) ;
#15870 = AXIS2_PLACEMENT_3D ( 'NONE', #11651, #14732, #18013 ) ;
#15871 = CARTESIAN_POINT ( 'NONE',  ( 0.7025991982850786632, -1.521397541714836210, 0.5686247791543105334 ) ) ;
#15872 = VERTEX_POINT ( 'NONE', #10372 ) ;
#15873 = CARTESIAN_POINT ( 'NONE',  ( 0.1850410792631035362, -0.8547936666690981733, 0.1477569985384108442 ) ) ;
#15874 = ORIENTED_EDGE ( 'NONE', *, *, #8718, .T. ) ;
#15875 = LINE ( 'NONE', #32861, #36196 ) ;
#15876 = CARTESIAN_POINT ( 'NONE',  ( 0.2746276767615154490, -1.658875007953147573, 0.7201787504598219369 ) ) ;
#15877 = CIRCLE ( 'NONE', #4698, 0.01499999999999995087 ) ;
#15878 = CARTESIAN_POINT ( 'NONE',  ( 0.1317540737835983244, -0.5510263468228310257, 0.1532934214773048198 ) ) ;
#15879 = ADVANCED_FACE ( 'NONE', ( #6650 ), #13459, .T. ) ;
#15881 = EDGE_LOOP ( 'NONE', ( #35929, #7744 ) ) ;
#15880 = CARTESIAN_POINT ( 'NONE',  ( 0.5446207946416926626, -1.171030664636589114, 0.5955391433021992587 ) ) ;
#15883 = ORIENTED_EDGE ( 'NONE', *, *, #34374, .T. ) ;
#15882 = VERTEX_POINT ( 'NONE', #35450 ) ;
#15884 = CARTESIAN_POINT ( 'NONE',  ( 0.6672263256168233791, -1.559577713309469038, 0.6159734170043378310 ) ) ;
#15885 = EDGE_LOOP ( 'NONE', ( #11682, #531, #13261, #40019, #360, #39171 ) ) ;
#15886 = VECTOR ( 'NONE', #7192, 39.37007874015748854 ) ;
#15887 = DIRECTION ( 'NONE',  ( 1.000000000000000000, -0.000000000000000000, -0.000000000000000000 ) ) ;
#15888 = CARTESIAN_POINT ( 'NONE',  ( 0.03113248654051816583, -0.2793841226333812489, -0.1799682156082512696 ) ) ;
#15889 = COORDINATED_UNIVERSAL_TIME_OFFSET ( 0, 0, .AHEAD. ) ;
#15890 = AXIS2_PLACEMENT_3D ( 'NONE', #7096, #23176, #5176 ) ;
#15891 = FACE_OUTER_BOUND ( 'NONE', #25138, .T. ) ;
#15892 = ORIENTED_EDGE ( 'NONE', *, *, #20852, .F. ) ;
#15893 = CARTESIAN_POINT ( 'NONE',  ( 0.1135430571860531063, -0.7812966806583707680, 0.4098588298052969758 ) ) ;
#15894 = CARTESIAN_POINT ( 'NONE',  ( 0.3758474042836421614, -1.611613784703100016, -0.3604881591361508431 ) ) ;
#15895 = CARTESIAN_POINT ( 'NONE',  ( 0.5249336263842677708, -1.526781716017400647, 0.5684230341163545308 ) ) ;
#15896 = DIRECTION ( 'NONE',  ( -1.000000000000000000, -0.000000000000000000, -0.000000000000000000 ) ) ;
#15897 = CARTESIAN_POINT ( 'NONE',  ( -0.1668451997768058692, 0.4851271022253518805, 0.1251051315678443909 ) ) ;
#15898 = VERTEX_POINT ( 'NONE', #22323 ) ;
#15899 = DIRECTION ( 'NONE',  ( 0.4999551463232376758, -0.8660512985181131329, 0.000000000000000000 ) ) ;
#15900 = CARTESIAN_POINT ( 'NONE',  ( 0.6520986873597004463, -1.511863584991765208, 0.7630484353180611024 ) ) ;
#15901 = CARTESIAN_POINT ( 'NONE',  ( 0.6409058204046232943, -1.459016202299332710, -0.5155029497116575543 ) ) ;
#15902 = CARTESIAN_POINT ( 'NONE',  ( 0.6098080674161761028, -1.478513402567430912, 0.5979631250306651769 ) ) ;
#15903 = CARTESIAN_POINT ( 'NONE',  ( -0.2746410161513776482, -3.849534981189179028, -0.2910928155360645864 ) ) ;
#15904 = AXIS2_PLACEMENT_3D ( 'NONE', #3109, #18330, #12364 ) ;
#15905 = CARTESIAN_POINT ( 'NONE',  ( -0.3000000000000000999, -2.599675038826658735, -0.8213992999509311943 ) ) ;
#15906 = CARTESIAN_POINT ( 'NONE',  ( 0.01895884884825074432, -0.5124024296374576348, -0.08888335629180295350 ) ) ;
#15907 = DIRECTION ( 'NONE',  ( -0.4999999999999988898, -0.6123724356957954695, 0.6123724356957944703 ) ) ;
#15908 = CARTESIAN_POINT ( 'NONE',  ( 0.5132401252193277141, -1.118795806750195077, 0.5530176081283582068 ) ) ;
#15909 = APPLICATION_PROTOCOL_DEFINITION ( 'international standard', 'automotive_design', 2000, #27157 ) ;
#15910 = CIRCLE ( 'NONE', #24465, 0.1400000000000007350 ) ;
#15911 = AXIS2_PLACEMENT_3D ( 'NONE', #11517, #33496, #21177 ) ;
#15912 = CARTESIAN_POINT ( 'NONE',  ( -0.1743922129835729085, -0.5166151207188712791, 0.3750000000000001110 ) ) ;
#15913 = AXIS2_PLACEMENT_3D ( 'NONE', #33848, #30754, #3370 ) ;
#15914 = LINE ( 'NONE', #12024, #39229 ) ;
#15915 = CARTESIAN_POINT ( 'NONE',  ( -0.02881329448201254764, 0.06013561456248567999, 0.4945523155237982471 ) ) ;
#15916 = VERTEX_POINT ( 'NONE', #34839 ) ;
#15917 = CARTESIAN_POINT ( 'NONE',  ( 0.2160079821674734668, -1.358042438312749622, -0.3319550444996756111 ) ) ;
#15918 = CARTESIAN_POINT ( 'NONE',  ( -0.01896968469603269383, -0.2428673116372725704, 0.4598334287537050868 ) ) ;
#15919 = CARTESIAN_POINT ( 'NONE',  ( 0.1850825143922525950, -0.8517056288164835953, 0.1806043688250910384 ) ) ;
#15920 = ORIENTED_EDGE ( 'NONE', *, *, #35867, .T. ) ;
#15921 = CARTESIAN_POINT ( 'NONE',  ( 0.3206535937437295369, -1.182295409031864697, 0.3157417262808777658 ) ) ;
#15922 = CARTESIAN_POINT ( 'NONE',  ( 0.01814112910464814668, -1.016494997226478070, 0.7024430388243299017 ) ) ;
#15924 = ORIENTED_EDGE ( 'NONE', *, *, #38545, .F. ) ;
#15923 = ORIENTED_EDGE ( 'NONE', *, *, #25352, .T. ) ;
#15925 = ADVANCED_FACE ( 'NONE', ( #739 ), #7251, .T. ) ;
#15926 = CARTESIAN_POINT ( 'NONE',  ( 0.6929208297549553919, -1.429122597532291650, 0.5682417262808779901 ) ) ;
#15927 = VERTEX_POINT ( 'NONE', #1148 ) ;
#15928 = CARTESIAN_POINT ( 'NONE',  ( 0.2247055958334348014, -1.611582774488795611, -0.3560079958479117623 ) ) ;
#15929 = ADVANCED_FACE ( 'NONE', ( #13648 ), #25771, .T. ) ;
#15931 = CARTESIAN_POINT ( 'NONE',  ( -0.2746410161513770931, -2.599675038826658735, -0.8213992999509311943 ) ) ;
#15930 = CARTESIAN_POINT ( 'NONE',  ( -0.2399999999999999079, -4.394818335734379744, -0.8816972205720928768 ) ) ;
#15932 = CARTESIAN_POINT ( 'NONE',  ( 0.03875673594170320896, -0.2524061059367321280, -0.4040421724581200191 ) ) ;
#15933 = EDGE_LOOP ( 'NONE', ( #21993, #28154, #28687, #9087 ) ) ;
#15934 = CARTESIAN_POINT ( 'NONE',  ( -0.01895884884825283639, 0.3622979475331356003, -0.3730907371368774039 ) ) ;
#15935 = EDGE_CURVE ( 'NONE', #8017, #32089, #16562, .T. ) ;
#15936 = ORIENTED_EDGE ( 'NONE', *, *, #28124, .F. ) ;
#15937 = ORIENTED_EDGE ( 'NONE', *, *, #27646, .T. ) ;
#15938 = CARTESIAN_POINT ( 'NONE',  ( 0.08990515874724799850, -0.5631160408504091164, 0.1543070364275382633 ) ) ;
#15939 = EDGE_LOOP ( 'NONE', ( #35964, #37422, #11788, #9765, #5423, #7931, #32114 ) ) ;
#15940 = ORIENTED_EDGE ( 'NONE', *, *, #15310, .F. ) ;
#15941 = CIRCLE ( 'NONE', #27141, 0.1249999999999999584 ) ;
#15942 = DIRECTION ( 'NONE',  ( -1.000000000000000000, -0.000000000000000000, -0.000000000000000000 ) ) ;
#15943 = AXIS2_PLACEMENT_3D ( 'NONE', #32852, #4655, #635 ) ;
#15944 = CARTESIAN_POINT ( 'NONE',  ( 0.2282559409138358864, -1.032523682450960267, 0.8073022102877677186 ) ) ;
#15946 = DIRECTION ( 'NONE',  ( 8.881784197001246407E-16, -2.361472542561082612E-16, 1.000000000000000000 ) ) ;
#15945 = CARTESIAN_POINT ( 'NONE',  ( 0.4445735045382223638, -1.592385390845466375, -0.4212583484125541622 ) ) ;
#15947 = DIRECTION ( 'NONE',  ( 0.000000000000000000, -0.3882559824134205195, 0.9215515678030119506 ) ) ;
#15948 = CARTESIAN_POINT ( 'NONE',  ( 0.2487277522598718149, -0.9673568096827294127, 0.5239956023218622638 ) ) ;
#15949 = CIRCLE ( 'NONE', #6742, 0.01500000000000004281 ) ;
#15950 = CARTESIAN_POINT ( 'NONE',  ( -0.2746410161513770931, -3.525450504378606187, -0.1357627943591874498 ) ) ;
#15951 = CARTESIAN_POINT ( 'NONE',  ( 0.1897189402164200511, -0.5341521847524689504, 0.1523768035615612193 ) ) ;
#15952 = CARTESIAN_POINT ( 'NONE',  ( 0.1298170261405827419, -0.5953669216844625911, 0.3065043694650786965 ) ) ;
#15953 = CARTESIAN_POINT ( 'NONE',  ( -0.04139678531769484110, 0.2901741387554239715, -0.3704845587920863048 ) ) ;
#15954 = TOROIDAL_SURFACE ( 'NONE', #38934, 0.05330708661417342398, 0.01000000000000000021 ) ;
#15955 = ADVANCED_FACE ( 'NONE', ( #4391 ), #21641, .T. ) ;
#15956 = FACE_OUTER_BOUND ( 'NONE', #35545, .T. ) ;
#15957 = APPROVAL ( #33107, 'UNSPECIFIED' ) ;
#15958 = CARTESIAN_POINT ( 'NONE',  ( 0.1784968570797965948, -1.218054820023663831, -0.5155029497116575543 ) ) ;
#15959 = CARTESIAN_POINT ( 'NONE',  ( 0.3005352500653590830, -1.024020065930653756, 0.7747702324826710729 ) ) ;
#15960 = CARTESIAN_POINT ( 'NONE',  ( 0.000000000000000000, -0.4700000000000001954, 0.000000000000000000 ) ) ;
#15961 = CARTESIAN_POINT ( 'NONE',  ( 0.2413003582545148740, -0.7023676887333554220, 0.5126316699731913173 ) ) ;
#15962 = CARTESIAN_POINT ( 'NONE',  ( 0.4824008369422878584, -1.130704479788579464, 0.4427808555068210583 ) ) ;
#15963 = CARTESIAN_POINT ( 'NONE',  ( 0.02842665824954763304, -1.107459934983165972, 0.6590139982913070238 ) ) ;
#15964 = VECTOR ( 'NONE', #35342, 39.37007874015748854 ) ;
#15965 = CARTESIAN_POINT ( 'NONE',  ( 0.6231091328894153847, -1.554071593431288756, -0.4320382102285837966 ) ) ;
#15966 = DIRECTION ( 'NONE',  ( -0.000000000000000000, 0.9246857012436749956, -0.3807313408632033713 ) ) ;
#15967 = DIRECTION ( 'NONE',  ( -0.4999551463232377313, 0.8660512985181132439, -0.000000000000000000 ) ) ;
#15968 = DIRECTION ( 'NONE',  ( -0.000000000000000000, 0.8438867430782084345, 0.5365213554527479278 ) ) ;
#15969 = EDGE_CURVE ( 'NONE', #16305, #23498, #1958, .T. ) ;
#15970 = CARTESIAN_POINT ( 'NONE',  ( 0.6111956757316053812, -1.601608420676993827, 0.4350745821225746046 ) ) ;
#15971 = VECTOR ( 'NONE', #12126, 39.37007874015748854 ) ;
#15972 = VECTOR ( 'NONE', #8012, 39.37007874015748143 ) ;
#15973 = ORIENTED_EDGE ( 'NONE', *, *, #37674, .F. ) ;
#15974 = CARTESIAN_POINT ( 'NONE',  ( 0.3632570605522777996, -1.760200006483175095, -0.5108946128509906925 ) ) ;
#15975 = CARTESIAN_POINT ( 'NONE',  ( 0.3470843243164753456, -1.069660623632250784, 0.7669445845107666360 ) ) ;
#15976 = VECTOR ( 'NONE', #26160, 39.37007874015748143 ) ;
#15977 = CARTESIAN_POINT ( 'NONE',  ( 0.6555154469717897614, -1.476457112295515905, 0.4182417262808776903 ) ) ;
#15978 = CARTESIAN_POINT ( 'NONE',  ( -0.2399999999999999079, -1.804235510932644004, -0.1501860188971498311 ) ) ;
#15979 = CARTESIAN_POINT ( 'NONE',  ( 0.3607791945725288829, -1.125243654965698337, 0.6038723418466845905 ) ) ;
#15980 = CIRCLE ( 'NONE', #35773, 0.07999999999999996003 ) ;
#15981 = ORIENTED_EDGE ( 'NONE', *, *, #24647, .F. ) ;
#15982 = EDGE_CURVE ( 'NONE', #16583, #31364, #32994, .T. ) ;
#15983 = CARTESIAN_POINT ( 'NONE',  ( 0.4186432780919984720, -1.612034538517055360, -0.6668481824684697745 ) ) ;
#15984 = AXIS2_PLACEMENT_3D ( 'NONE', #30532, #18588, #21679 ) ;
#15985 = CARTESIAN_POINT ( 'NONE',  ( -0.3000000000000000999, -2.809880844172510272, -0.2480969101616946337 ) ) ;
#15986 = CARTESIAN_POINT ( 'NONE',  ( 0.4880443886438106116, -1.659886120534822096, 0.5165855446388504246 ) ) ;
#15987 = CARTESIAN_POINT ( 'NONE',  ( 0.03672447062657326761, 0.2485879206383745099, -0.4115698867982595099 ) ) ;
#15988 = EDGE_CURVE ( 'NONE', #32917, #23555, #24757, .T. ) ;
#15989 = CARTESIAN_POINT ( 'NONE',  ( 0.4978345755714322918, -1.288570401096832407, 0.6247038493719151431 ) ) ;
#15990 = CARTESIAN_POINT ( 'NONE',  ( 0.3183458363839229421, -1.763251125072305969, 0.5158787115206079354 ) ) ;
#15991 = CARTESIAN_POINT ( 'NONE',  ( 0.4241296934850513067, -1.044958113096912777, 0.6349482895397999815 ) ) ;
#15992 = EDGE_LOOP ( 'NONE', ( #30727, #18473, #142, #23857, #1590, #17049 ) ) ;
#15993 = APPROVAL_DATE_TIME ( #25465, #19454 ) ;
#15994 = EDGE_CURVE ( 'NONE', #34957, #23581, #22510, .T. ) ;
#15995 = CARTESIAN_POINT ( 'NONE',  ( -0.002130502458654864786, -0.8570779732651497840, 0.2369880927919252311 ) ) ;
#15996 = ORIENTED_EDGE ( 'NONE', *, *, #687, .T. ) ;
#15997 = CARTESIAN_POINT ( 'NONE',  ( 0.3871526695961494124, -1.595276482059940548, 0.6939178973677117002 ) ) ;
#15999 = CARTESIAN_POINT ( 'NONE',  ( 0.1744619341259203982, -0.9164761487563395370, 0.1198935801002234819 ) ) ;
#15998 = CARTESIAN_POINT ( 'NONE',  ( 0.08661364503105330181, -0.7606219696568068400, 0.02128811888083972578 ) ) ;
#16000 = CARTESIAN_POINT ( 'NONE',  ( 0.06923712653936904549, -0.5400029222721455247, 0.1457185332388703236 ) ) ;
#16001 = ORIENTED_EDGE ( 'NONE', *, *, #14200, .T. ) ;
#16002 = VECTOR ( 'NONE', #1780, 39.37007874015748143 ) ;
#16003 = ORIENTED_EDGE ( 'NONE', *, *, #12737, .T. ) ;
#16004 = B_SPLINE_CURVE_WITH_KNOTS ( 'NONE', 3,
 ( #3211, #21957, #22171, #5876 ),
 .UNSPECIFIED., .F., .F.,
 ( 4, 4 ),
 ( 0.007879993664335074866, 0.008137213426454060344 ),
 .UNSPECIFIED. ) ;
#16005 = EDGE_LOOP ( 'NONE', ( #2717, #14409, #19677, #22844 ) ) ;
#16006 = CARTESIAN_POINT ( 'NONE',  ( 0.3244236418308351078, -1.295451955201979866, 0.5689238818033025558 ) ) ;
#16007 = CARTESIAN_POINT ( 'NONE',  ( 0.3203573007257789484, -1.073668807559134519, 0.7999796645404516626 ) ) ;
#16008 = VERTEX_POINT ( 'NONE', #35003 ) ;
#16009 = CARTESIAN_POINT ( 'NONE',  ( 0.4738546087217606062, -1.652018268363231845, -0.3975985852014427002 ) ) ;
#16010 = CARTESIAN_POINT ( 'NONE',  ( 0.06504549419198706051, -1.972538361174909882, -0.3281045264835606989 ) ) ;
#16011 = LINE ( 'NONE', #12928, #22449 ) ;
#16012 = VECTOR ( 'NONE', #38826, 39.37007874015748854 ) ;
#16013 = VECTOR ( 'NONE', #10273, 39.37007874015748143 ) ;
#16014 = EDGE_CURVE ( 'NONE', #39656, #26889, #15267, .T. ) ;
#16015 = DIRECTION ( 'NONE',  ( 0.000000000000000000, 0.000000000000000000, 1.000000000000000000 ) ) ;
#16016 = DIRECTION ( 'NONE',  ( 7.771561172376107616E-16, -7.170354002788761615E-17, 1.000000000000000000 ) ) ;
#16017 = CARTESIAN_POINT ( 'NONE',  ( -0.02000000000000000042, -1.968175500587574067, -0.6048844944454191408 ) ) ;
#16018 = LINE ( 'NONE', #31852, #35849 ) ;
#16019 = CIRCLE ( 'NONE', #28485, 0.009999999999999996739 ) ;
#16020 = CARTESIAN_POINT ( 'NONE',  ( 0.1999999999999789724, -2.097675824466503691, -0.5196396315034578217 ) ) ;
#16021 = CARTESIAN_POINT ( 'NONE',  ( 0.5264113014007820723, -1.640729993778254014, 0.5682417262808777680 ) ) ;
#16022 = CARTESIAN_POINT ( 'NONE',  ( 0.1698555401406868226, -1.244443917810318823, 0.6163427178748981383 ) ) ;
#16023 = CIRCLE ( 'NONE', #26538, 0.2200000000000000566 ) ;
#16024 = CARTESIAN_POINT ( 'NONE',  ( 0.1581139529352034445, -1.989394613953671342, -0.6673518793402363203 ) ) ;
#16025 = FACE_OUTER_BOUND ( 'NONE', #24803, .T. ) ;
#16026 = PERSON_AND_ORGANIZATION ( #28500, #32463 ) ;
#16027 = CARTESIAN_POINT ( 'NONE',  ( 0.1875000000000002498, -0.9151275355372966436, 0.1457185332388701016 ) ) ;
#16028 = CARTESIAN_POINT ( 'NONE',  ( 0.3164589185008098160, -1.173239401124993364, 0.4880957576780184937 ) ) ;
#16029 = CARTESIAN_POINT ( 'NONE',  ( 0.4509257687968690753, -1.222389892490845620, 0.5856983068965044836 ) ) ;
#16030 = FACE_OUTER_BOUND ( 'NONE', #10290, .T. ) ;
#16031 = CARTESIAN_POINT ( 'NONE',  ( 0.1849096901904442591, -1.549205955729530793, 0.5682417262808778791 ) ) ;
#16032 = CARTESIAN_POINT ( 'NONE',  ( -0.0003565257878083244957, -0.9235813610340595226, 0.06569692014612905917 ) ) ;
#16033 = AXIS2_PLACEMENT_3D ( 'NONE', #17192, #11220, #1795 ) ;
#16034 = CARTESIAN_POINT ( 'NONE',  ( 0.1399999999999994582, 0.000000000000000000, 0.000000000000000000 ) ) ;
#16035 = FACE_OUTER_BOUND ( 'NONE', #17144, .T. ) ;
#16036 = ORIENTED_EDGE ( 'NONE', *, *, #18787, .F. ) ;
#16037 = AXIS2_PLACEMENT_3D ( 'NONE', #39588, #16989, #35914 ) ;
#16038 = ORIENTED_EDGE ( 'NONE', *, *, #38413, .T. ) ;
#16039 = EDGE_CURVE ( 'NONE', #17786, #1840, #37572, .T. ) ;
#16040 = AXIS2_PLACEMENT_3D ( 'NONE', #24961, #718, #6428 ) ;
#16041 = CARTESIAN_POINT ( 'NONE',  ( 0.05999999999999990757, -0.0007915077497714572644, 0.0008899645335182150997 ) ) ;
#16042 = ORIENTED_EDGE ( 'NONE', *, *, #40303, .T. ) ;
#16043 = LINE ( 'NONE', #38038, #21087 ) ;
#16044 = FACE_OUTER_BOUND ( 'NONE', #35723, .T. ) ;
#16045 = EDGE_CURVE ( 'NONE', #20255, #25087, #2151, .T. ) ;
#16046 = CARTESIAN_POINT ( 'NONE',  ( 0.4914727279001435689, -1.286330727027781728, 0.8049515525046259112 ) ) ;
#16048 = EDGE_LOOP ( 'NONE', ( #23844, #21915 ) ) ;
#16047 = LINE ( 'NONE', #32257, #40340 ) ;
#16049 = VECTOR ( 'NONE', #9772, 39.37007874015748143 ) ;
#16050 = ORIENTED_EDGE ( 'NONE', *, *, #29559, .T. ) ;
#16051 = DIRECTION ( 'NONE',  ( -0.9780874495037195082, 0.000000000000000000, 0.2081944790894049990 ) ) ;
#16052 = VERTEX_POINT ( 'NONE', #6813 ) ;
#16053 = VECTOR ( 'NONE', #26545, 39.37007874015748143 ) ;
#16054 = CARTESIAN_POINT ( 'NONE',  ( 0.2979046102063983015, -1.656890573677640921, 0.5828864586326335528 ) ) ;
#16055 = CARTESIAN_POINT ( 'NONE',  ( 0.6396152150128876501, -1.561615300510546200, 0.4193375745894342144 ) ) ;
#16056 = CARTESIAN_POINT ( 'NONE',  ( 0.03113248654051816583, 0.1919340784543128453, -0.1767348310837237868 ) ) ;
#16057 = EDGE_CURVE ( 'NONE', #6598, #37905, #37608, .T. ) ;
#16058 = CARTESIAN_POINT ( 'NONE',  ( 0.1877036592482687616, -0.9196856789278203825, 0.1015045423513593059 ) ) ;
#16059 = CARTESIAN_POINT ( 'NONE',  ( 0.4191100986680896257, -1.701672718972387477, 0.4233639548768124428 ) ) ;
#16061 = ORIENTED_EDGE ( 'NONE', *, *, #5769, .T. ) ;
#16060 = ORIENTED_EDGE ( 'NONE', *, *, #10337, .F. ) ;
#16062 = CARTESIAN_POINT ( 'NONE',  ( 0.4159916692016358830, -1.069406866067976081, -0.5155029497116575543 ) ) ;
#16063 = CARTESIAN_POINT ( 'NONE',  ( 0.1862143093560912621, -0.9153542374866666664, 0.1462684119608146649 ) ) ;
#16064 = CARTESIAN_POINT ( 'NONE',  ( -0.03647137243075361523, -0.4543612417835832251, 0.2356044583002005754 ) ) ;
#16065 = CARTESIAN_POINT ( 'NONE',  ( -0.01548846960707524721, 0.2306506793134049660, -0.4716198300880325434 ) ) ;
#16066 = CARTESIAN_POINT ( 'NONE',  ( 0.1773078868329161784, -0.8723994076705423595, 0.5291939128694373995 ) ) ;
#16067 = CARTESIAN_POINT ( 'NONE',  ( -0.2399999999999999079, -2.292669950144801572, -0.8383185228372386222 ) ) ;
#16068 = EDGE_CURVE ( 'NONE', #17175, #26250, #8275, .T. ) ;
#16069 = VECTOR ( 'NONE', #30908, 39.37007874015748143 ) ;
#16070 = APPROVAL ( #13407, 'UNKNOWN' ) ;
#16071 = CARTESIAN_POINT ( 'NONE',  ( 0.4870128057575630054, -1.169653738304198054, 0.4224702079871185401 ) ) ;
#16072 = EDGE_CURVE ( 'NONE', #17308, #9809, #31721, .T. ) ;
#16073 = AXIS2_PLACEMENT_3D ( 'NONE', #2848, #8595, #36992 ) ;
#16074 = CIRCLE ( 'NONE', #3572, 0.2149999999999999967 ) ;
#16075 = FACE_OUTER_BOUND ( 'NONE', #33847, .T. ) ;
#16076 = CARTESIAN_POINT ( 'NONE',  ( -0.01548846960707524721, 0.2306506793134049660, -0.4716198300880325434 ) ) ;
#16077 = CIRCLE ( 'NONE', #4850, 0.1033070866141734129 ) ;
#16078 = CARTESIAN_POINT ( 'NONE',  ( 0.1854100492481942641, -0.7689184785536463673, 0.1457185332388699350 ) ) ;
#16079 = CARTESIAN_POINT ( 'NONE',  ( 0.3888255243409498019, -1.692620460247742598, -0.4086109642453172874 ) ) ;
#16080 = DIRECTION ( 'NONE',  ( 0.4999551463232373982, -0.8660512985181132439, -8.944667923005411581E-18 ) ) ;
#16081 = APPROVAL_PERSON_ORGANIZATION ( #11577, #22255, #24139 ) ;
#16082 = CARTESIAN_POINT ( 'NONE',  ( -0.05464101615137768181, -1.699711333021935777, -0.9366211149475224262 ) ) ;
#16083 = CARTESIAN_POINT ( 'NONE',  ( 0.1499999999999994948, 0.3772621329472714558, 0.3651003739303416706 ) ) ;
#16084 = CIRCLE ( 'NONE', #39058, 0.01500000000000006016 ) ;
#16085 = CARTESIAN_POINT ( 'NONE',  ( 0.1155264449205179456, -1.390086609329345801, 0.6489119185965581682 ) ) ;
#16086 = PERSON_AND_ORGANIZATION_ROLE ( 'creator' ) ;
#16087 = CIRCLE ( 'NONE', #39064, 0.01499999999999996128 ) ;
#16088 = CARTESIAN_POINT ( 'NONE',  ( -0.02000000000000000042, -2.097192720079996242, -0.6592403319832980113 ) ) ;
#16089 = CARTESIAN_POINT ( 'NONE',  ( -0.01548846960707422199, 0.4730347584886799295, 0.2341461249029806180 ) ) ;
#16090 = B_SPLINE_CURVE_WITH_KNOTS ( 'NONE', 3,
 ( #37260, #15463, #40548, #12368, #19158, #6187, #9268, #3113, #9480, #490, #34980, #21845, #34370, #12989, #22062, #25536, #18755, #31305 ),
 .UNSPECIFIED., .F., .F.,
 ( 4, 2, 2, 2, 2, 2, 2, 2, 4 ),
 ( 0.01935643071104403007, 0.02032766186723907603, 0.02129889302343412200, 0.02227012417962916796, 0.02324135533582421392, 0.02421258649201925989, 0.02518381764821430238, 0.02615504880440934835, 0.02712627996060439431 ),
 .UNSPECIFIED. ) ;
#16091 = CARTESIAN_POINT ( 'NONE',  ( 0.6544078563150221850, -1.544269123161552626, 0.4241055859090109292 ) ) ;
#16092 = CARTESIAN_POINT ( 'NONE',  ( 0.1969360143439681521, -0.5736523733507086220, 0.3127385286629807970 ) ) ;
#16093 = ORIENTED_EDGE ( 'NONE', *, *, #19551, .F. ) ;
#16094 = CARTESIAN_POINT ( 'NONE',  ( -0.1399999999999997358, 0.2149999999999997469, -5.463695987328526437E-16 ) ) ;
#16095 = CARTESIAN_POINT ( 'NONE',  ( 0.2665534027467502676, -1.663858438167157283, 0.7214166325115675127 ) ) ;
#16096 = CIRCLE ( 'NONE', #18047, 0.01500000000000001159 ) ;
#16097 = EDGE_CURVE ( 'NONE', #17902, #36736, #2819, .T. ) ;
#16098 = CARTESIAN_POINT ( 'NONE',  ( 0.4326761725401005454, -1.237000291097626770, 0.8252275854053723325 ) ) ;
#16100 = EDGE_LOOP ( 'NONE', ( #2882, #11181, #8147, #23232, #17416, #3450 ) ) ;
#16099 = DIRECTION ( 'NONE',  ( 0.4999999999999966693, 0.7750948722061129503, -0.3863003223915205675 ) ) ;
#16101 = VECTOR ( 'NONE', #320, 39.37007874015748854 ) ;
#16102 = ADVANCED_FACE ( 'NONE', ( #19394 ), #35413, .F. ) ;
#16104 = ORIENTED_EDGE ( 'NONE', *, *, #4913, .T. ) ;
#16103 = ORIENTED_EDGE ( 'NONE', *, *, #36894, .F. ) ;
#16105 = CARTESIAN_POINT ( 'NONE',  ( 0.03113248654051816583, 0.2463462108298974940, -0.03520871226632921180 ) ) ;
#16106 = CIRCLE ( 'NONE', #21337, 0.2500000000000000000 ) ;
#16107 = VERTEX_POINT ( 'NONE', #29034 ) ;
#16108 = VECTOR ( 'NONE', #38048, 39.37007874015748854 ) ;
#16109 = APPLIED_SECURITY_CLASSIFICATION_ASSIGNMENT ( #33833, ( #10846 ) ) ;
#16110 = CARTESIAN_POINT ( 'NONE',  ( 0.6272581727275550190, -1.617152969708947063, -0.5103538732883908802 ) ) ;
#16111 = PERSON_AND_ORGANIZATION_ROLE ( 'classification_officer' ) ;
#16112 = CARTESIAN_POINT ( 'NONE',  ( 0.2614565024141662919, -0.7584087153545726601, 0.1023043458361303226 ) ) ;
#16113 = VERTEX_POINT ( 'NONE', #16105 ) ;
#16114 = CARTESIAN_POINT ( 'NONE',  ( 0.1896256107075826869, -0.8716025430740738100, 0.6086388917311702507 ) ) ;
#16115 = VECTOR ( 'NONE', #7994, 39.37007874015748143 ) ;
#16116 = CARTESIAN_POINT ( 'NONE',  ( 0.08990936761269915922, -0.5436479961250830772, 0.1370866209488758314 ) ) ;
#16117 =( BOUNDED_SURFACE ( )  B_SPLINE_SURFACE ( 3, 2, ( 
 ( #16089, #3526, #31497 ),
 ( #13176, #6397, #18765 ),
 ( #28213, #31315, #21855 ),
 ( #3124, #31705, #19380 ),
 ( #9492, #6584, #12573 ),
 ( #25348, #28630, #22070 ),
 ( #15868, #15664, #28827 ),
 ( #80, #3736, #25133 ),
 ( #34594, #289, #19166 ),
 ( #685, #28417, #18965 ),
 ( #9699, #31914, #25746 ),
 ( #502, #38272, #12788 ),
 ( #37887, #10104, #22266 ),
 ( #16476, #12998, #25545 ),
 ( #34989, #38073, #9892 ),
 ( #22677, #35209, #7011 ),
 ( #19578, #32111, #3918 ),
 ( #29017, #884, #24932 ) ),
 .UNSPECIFIED., .F., .F., .F. ) 
 B_SPLINE_SURFACE_WITH_KNOTS ( ( 4, 2, 2, 2, 2, 2, 2, 2, 4 ),
 ( 3, 3 ),
 ( -0.001532620576208785709, -0.0007637936630078138219, 5.033250193158065461E-06, 0.0007738601633941299528, 0.001542687076595101840, 0.002311513989796073511, 0.003080340902997045615, 0.003849167816198017719, 0.004617994729398989390 ),
 ( 0.000000000000000000, 1.000000000000000000 ),
 .UNSPECIFIED. ) 
 GEOMETRIC_REPRESENTATION_ITEM ( )  RATIONAL_B_SPLINE_SURFACE ( (
 ( 1.000000000000000000, 0.7283825911960394306, 1.000000000000000000),
 ( 1.000000000000000000, 0.7404385082111522021, 1.000000000000000000),
 ( 1.000000000000000000, 0.7521504257741571386, 1.000000000000000000),
 ( 1.000000000000000000, 0.7744497410758119926, 1.000000000000000000),
 ( 1.000000000000000000, 0.7845654757376191446, 1.000000000000000000),
 ( 1.000000000000000000, 0.8022083990889726790, 1.000000000000000000),
 ( 1.000000000000000000, 0.8094167424698524016, 1.000000000000000000),
 ( 1.000000000000000000, 0.8194491993617223358, 1.000000000000000000),
 ( 1.000000000000000000, 0.8220634900779297816, 1.000000000000000000),
 ( 1.000000000000000000, 0.8220705070824532168, 1.000000000000000000),
 ( 1.000000000000000000, 0.8194468812479978048, 1.000000000000000000),
 ( 1.000000000000000000, 0.8094220769840463348, 1.000000000000000000),
 ( 1.000000000000000000, 0.8022659121985385999, 1.000000000000000000),
 ( 1.000000000000000000, 0.7845681159035809982, 1.000000000000000000),
 ( 1.000000000000000000, 0.7744426415185043933, 1.000000000000000000),
 ( 1.000000000000000000, 0.7522890290929258317, 1.000000000000000000),
 ( 1.000000000000000000, 0.7403540167215301171, 1.000000000000000000),
 ( 1.000000000000000000, 0.7283825911960428723, 1.000000000000000000) ) ) 
 REPRESENTATION_ITEM ( '' )  SURFACE ( )  );
#16118 = CARTESIAN_POINT ( 'NONE',  ( 0.1184657642459996246, -0.6327582549063645034, 0.3942365859262391692 ) ) ;
#16119 = CARTESIAN_POINT ( 'NONE',  ( 0.5918007220238434840, -1.591304679919291809, -0.5951766354897257694 ) ) ;
#16120 = CARTESIAN_POINT ( 'NONE',  ( -0.1508021419688995723, 0.4665171419162755795, 0.1089215716836984676 ) ) ;
#16121 = ORIENTED_EDGE ( 'NONE', *, *, #24094, .T. ) ;
#16122 = CARTESIAN_POINT ( 'NONE',  ( 0.4034423500592668188, -1.711423766529257762, 0.6205252146552449055 ) ) ;
#16123 = CARTESIAN_POINT ( 'NONE',  ( 0.6671799058731299192, -1.556892339446394269, 0.6418398848070931972 ) ) ;
#16124 = VERTEX_POINT ( 'NONE', #28646 ) ;
#16125 = CARTESIAN_POINT ( 'NONE',  ( 0.4412967101137347248, -1.641228763480250485, -0.6201386750407782422 ) ) ;
#16126 = CARTESIAN_POINT ( 'NONE',  ( 0.1356025888936704948, -0.5758974039257369615, 0.2504448515252820084 ) ) ;
#16127 = DIRECTION ( 'NONE',  ( 0.8660512985181135770, 0.4999551463232370097, 0.000000000000000000 ) ) ;
#16128 = AXIS2_PLACEMENT_3D ( 'NONE', #40214, #31385, #8746 ) ;
#16129 = EDGE_CURVE ( 'NONE', #12691, #6348, #19247, .T. ) ;
#16130 = CARTESIAN_POINT ( 'NONE',  ( -0.2746410161513779258, -3.527715956914472706, -0.3920205355121876289 ) ) ;
#16131 = AXIS2_PLACEMENT_3D ( 'NONE', #36234, #30259, #17916 ) ;
#16132 = CARTESIAN_POINT ( 'NONE',  ( 0.4449199297089959648, -1.104150615014060977, -0.4000593327082896389 ) ) ;
#16133 = CARTESIAN_POINT ( 'NONE',  ( 0.02591418161326580066, -1.064383994110095877, 0.6545759956939124491 ) ) ;
#16134 = CARTESIAN_POINT ( 'NONE',  ( 0.5003933895997771941, -1.101010879683239629, 0.6202731239902519178 ) ) ;
#16135 = PERSON_AND_ORGANIZATION_ROLE ( 'classification_officer' ) ;
#16136 = DIRECTION ( 'NONE',  ( 0.4999551463232372317, -0.8660512985181135770, 0.000000000000000000 ) ) ;
#16137 = APPLIED_APPROVAL_ASSIGNMENT ( #408, ( #40563 ) ) ;
#16138 = CARTESIAN_POINT ( 'NONE',  ( -0.03868264068766711500, 0.4624969084406940767, -0.1149348357506045082 ) ) ;
#16139 = CIRCLE ( 'NONE', #35197, 0.03000000000000002318 ) ;
#16140 = CARTESIAN_POINT ( 'NONE',  ( -0.03647137243075569690, 0.08366781003817685969, 0.5049290013154925649 ) ) ;
#16141 = EDGE_LOOP ( 'NONE', ( #38333, #9335, #2925, #24942 ) ) ;
#16142 = CARTESIAN_POINT ( 'NONE',  ( -0.07811717810578547305, 0.05441343863104623063, -0.1146970785768719608 ) ) ;
#16143 = DIRECTION ( 'NONE',  ( -1.000000000000000000, -0.000000000000000000, -0.000000000000000000 ) ) ;
#16144 = CARTESIAN_POINT ( 'NONE',  ( 0.08794433374487309329, -0.6550045186490311977, 0.02677513513356245822 ) ) ;
#16145 = VERTEX_POINT ( 'NONE', #31511 ) ;
#16146 = DIRECTION ( 'NONE',  ( 1.000000000000000000, 0.000000000000000000, 0.000000000000000000 ) ) ;
#16147 = CARTESIAN_POINT ( 'NONE',  ( 0.06554679988413804337, -1.239417238573976787, 0.7589085834725802782 ) ) ;
#16149 = ORIENTED_EDGE ( 'NONE', *, *, #31387, .T. ) ;
#16148 = ORIENTED_EDGE ( 'NONE', *, *, #16068, .F. ) ;
#16150 = DIRECTION ( 'NONE',  ( 0.000000000000000000, 0.000000000000000000, -1.000000000000000000 ) ) ;
#16151 = EDGE_LOOP ( 'NONE', ( #48, #10410, #35620, #8752, #4895, #11491 ) ) ;
#16152 = CARTESIAN_POINT ( 'NONE',  ( 0.6343156381093978391, -1.595758837318228318, -0.5875140676452393906 ) ) ;
#16153 = CARTESIAN_POINT ( 'NONE',  ( 0.3540817610093318635, -1.633452470505663667, 0.5182417262812423209 ) ) ;
#16155 = CARTESIAN_POINT ( 'NONE',  ( 0.1837188672183508453, -1.376100911138345761, 0.5510147385948768184 ) ) ;
#16154 = CARTESIAN_POINT ( 'NONE',  ( 0.02242905165738221310, 0.4611019942560743989, 0.2233384654055277641 ) ) ;
#16156 = CIRCLE ( 'NONE', #38489, 0.01500000000000005322 ) ;
#16157 = FACE_OUTER_BOUND ( 'NONE', #5549, .T. ) ;
#16158 = ORIENTED_EDGE ( 'NONE', *, *, #34775, .F. ) ;
#16159 = CARTESIAN_POINT ( 'NONE',  ( 0.2237400956572660471, -0.6730011667035054046, 0.6888067665799237904 ) ) ;
#16160 = CIRCLE ( 'NONE', #18801, 0.7750185148639454624 ) ;
#16161 = ORIENTED_EDGE ( 'NONE', *, *, #15710, .T. ) ;
#16162 = EDGE_LOOP ( 'NONE', ( #29651, #30620, #1497, #35410, #14791, #20849, #18005 ) ) ;
#16163 = CARTESIAN_POINT ( 'NONE',  ( 0.2241624023114427433, -0.8762251062628222398, 0.6812710069543531644 ) ) ;
#16164 = EDGE_LOOP ( 'NONE', ( #32722, #15103, #6154, #13046 ) ) ;
#16165 = VERTEX_POINT ( 'NONE', #38696 ) ;
#16166 = CARTESIAN_POINT ( 'NONE',  ( 0.001988497880919273385, -0.4774668436778984892, 0.3122510010075223441 ) ) ;
#16167 = CARTESIAN_POINT ( 'NONE',  ( 0.07778086292406850843, -0.5899326820504365854, 0.3178732319592481037 ) ) ;
#16169 = CARTESIAN_POINT ( 'NONE',  ( -0.1105109110478532802, -0.5048634036869349417, 0.3351973644282389420 ) ) ;
#16168 = CARTESIAN_POINT ( 'NONE',  ( 0.03036294788238842746, -0.7483465999182054018, 0.6255648834759816035 ) ) ;
#16170 = CARTESIAN_POINT ( 'NONE',  ( 0.6127029595038788745, -1.475330056106460175, 0.4882469897972008255 ) ) ;
#16171 = CARTESIAN_POINT ( 'NONE',  ( 0.1410436376702208783, -0.9237311270473411717, 0.1925856316968101722 ) ) ;
#16172 = APPLIED_APPROVAL_ASSIGNMENT ( #8891, ( #8373 ) ) ;
#16173 = DIRECTION ( 'NONE',  ( 0.01265474379914247223, 0.8659329421511292590, -0.4999999971568669932 ) ) ;
#16174 = CARTESIAN_POINT ( 'NONE',  ( 0.4220651889022443704, -1.705682529110253753, -0.5196166052937188917 ) ) ;
#16175 = CARTESIAN_POINT ( 'NONE',  ( 0.2439137596789311413, -0.8887190363322325926, 0.6933903873120049743 ) ) ;
#16176 = AXIS2_PLACEMENT_3D ( 'NONE', #38364, #19259, #31803 ) ;
#16177 = CARTESIAN_POINT ( 'NONE',  ( -0.02953079040095652960, 0.2329676531120518090, 0.4763574306556300764 ) ) ;
#16178 = DIRECTION ( 'NONE',  ( 0.000000000000000000, -0.5237184928541299689, 0.8518913899333638851 ) ) ;
#16179 = CARTESIAN_POINT ( 'NONE',  ( -0.02953079040095700838, 0.000000000000000000, 0.000000000000000000 ) ) ;
#16180 = CARTESIAN_POINT ( 'NONE',  ( 0.2143793204313029777, -0.6499299462495844448, 0.4116214953459712556 ) ) ;
#16181 = DIRECTION ( 'NONE',  ( -1.000000000000000000, -2.276539994720197063E-15, 0.000000000000000000 ) ) ;
#16182 = CARTESIAN_POINT ( 'NONE',  ( 0.02461225487835269621, -1.084833808655251364, 0.6449087556199543103 ) ) ;
#16183 = CARTESIAN_POINT ( 'NONE',  ( 0.04760578872586068017, 0.4435171289962488994, -0.1893230556938475806 ) ) ;
#16184 = AXIS2_PLACEMENT_3D ( 'NONE', #14987, #14787, #11698 ) ;
#16185 = CARTESIAN_POINT ( 'NONE',  ( 0.1923911736828807784, -0.6113561202327233435, 0.3150503200843174922 ) ) ;
#16186 = CARTESIAN_POINT ( 'NONE',  ( 0.1876172797476865217, -0.9222972260603201633, 0.6278714507645634102 ) ) ;
#16187 = EDGE_CURVE ( 'NONE', #26513, #14366, #8060, .T. ) ;
#16188 = CARTESIAN_POINT ( 'NONE',  ( 0.01548846960712797240, 0.07651041855115807422, 0.5222379212567064277 ) ) ;
#16189 = PLANE ( 'NONE',  #25192 ) ;
#16190 = LOCAL_TIME ( 0, 53, 7.000000000000000000, #5804 ) ;
#16191 = ORIENTED_EDGE ( 'NONE', *, *, #28286, .T. ) ;
#16192 = CARTESIAN_POINT ( 'NONE',  ( 0.3409152363046967782, -1.516880185093673061, -0.4991292961807996531 ) ) ;
#16193 = CARTESIAN_POINT ( 'NONE',  ( 0.4219866632171927479, -1.610104465087647041, -0.3647299066799422618 ) ) ;
#16194 = CARTESIAN_POINT ( 'NONE',  ( 0.5612334960093817715, -1.620627794947044897, -0.4868944820179722521 ) ) ;
#16195 = CARTESIAN_POINT ( 'NONE',  ( 0.1077839203105155352, -1.313547715378476477, 0.4360033019131892562 ) ) ;
#16196 = CIRCLE ( 'NONE', #37865, 0.1400000000000005684 ) ;
#16197 = ORIENTED_EDGE ( 'NONE', *, *, #38648, .T. ) ;
#16198 = CARTESIAN_POINT ( 'NONE',  ( -0.1696286242763907215, 0.4941126639394833875, 0.3207424310465851192 ) ) ;
#16199 = EDGE_CURVE ( 'NONE', #40356, #11170, #22080, .T. ) ;
#16200 = DIRECTION ( 'NONE',  ( 0.000000000000000000, 0.000000000000000000, -1.000000000000000000 ) ) ;
#16201 = DIRECTION ( 'NONE',  ( 1.000000000000000000, 1.113825344428167933E-31, -7.771561172376107616E-16 ) ) ;
#16202 = APPLIED_PERSON_AND_ORGANIZATION_ASSIGNMENT ( #38927, #7667, ( #37152 ) ) ;
#16203 = CARTESIAN_POINT ( 'NONE',  ( 0.2011892967074958294, -1.251141541415955905, -0.7187326247832954706 ) ) ;
#16204 = CARTESIAN_POINT ( 'NONE',  ( 0.5114492881455343642, -1.312534973236980207, 0.6060176179980171218 ) ) ;
#16206 = CARTESIAN_POINT ( 'NONE',  ( 0.3177034180418226716, -1.763592183760435139, 0.5237719207440205693 ) ) ;
#16205 = DIRECTION ( 'NONE',  ( -8.881784197001246407E-16, 2.361472542561082612E-16, -1.000000000000000000 ) ) ;
#16207 = CARTESIAN_POINT ( 'NONE',  ( 0.4927680500253098783, -1.082617619565096723, 0.5740975660237009892 ) ) ;
#16208 = VERTEX_POINT ( 'NONE', #23294 ) ;
#16209 = CARTESIAN_POINT ( 'NONE',  ( 0.03244452491656055204, -0.9937768954163109791, 0.6733904430455559531 ) ) ;
#16210 = VERTEX_POINT ( 'NONE', #35819 ) ;
#16211 = VERTEX_POINT ( 'NONE', #26781 ) ;
#16212 = CARTESIAN_POINT ( 'NONE',  ( 0.2241274359060463905, -1.183323756640323188, 0.8809317799930992399 ) ) ;
#16214 = CARTESIAN_POINT ( 'NONE',  ( 0.1745799861983162171, -0.9110852329601157873, 0.09004006346363319091 ) ) ;
#16213 = CARTESIAN_POINT ( 'NONE',  ( 0.08638846605571078030, -0.7763520792700653317, 0.03197444058538126410 ) ) ;
#16215 = DIRECTION ( 'NONE',  ( 0.000000000000000000, -3.414809992080329122E-15, -1.000000000000000000 ) ) ;
#16216 = EDGE_LOOP ( 'NONE', ( #27990, #24711, #3137, #27115, #21886 ) ) ;
#16217 = AXIS2_PLACEMENT_3D ( 'NONE', #14040, #10976, #26618 ) ;
#16218 = CARTESIAN_POINT ( 'NONE',  ( 0.5382321766149011921, -1.161161941655080465, 0.5682417262808779901 ) ) ;
#16219 = CARTESIAN_POINT ( 'NONE',  ( 0.5679525285178691485, -1.502762679576377547, 0.6000120267691632092 ) ) ;
#16220 = VERTEX_POINT ( 'NONE', #7632 ) ;
#16221 = DIRECTION ( 'NONE',  ( -1.000000000000000000, -0.000000000000000000, -0.000000000000000000 ) ) ;
#16222 = CARTESIAN_POINT ( 'NONE',  ( 0.05999999999999990757, 0.7171888913565960255, -0.2325238883388469069 ) ) ;
#16223 = APPLIED_SECURITY_CLASSIFICATION_ASSIGNMENT ( #38548, ( #40665 ) ) ;
#16224 = DIRECTION ( 'NONE',  ( 0.4999551463232373427, -0.8660512985181134660, 0.000000000000000000 ) ) ;
#16225 = FACE_OUTER_BOUND ( 'NONE', #40265, .T. ) ;
#16226 = CARTESIAN_POINT ( 'NONE',  ( 0.1499999999999994671, 0.5346638663566677385, -0.07572681171513587217 ) ) ;
#16227 = CARTESIAN_POINT ( 'NONE',  ( -0.1210148435730033917, -0.5061394519556894345, 0.1438724812234795092 ) ) ;
#16228 = ADVANCED_FACE ( 'NONE', ( #30238 ), #17509, .T. ) ;
#16229 = CARTESIAN_POINT ( 'NONE',  ( 0.5225354986670117663, -1.146792065252953297, 0.8742509268737332917 ) ) ;
#16230 = EDGE_CURVE ( 'NONE', #8849, #10513, #23009, .T. ) ;
#16231 = CARTESIAN_POINT ( 'NONE',  ( 0.3985951925633877124, -2.053915860785213265, -0.5118549077720337959 ) ) ;
#16232 = DIRECTION ( 'NONE',  ( 5.551115123125783935E-17, 0.000000000000000000, -1.000000000000000000 ) ) ;
#16233 = DIRECTION ( 'NONE',  ( 0.8660512985181133550, 0.4999551463232372317, 0.000000000000000000 ) ) ;
#16234 = PERSON_AND_ORGANIZATION ( #28500, #32463 ) ;
#16235 = EDGE_CURVE ( 'NONE', #36014, #39055, #33133, .T. ) ;
#16236 = CARTESIAN_POINT ( 'NONE',  ( -0.07999999999999998779, -2.504411011601259673, -0.4441669705721119632 ) ) ;
#16237 = CARTESIAN_POINT ( 'NONE',  ( -0.2399999999999999079, -3.941790907013290823, -0.4709369376873030477 ) ) ;
#16238 = ADVANCED_FACE ( 'NONE', ( #27178 ), #17900, .T. ) ;
#16239 = CARTESIAN_POINT ( 'NONE',  ( 0.05999999999999990757, 0.03243672405480754750, -0.03647157466310641666 ) ) ;
#16240 = DIRECTION ( 'NONE',  ( 0.000000000000000000, -0.5781348229923771731, 0.8159412518334715481 ) ) ;
#16241 = CARTESIAN_POINT ( 'NONE',  ( 0.003124719664520334353, -0.5686731593868922241, 0.1635439462316863046 ) ) ;
#16242 = CARTESIAN_POINT ( 'NONE',  ( -0.0001024326674552539332, -0.7830864717413182907, -0.08467859722999726557 ) ) ;
#16243 = CARTESIAN_POINT ( 'NONE',  ( -0.3000000000000000999, -3.730063144961804245, -0.1064410973704724289 ) ) ;
#16244 = AXIS2_PLACEMENT_3D ( 'NONE', #20847, #17336, #11363 ) ;
#16245 = CARTESIAN_POINT ( 'NONE',  ( 0.3668746095265680296, -1.158496670723083710, 0.4182417262808777458 ) ) ;
#16246 = ORIENTED_EDGE ( 'NONE', *, *, #27283, .T. ) ;
#16247 = ORIENTED_EDGE ( 'NONE', *, *, #24087, .T. ) ;
#16248 = ADVANCED_FACE ( 'NONE', ( #50 ), #21199, .T. ) ;
#16249 = CARTESIAN_POINT ( 'NONE',  ( 0.5403448000457758971, -1.667326427136834432, -0.4959994330086618941 ) ) ;
#16250 = VERTEX_POINT ( 'NONE', #18316 ) ;
#16251 = CARTESIAN_POINT ( 'NONE',  ( 0.3794340307020034886, -1.736095262011157825, 0.4301452658221664449 ) ) ;
#16252 = CARTESIAN_POINT ( 'NONE',  ( -0.02000000000000000042, -2.071870001606465284, -0.3441689154348898105 ) ) ;
#16253 = CARTESIAN_POINT ( 'NONE',  ( 0.5048440467754061745, -1.307303468802018864, 0.7988581323005864432 ) ) ;
#16255 = ORIENTED_EDGE ( 'NONE', *, *, #27792, .F. ) ;
#16254 = LINE ( 'NONE', #32076, #10101 ) ;
#16256 = ORIENTED_EDGE ( 'NONE', *, *, #8448, .F. ) ;
#16257 = CARTESIAN_POINT ( 'NONE',  ( 0.1927077495703349852, -0.8180328145591141409, 0.2791508387892263077 ) ) ;
#16258 = ORIENTED_EDGE ( 'NONE', *, *, #32624, .T. ) ;
#16259 = CARTESIAN_POINT ( 'NONE',  ( 0.3001998578127315076, -1.656212505849981698, 0.6213433347872623358 ) ) ;
#16261 = CARTESIAN_POINT ( 'NONE',  ( 0.1115696861367231063, -0.8921960531934336469, 0.01816369405970581427 ) ) ;
#16260 = CARTESIAN_POINT ( 'NONE',  ( 0.000000000000000000, 0.000000000000000000, 0.000000000000000000 ) ) ;
#16262 = DIRECTION ( 'NONE',  ( -0.4999999999999968359, 0.7308273574226419322, 0.4646411234949411884 ) ) ;
#16263 = FACE_OUTER_BOUND ( 'NONE', #1695, .T. ) ;
#16264 = CARTESIAN_POINT ( 'NONE',  ( 0.02988687873307911344, -2.020173214415363461, -0.2839403628030972571 ) ) ;
#16266 = VERTEX_POINT ( 'NONE', #18725 ) ;
#16265 = VERTEX_POINT ( 'NONE', #24494 ) ;
#16267 = CARTESIAN_POINT ( 'NONE',  ( 0.1942853770376357925, -0.8441127787454487663, 0.2952251170591385088 ) ) ;
#16268 = CARTESIAN_POINT ( 'NONE',  ( -0.1710642718812829255, 0.4986889572247755198, 0.3749999999999999445 ) ) ;
#16269 = CARTESIAN_POINT ( 'NONE',  ( 0.6018439701642503969, -1.465521054425967362, 0.6780457446538449284 ) ) ;
#16270 = DIRECTION ( 'NONE',  ( 0.000000000000000000, -0.5365213554527457074, 0.8438867430782097667 ) ) ;
#16271 = DIRECTION ( 'NONE',  ( 1.000000000000000000, -0.000000000000000000, -0.000000000000000000 ) ) ;
#16272 = CARTESIAN_POINT ( 'NONE',  ( 0.4227463786284310632, -1.145941386794042671, 0.4182417262808777458 ) ) ;
#16273 = B_SPLINE_CURVE_WITH_KNOTS ( 'NONE', 3,
 ( #27794, #30681, #40538, #28002, #34153, #15846, #12360, #2497 ),
 .UNSPECIFIED., .F., .F.,
 ( 4, 2, 2, 4 ),
 ( 1.734723475976807094E-18, 0.0005953189690397796881, 0.0008929784535596708333, 0.001190637938079561978 ),
 .UNSPECIFIED. ) ;
#16274 = LINE ( 'NONE', #673, #31093 ) ;
#16275 = ADVANCED_FACE ( 'NONE', ( #40317 ), #6162, .T. ) ;
#16276 = DIRECTION ( 'NONE',  ( 1.000000000000000000, 0.000000000000000000, 0.000000000000000000 ) ) ;
#16277 = CARTESIAN_POINT ( 'NONE',  ( -0.3000000000000000999, -2.416006048095809877, -1.059240699271965402 ) ) ;
#16278 = DIRECTION ( 'NONE',  ( 1.000000000000000000, 0.000000000000000000, 0.000000000000000000 ) ) ;
#16279 = ADVANCED_FACE ( 'NONE', ( #8436 ), #33522, .F. ) ;
#16280 = CARTESIAN_POINT ( 'NONE',  ( 0.03674078017395952106, -0.3145504785376008750, 0.3636064179578495925 ) ) ;
#16281 = EDGE_CURVE ( 'NONE', #34829, #30207, #25141, .T. ) ;
#16282 = DIRECTION ( 'NONE',  ( -7.771561172376107616E-16, 7.170354002788761615E-17, -1.000000000000000000 ) ) ;
#16283 = AXIS2_PLACEMENT_3D ( 'NONE', #29647, #35614, #26577 ) ;
#16284 = CARTESIAN_POINT ( 'NONE',  ( 0.1877114757398583578, -1.688462026347908873, -0.6542463691362495615 ) ) ;
#16285 = PERSON_AND_ORGANIZATION ( #28500, #32463 ) ;
#16286 = EDGE_CURVE ( 'NONE', #30856, #36434, #11334, .T. ) ;
#16287 = CARTESIAN_POINT ( 'NONE',  ( 0.3561222603844115264, -1.742508409003949987, 0.4387334599642109811 ) ) ;
#16288 = CARTESIAN_POINT ( 'NONE',  ( 0.2156332787663666484, -1.620970839068891944, -0.6635100984292762183 ) ) ;
#16289 = FACE_OUTER_BOUND ( 'NONE', #36808, .T. ) ;
#16290 = CARTESIAN_POINT ( 'NONE',  ( -0.02000000000000000042, -2.183180860297908144, -0.4312760292030870524 ) ) ;
#16291 = EDGE_CURVE ( 'NONE', #26127, #9912, #27777, .T. ) ;
#16292 = CARTESIAN_POINT ( 'NONE',  ( 0.3564258580595303649, -1.150190177429248672, 0.4382532076974842705 ) ) ;
#16293 = EDGE_LOOP ( 'NONE', ( #32088, #28831, #30049, #17688 ) ) ;
#16294 = CARTESIAN_POINT ( 'NONE',  ( 0.1058947752955989308, -1.412241959666070912, 0.5633263997903267262 ) ) ;
#16295 = CARTESIAN_POINT ( 'NONE',  ( 0.2711279843670483802, -1.680576011916085521, 0.6848605795586665268 ) ) ;
#16296 = ADVANCED_FACE ( 'NONE', ( #27989 ), #12542, .F. ) ;
#16297 = CARTESIAN_POINT ( 'NONE',  ( 0.1317540737835982967, -0.5510263468228310257, 0.1457185332388695742 ) ) ;
#16299 = ORIENTED_EDGE ( 'NONE', *, *, #26115, .F. ) ;
#16298 = CARTESIAN_POINT ( 'NONE',  ( 0.5213789366507165512, -1.637636803980936362, -0.4211300373884619974 ) ) ;
#16300 = ADVANCED_FACE ( 'NONE', ( #5550 ), #8629, .T. ) ;
#16302 = EDGE_LOOP ( 'NONE', ( #19226, #38238, #34561, #5757 ) ) ;
#16301 = ORIENTED_EDGE ( 'NONE', *, *, #10741, .F. ) ;
#16303 = CARTESIAN_POINT ( 'NONE',  ( -0.05464101615137795936, -1.598492537578166672, -0.1971380022280825872 ) ) ;
#16304 = EDGE_LOOP ( 'NONE', ( #19841, #14055, #26735, #9345, #14875, #7123, #6804, #15184, #28267, #3896, #30704, #8027, #5996, #6300, #40, #16980, #9965 ) ) ;
#16305 = VERTEX_POINT ( 'NONE', #33738 ) ;
#16306 = CARTESIAN_POINT ( 'NONE',  ( 0.000000000000000000, 0.000000000000000000, 0.000000000000000000 ) ) ;
#16307 = CARTESIAN_POINT ( 'NONE',  ( -0.1743922129835733803, -0.5166151207188712791, 0.3749999999999999445 ) ) ;
#16308 = CONTEXT_DEPENDENT_SHAPE_REPRESENTATION ( #34768, #17019 ) ;
#16309 = FACE_OUTER_BOUND ( 'NONE', #11544, .T. ) ;
#16310 = EDGE_LOOP ( 'NONE', ( #37097, #23026 ) ) ;
#16311 = CARTESIAN_POINT ( 'NONE',  ( 0.1340034493811799732, -0.8053594121975541364, 0.4832924993268126190 ) ) ;
#16312 = CIRCLE ( 'NONE', #39288, 0.9237847906030155487 ) ;
#16313 = CARTESIAN_POINT ( 'NONE',  ( 0.06924669681850037506, -0.5400070402892428456, 0.1467347635635346537 ) ) ;
#16314 = CARTESIAN_POINT ( 'NONE',  ( 0.5390309913773138062, -1.513666831327822537, 0.6478081614881986416 ) ) ;
#16315 = CARTESIAN_POINT ( 'NONE',  ( 0.6272266378578528201, -1.617171174196860628, -0.5046292136067113132 ) ) ;
#16316 = CARTESIAN_POINT ( 'NONE',  ( -0.1628171590788634604, 0.5058980335669979178, 0.1333422639292566048 ) ) ;
#16317 = FACE_OUTER_BOUND ( 'NONE', #10228, .T. ) ;
#16318 = CARTESIAN_POINT ( 'NONE',  ( 0.3715339819472113225, -1.730447381542274066, 0.6049165315556401801 ) ) ;
#16319 = CARTESIAN_POINT ( 'NONE',  ( 0.6898418300915178936, -1.417705155587995369, 0.6911030477506114877 ) ) ;
#16320 = CARTESIAN_POINT ( 'NONE',  ( 0.1048591973540500683, -1.410537849644770025, 0.5682417262808777680 ) ) ;
#16321 = CARTESIAN_POINT ( 'NONE',  ( 0.6011624602559976216, -1.464707089772093740, 0.6803405452985709090 ) ) ;
#16322 = CARTESIAN_POINT ( 'NONE',  ( -0.1684323895665170989, 0.5231977504176972271, 0.3102582297535285139 ) ) ;
#16323 = ADVANCED_FACE ( 'NONE', ( #30857 ), #30668, .T. ) ;
#16324 = CARTESIAN_POINT ( 'NONE',  ( 0.2320755761173002307, -1.232873731908348480, 0.4177417262808779674 ) ) ;
#16325 = CARTESIAN_POINT ( 'NONE',  ( 0.4659739283829816836, -1.067701485818283835, -0.6091934467387866148 ) ) ;
#16326 = EDGE_CURVE ( 'NONE', #36862, #5225, #19585, .T. ) ;
#16327 = CARTESIAN_POINT ( 'NONE',  ( 0.0008242595369169036616, -0.9534780057342879811, 0.2825590231195395652 ) ) ;
#16328 = CARTESIAN_POINT ( 'NONE',  ( 0.4004013247085298488, -1.001184149470538909, 0.6774742858917212063 ) ) ;
#16329 = DATE_TIME_ROLE ( 'creation_date' ) ;
#16330 = DIRECTION ( 'NONE',  ( 0.000000000000000000, 0.8660489055767764954, 0.4999592914920847897 ) ) ;
#16331 = CARTESIAN_POINT ( 'NONE',  ( 0.3806791355520856568, -1.717835243773888854, 0.4208876441603489615 ) ) ;
#16332 = CARTESIAN_POINT ( 'NONE',  ( -0.02881302694829873320, -0.06014213504334085109, 0.4945521340962454881 ) ) ;
#16333 = ORIENTED_EDGE ( 'NONE', *, *, #5238, .F. ) ;
#16334 = LINE ( 'NONE', #19624, #16772 ) ;
#16335 = CARTESIAN_POINT ( 'NONE',  ( 0.01055999354155550199, -0.5296565605740121141, 0.1467999231854481279 ) ) ;
#16336 = CARTESIAN_POINT ( 'NONE',  ( 0.1857430203655689449, -0.8056635886342103925, 0.2698372336795830662 ) ) ;
#16337 = ORIENTED_EDGE ( 'NONE', *, *, #35891, .T. ) ;
#16338 = CARTESIAN_POINT ( 'NONE',  ( 0.1438681892407857876, -1.284094082863941111, 0.3157417262808777658 ) ) ;
#16339 = CARTESIAN_POINT ( 'NONE',  ( 0.6789872039812443472, -1.407470790535994221, 0.5375528621076278712 ) ) ;
#16341 = ORIENTED_EDGE ( 'NONE', *, *, #15554, .F. ) ;
#16340 = ORIENTED_EDGE ( 'NONE', *, *, #22571, .T. ) ;
#16342 = DIRECTION ( 'NONE',  ( 1.000000000000000000, 2.341930812374887555E-31, -1.664003471950578127E-31 ) ) ;
#16343 =( BOUNDED_SURFACE ( )  B_SPLINE_SURFACE ( 3, 2, ( 
 ( #40636, #7080, #25006 ),
 ( #19460, #19046, #34469 ),
 ( #31793, #6674, #38354 ),
 ( #3610, #3997, #6284 ),
 ( #31397, #15741, #156 ),
 ( #37539, #34865, #31578 ),
 ( #12877, #38156, #16362 ),
 ( #9979, #22761, #31994 ),
 ( #15953, #12651, #25213 ),
 ( #28108, #9362, #19651 ),
 ( #32184, #37759, #9580 ),
 ( #22157, #35079, #6882 ),
 ( #22548, #25435, #37966 ),
 ( #3806, #22348, #28899 ),
 ( #760, #35285, #32597 ),
 ( #967, #7270, #16969 ),
 ( #4409, #29320, #16558 ),
 ( #1557, #23372, #14282 ),
 ( #38753, #13666, #38565 ),
 ( #4207, #8099, #26232 ),
 ( #20267, #35894, #26847 ),
 ( #32381, #16771, #13478 ) ),
 .UNSPECIFIED., .F., .F., .T. ) 
 B_SPLINE_SURFACE_WITH_KNOTS ( ( 4, 2, 2, 2, 2, 2, 2, 2, 2, 2, 4 ),
 ( 3, 3 ),
 ( 0.002013519961495850892, 0.002780892266055758240, 0.003548264570615666021, 0.004315636875175573803, 0.004699323027455527477, 0.005083009179735481151, 0.005466695332015434824, 0.005850381484295388498, 0.006617753788855296714, 0.007385126093415204929, 0.008152498397975112276 ),
 ( 0.000000000000000000, 1.000000000000000000 ),
 .UNSPECIFIED. ) 
 GEOMETRIC_REPRESENTATION_ITEM ( )  RATIONAL_B_SPLINE_SURFACE ( (
 ( 1.000000000000000000, 0.7283825911960390975, 1.000000000000000000),
 ( 1.000000000000000000, 0.7404375345927360907, 1.000000000000000000),
 ( 1.000000000000000000, 0.7521483142435548830, 1.000000000000000000),
 ( 1.000000000000000000, 0.7744460733776878936, 1.000000000000000000),
 ( 1.000000000000000000, 0.7845612039380914782, 1.000000000000000000),
 ( 1.000000000000000000, 0.8022035258263230384, 1.000000000000000000),
 ( 1.000000000000000000, 0.8093965293320422028, 1.000000000000000000),
 ( 1.000000000000000000, 0.8169028692726111318, 1.000000000000000000),
 ( 1.000000000000000000, 0.8188329634863092954, 1.000000000000000000),
 ( 1.000000000000000000, 0.8214004505364272957, 1.000000000000000000),
 ( 1.000000000000000000, 0.8220602406261449113, 1.000000000000000000),
 ( 1.000000000000000000, 0.8220736605435178257, 1.000000000000000000),
 ( 1.000000000000000000, 0.8214126668415498989, 1.000000000000000000),
 ( 1.000000000000000000, 0.8188520474558501627, 1.000000000000000000),
 ( 1.000000000000000000, 0.8169545908334044926, 1.000000000000000000),
 ( 1.000000000000000000, 0.8094771004220393529, 1.000000000000000000),
 ( 1.000000000000000000, 0.8022723753807737834, 1.000000000000000000),
 ( 1.000000000000000000, 0.7845733350637268400, 1.000000000000000000),
 ( 1.000000000000000000, 0.7744472902493437783, 1.000000000000000000),
 ( 1.000000000000000000, 0.7522916829163295294, 1.000000000000000000),
 ( 1.000000000000000000, 0.7403553004665951454, 1.000000000000000000),
 ( 1.000000000000000000, 0.7283825911960403188, 1.000000000000000000) ) ) 
 REPRESENTATION_ITEM ( '' )  SURFACE ( )  );
#16344 = ORIENTED_EDGE ( 'NONE', *, *, #39380, .T. ) ;
#16345 = DIRECTION ( 'NONE',  ( -0.5000000000000004441, -4.190823558986626968E-31, -0.8660254037844383745 ) ) ;
#16346 = DIRECTION ( 'NONE',  ( 1.000000000000000000, 0.000000000000000000, 0.000000000000000000 ) ) ;
#16347 = CARTESIAN_POINT ( 'NONE',  ( 0.03647137243074413671, 0.4543612417835987682, 0.2356044583002223913 ) ) ;
#16348 = FACE_OUTER_BOUND ( 'NONE', #31811, .T. ) ;
#16349 = EDGE_LOOP ( 'NONE', ( #5640, #19219, #15446, #28278 ) ) ;
#16350 = CARTESIAN_POINT ( 'NONE',  ( 0.04687500000000013878, -0.4345172148286635116, 0.1457185332388691301 ) ) ;
#16351 = CARTESIAN_POINT ( 'NONE',  ( 0.1770748127338239997, -0.8007700866384124261, 0.6050427707434069546 ) ) ;
#16352 = EDGE_LOOP ( 'NONE', ( #2078, #29707, #23906, #16337, #26790, #38646, #20904 ) ) ;
#16353 = CARTESIAN_POINT ( 'NONE',  ( 0.01610093497955936842, -0.4922387448986250136, 0.3764339700947045286 ) ) ;
#16354 = CARTESIAN_POINT ( 'NONE',  ( 0.4697542972204731826, -1.557995369357642934, 0.5737367010564736747 ) ) ;
#16356 = CARTESIAN_POINT ( 'NONE',  ( -0.1204800139379097468, -0.5035717010276847816, 0.3194901984145592233 ) ) ;
#16355 = CARTESIAN_POINT ( 'NONE',  ( 0.5209049548566241361, -1.602498953031318729, -0.4230150025751962528 ) ) ;
#16357 = DIRECTION ( 'NONE',  ( 8.881784197001246407E-16, -2.361472542561082612E-16, 1.000000000000000000 ) ) ;
#16358 = CARTESIAN_POINT ( 'NONE',  ( 0.4442549097070609410, -1.097829417026605858, 0.6115672446538368279 ) ) ;
#16359 = ORIENTED_EDGE ( 'NONE', *, *, #16675, .T. ) ;
#16360 = CARTESIAN_POINT ( 'NONE',  ( 0.6364841839958734759, -1.591084691710345389, -0.5918496660566199274 ) ) ;
#16361 = CARTESIAN_POINT ( 'NONE',  ( 0.2325020897479753157, -1.594945628236600133, -0.3239020423276253724 ) ) ;
#16362 = CARTESIAN_POINT ( 'NONE',  ( -0.05279185365593493107, 0.3066183444142228653, -0.3541401447632883115 ) ) ;
#16363 = DIRECTION ( 'NONE',  ( 0.000000000000000000, 0.5365213554527465956, -0.8438867430782092116 ) ) ;
#16364 = EDGE_LOOP ( 'NONE', ( #22786, #1366, #37515, #11688 ) ) ;
#16365 = CARTESIAN_POINT ( 'NONE',  ( 0.5195754528810989648, -1.145330933930835959, 0.8096739517683957388 ) ) ;
#16366 = CARTESIAN_POINT ( 'NONE',  ( 0.4571661123351543066, -1.116215641761870936, 0.5698312831065212025 ) ) ;
#16367 = CARTESIAN_POINT ( 'NONE',  ( 0.06792916418419493729, -1.318672173847188711, 0.5972585457936512299 ) ) ;
#16368 = CARTESIAN_POINT ( 'NONE',  ( 0.04157143636675642712, 0.4416880288200873417, -0.1614235308635272315 ) ) ;
#16369 = CARTESIAN_POINT ( 'NONE',  ( 0.1949081798141291400, -0.7265219913688031328, 0.3259659631419143944 ) ) ;
#16370 = CARTESIAN_POINT ( 'NONE',  ( 0.3363202282376455132, -1.061977972960397976, 0.7384839447874953500 ) ) ;
#16371 = CARTESIAN_POINT ( 'NONE',  ( 0.5164663794816727327, -1.539710880569944207, 0.5182417262812423209 ) ) ;
#16372 = CARTESIAN_POINT ( 'NONE',  ( 0.6174474092321283747, -1.596955002812002089, 0.4316719645203795364 ) ) ;
#16373 = ORIENTED_EDGE ( 'NONE', *, *, #4922, .T. ) ;
#16374 = CARTESIAN_POINT ( 'NONE',  ( -0.3000000000000000999, -2.778907721888695281, -0.2599079779360263798 ) ) ;
#16375 = CARTESIAN_POINT ( 'NONE',  ( 0.3595715536228104581, -1.625401886829162867, -0.3696110269036071982 ) ) ;
#16376 = CARTESIAN_POINT ( 'NONE',  ( -1.502516396515344672E-15, -0.3899999999999999578, 5.463695987328526437E-16 ) ) ;
#16377 = CARTESIAN_POINT ( 'NONE',  ( 0.1429230018409890501, -1.294172685953591362, 0.4193902154642965563 ) ) ;
#16378 = B_SPLINE_CURVE_WITH_KNOTS ( 'NONE', 3,
 ( #35629, #9923, #19609, #32541, #918, #13422 ),
 .UNSPECIFIED., .F., .F.,
 ( 4, 2, 4 ),
 ( 0.000000000000000000, 0.5000000000000000000, 1.000000000000000000 ),
 .UNSPECIFIED. ) ;
#16379 = ORIENTED_EDGE ( 'NONE', *, *, #3712, .T. ) ;
#16380 = CARTESIAN_POINT ( 'NONE',  ( -0.1628177922134294298, 0.5059000297268239077, 0.3228062255482121445 ) ) ;
#16381 = CARTESIAN_POINT ( 'NONE',  ( 0.1863410289239364470, -0.5450895766423083932, 0.2630702390344190622 ) ) ;
#16382 = CARTESIAN_POINT ( 'NONE',  ( 0.4569551544390156317, -1.119309369577474955, -0.6070915220724588668 ) ) ;
#16383 = CARTESIAN_POINT ( 'NONE',  ( 0.3917195419103990384, -1.137763892611062699, 0.7222388353537541050 ) ) ;
#16385 = LINE ( 'NONE', #793, #12855 ) ;
#16384 = CARTESIAN_POINT ( 'NONE',  ( 0.01548846960707524721, 0.2306506793133126232, 0.4716198300880778960 ) ) ;
#16386 = CARTESIAN_POINT ( 'NONE',  ( 0.4912263342062789806, -1.081771733098906729, 0.5857582446664630904 ) ) ;
#16387 = ORIENTED_EDGE ( 'NONE', *, *, #10680, .T. ) ;
#16388 = SECURITY_CLASSIFICATION_LEVEL ( 'unclassified' ) ;
#16389 = DIRECTION ( 'NONE',  ( 1.000000000000000000, -0.000000000000000000, -0.000000000000000000 ) ) ;
#16390 = EDGE_LOOP ( 'NONE', ( #32671, #28792, #3489, #32013 ) ) ;
#16391 = ORIENTED_EDGE ( 'NONE', *, *, #1272, .F. ) ;
#16392 = CARTESIAN_POINT ( 'NONE',  ( 0.3157976591183140336, -1.353229759395969678, 0.8845812709865115142 ) ) ;
#16394 = CARTESIAN_POINT ( 'NONE',  ( 0.1747443221411794922, -0.8985867114839785064, 0.05431702021998949942 ) ) ;
#16393 = CARTESIAN_POINT ( 'NONE',  ( -0.08408070219615604302, -0.09959325338431369856, 0.09999999999999892308 ) ) ;
#16395 = CARTESIAN_POINT ( 'NONE',  ( 0.1995529058109158649, -2.050896138459939344, -0.3054326997595754878 ) ) ;
#16396 = EDGE_LOOP ( 'NONE', ( #23305, #14603, #22595, #34057 ) ) ;
#16397 = B_SPLINE_CURVE_WITH_KNOTS ( 'NONE', 3,
 ( #35037, #19428, #31961, #3778, #728, #13229, #38322, #13443, #35858, #936, #29478, #35440 ),
 .UNSPECIFIED., .F., .F.,
 ( 4, 2, 2, 2, 2, 4 ),
 ( 0.001615335599980241782, 0.002213674370351530803, 0.002812013140722820041, 0.003410351911094108845, 0.003709521296279748477, 0.004008690681465387241 ),
 .UNSPECIFIED. ) ;
#16398 = ORIENTED_EDGE ( 'NONE', *, *, #2671, .T. ) ;
#16399 = DIRECTION ( 'NONE',  ( -1.000000000000000000, -0.000000000000000000, -0.000000000000000000 ) ) ;
#16400 = CARTESIAN_POINT ( 'NONE',  ( 0.4113960816100760698, -1.246834456972530703, 0.8355117767174224941 ) ) ;
#16401 = VERTEX_POINT ( 'NONE', #22237 ) ;
#16402 = CARTESIAN_POINT ( 'NONE',  ( 0.1874578000378240850, -0.6893444085712847613, 0.06304793604024336307 ) ) ;
#16403 = CYLINDRICAL_SURFACE ( 'NONE', #27902, 0.08139150547213643005 ) ;
#16404 = CARTESIAN_POINT ( 'NONE',  ( -0.3000000000000000999, -3.941790907013290823, -0.4709369376873030477 ) ) ;
#16405 = DIRECTION ( 'NONE',  ( 1.000000000000000000, 0.000000000000000000, 7.762195515159383243E-16 ) ) ;
#16406 = CARTESIAN_POINT ( 'NONE',  ( -1.019575837292303166, -0.04310840302197994911, 0.3599999999999993205 ) ) ;
#16407 = CARTESIAN_POINT ( 'NONE',  ( 0.03333333333331311293, -1.846784381541715314, -0.3501698912633309790 ) ) ;
#16408 = CARTESIAN_POINT ( 'NONE',  ( 0.3893341572580266141, -1.754502034563850454, -0.5437939363053549968 ) ) ;
#16409 = DIRECTION ( 'NONE',  ( 0.8660512985181134660, 0.4999551463232372872, 0.000000000000000000 ) ) ;
#16410 = LINE ( 'NONE', #28769, #25934 ) ;
#16411 = CARTESIAN_POINT ( 'NONE',  ( 0.3200662685693974052, -1.759564150209586897, 0.5682417262808787672 ) ) ;
#16412 = CARTESIAN_POINT ( 'NONE',  ( 0.09095675709397832431, -1.344211122730877506, 0.7083116771559543334 ) ) ;
#16413 = DATE_TIME_ROLE ( 'classification_date' ) ;
#16414 = APPLIED_DATE_AND_TIME_ASSIGNMENT ( #13304, #1755, ( #445 ) ) ;
#16415 = CARTESIAN_POINT ( 'NONE',  ( 0.3699999999999786793, -2.097675824466503691, -0.5196396315034578217 ) ) ;
#16416 = B_SPLINE_CURVE_WITH_KNOTS ( 'NONE', 3,
 ( #23312, #33153, #17110, #7220 ),
 .UNSPECIFIED., .F., .F.,
 ( 4, 4 ),
 ( 0.000000000000000000, 0.001650735412551658380 ),
 .UNSPECIFIED. ) ;
#16417 = CARTESIAN_POINT ( 'NONE',  ( -0.2399999999999999079, -3.880844374714816247, -0.2860650318788287017 ) ) ;
#16418 = CARTESIAN_POINT ( 'NONE',  ( 0.1840090184099318349, -0.5566218984093596056, 0.02008366405345159145 ) ) ;
#16419 = CARTESIAN_POINT ( 'NONE',  ( 0.4264813724157178187, -1.236570049007190919, 0.4854677512712051723 ) ) ;
#16420 = LINE ( 'NONE', #31862, #2850 ) ;
#16421 = CARTESIAN_POINT ( 'NONE',  ( 0.2518326032030922534, -1.639413698222365046, 0.7148483533190357342 ) ) ;
#16422 = CARTESIAN_POINT ( 'NONE',  ( 0.6134394428779069708, -1.489641535132577577, -0.4161639220292565611 ) ) ;
#16423 = CARTESIAN_POINT ( 'NONE',  ( -0.2399999999999999079, -3.291368864184588183, -0.6988176298300771139 ) ) ;
#16424 = CARTESIAN_POINT ( 'NONE',  ( 0.04293701532779483493, -0.2295363440003016231, 0.4381116105132966121 ) ) ;
#16425 = CYLINDRICAL_SURFACE ( 'NONE', #38107, 0.07999999999999996003 ) ;
#16426 = EDGE_LOOP ( 'NONE', ( #39371, #458, #21527, #28222, #1112, #4351 ) ) ;
#16427 = EDGE_LOOP ( 'NONE', ( #39071, #6105, #5386, #5659, #8190, #7063, #20495, #32716 ) ) ;
#16428 = EDGE_CURVE ( 'NONE', #9403, #28175, #36282, .T. ) ;
#16429 = CARTESIAN_POINT ( 'NONE',  ( 0.1727391575749071539, -1.224311773214861176, 0.5182417262812423209 ) ) ;
#16430 = ORIENTED_EDGE ( 'NONE', *, *, #8675, .T. ) ;
#16431 = DIRECTION ( 'NONE',  ( 0.9766636885342071528, -0.2147743920926261929, 1.138269997360109773E-15 ) ) ;
#16432 = CARTESIAN_POINT ( 'NONE',  ( 0.3593346688482154661, -1.735925422213635549, -0.5010936962835144115 ) ) ;
#16433 = CARTESIAN_POINT ( 'NONE',  ( 0.4994410488334536380, -1.297393737506421951, 0.7727712239381648862 ) ) ;
#16434 = CIRCLE ( 'NONE', #36803, 0.1600000000000001976 ) ;
#16436 = ORIENTED_EDGE ( 'NONE', *, *, #15423, .T. ) ;
#16435 = DIRECTION ( 'NONE',  ( -1.387778780781449423E-15, 6.691181741238501047E-16, -1.000000000000000000 ) ) ;
#16437 = CARTESIAN_POINT ( 'NONE',  ( 0.3392765801623501276, -0.9012043381553855870, 0.6651284465457234507 ) ) ;
#16438 = ORIENTED_EDGE ( 'NONE', *, *, #36308, .F. ) ;
#16439 = CARTESIAN_POINT ( 'NONE',  ( 0.2629665421248923995, -1.157745397434066126, -0.5155029497116575543 ) ) ;
#16440 = ADVANCED_FACE ( 'NONE', ( #25512 ), #1060, .T. ) ;
#16441 = EDGE_LOOP ( 'NONE', ( #18409, #30951, #6756 ) ) ;
#16442 = TOROIDAL_SURFACE ( 'NONE', #36873, 0.06434668806854092205, 0.005000000000000000104 ) ;
#16443 = CARTESIAN_POINT ( 'NONE',  ( 0.07674151747445530358, -0.8568903145152425571, 0.7207360041014601038 ) ) ;
#16445 = CARTESIAN_POINT ( 'NONE',  ( 0.1110248181161190423, -0.9270180154169346265, 0.1138591024880182823 ) ) ;
#16444 = CARTESIAN_POINT ( 'NONE',  ( 0.5457083359927942245, -1.652683498676156271, -0.4845597240607255607 ) ) ;
#16446 = DIRECTION ( 'NONE',  ( 0.000000000000000000, 0.000000000000000000, -1.000000000000000000 ) ) ;
#16447 = CARTESIAN_POINT ( 'NONE',  ( 0.3957364756389608607, -1.753984992610886584, -0.5139882692845931800 ) ) ;
#16448 = EDGE_CURVE ( 'NONE', #40210, #5485, #18558, .T. ) ;
#16449 = EDGE_CURVE ( 'NONE', #36513, #7506, #4101, .T. ) ;
#16450 = CARTESIAN_POINT ( 'NONE',  ( 0.09094713279931705696, -1.440988727485061682, -0.3374321700806039992 ) ) ;
#16452 = ORIENTED_EDGE ( 'NONE', *, *, #26985, .T. ) ;
#16451 = VERTEX_POINT ( 'NONE', #34751 ) ;
#16453 = EDGE_CURVE ( 'NONE', #3787, #16305, #10263, .T. ) ;
#16454 = CARTESIAN_POINT ( 'NONE',  ( 0.01548846960721255751, -0.3688619771570325612, 0.3775276577325259453 ) ) ;
#16455 = CARTESIAN_POINT ( 'NONE',  ( 0.1868366425318004342, -0.9712607208092176592, 0.5097868630048105754 ) ) ;
#16456 = CARTESIAN_POINT ( 'NONE',  ( -0.01548846960707348300, -0.4730347584886833157, 0.2341461249029785086 ) ) ;
#16457 = CARTESIAN_POINT ( 'NONE',  ( 0.5762190745332915753, -1.421659016055986990, 0.7172490134945124218 ) ) ;
#16458 = CARTESIAN_POINT ( 'NONE',  ( 0.3788791674705027090, -1.253375940808735489, 0.6247566768318951747 ) ) ;
#16459 = CARTESIAN_POINT ( 'NONE',  ( 0.05999999999999990757, 0.4357424459509059433, 0.2678820090948816901 ) ) ;
#16460 = CARTESIAN_POINT ( 'NONE',  ( 0.3405242896115074913, -1.744906522954273731, 0.4484829386636806081 ) ) ;
#16461 = B_SPLINE_CURVE_WITH_KNOTS ( 'NONE', 3,
 ( #9804, #22376, #26265, #13891, #11037, #26465 ),
 .UNSPECIFIED., .F., .F.,
 ( 4, 2, 4 ),
 ( 0.000000000000000000, 0.0005950409463462349047, 0.001190081892692469809 ),
 .UNSPECIFIED. ) ;
#16462 = CARTESIAN_POINT ( 'NONE',  ( -0.1593715683900499003, 0.4948507460962193183, 0.3535463917166182246 ) ) ;
#16463 = CARTESIAN_POINT ( 'NONE',  ( 0.4000099798367660608, -1.704638381955401183, 0.4182417262808776903 ) ) ;
#16464 = DIRECTION ( 'NONE',  ( -1.416619696839557898E-11, 0.000000000000000000, -1.000000000000000000 ) ) ;
#16465 = EDGE_CURVE ( 'NONE', #34098, #34794, #7304, .T. ) ;
#16466 = LINE ( 'NONE', #25733, #23380 ) ;
#16467 = COORDINATED_UNIVERSAL_TIME_OFFSET ( 0, 0, .AHEAD. ) ;
#16468 = PRODUCT_RELATED_PRODUCT_CATEGORY ( 'detail', '', ( #33451 ) ) ;
#16469 = CIRCLE ( 'NONE', #1393, 0.2500000000000000555 ) ;
#16470 = CYLINDRICAL_SURFACE ( 'NONE', #8840, 0.2000000000000000111 ) ;
#16471 = CARTESIAN_POINT ( 'NONE',  ( 0.1807325509464224600, -0.4982638852683227704, 0.1182772881561286321 ) ) ;
#16472 = CARTESIAN_POINT ( 'NONE',  ( 0.1748174088606663235, -1.825896565190340048, -0.6523992043106852101 ) ) ;
#16473 = AXIS2_PLACEMENT_3D ( 'NONE', #18506, #30662, #18310 ) ;
#16474 = FACE_OUTER_BOUND ( 'NONE', #9556, .T. ) ;
#16475 = CARTESIAN_POINT ( 'NONE',  ( 0.2738670336145942463, -1.555218499503542295, -0.6850478759345199897 ) ) ;
#16476 = CARTESIAN_POINT ( 'NONE',  ( -0.03170953572519233377, 0.4816881781209654823, 0.09938198567066955369 ) ) ;
#16477 = DIRECTION ( 'NONE',  ( 0.4987694591008374201, -0.8667346922030165768, 0.000000000000000000 ) ) ;
#16478 = DIRECTION ( 'NONE',  ( -8.881784197001246407E-16, 2.361472542561082612E-16, -1.000000000000000000 ) ) ;
#16479 = ORIENTED_EDGE ( 'NONE', *, *, #13158, .F. ) ;
#16480 = CARTESIAN_POINT ( 'NONE',  ( 0.4741640079579751421, -1.162838329081267830, -0.4122610257295771796 ) ) ;
#16481 = CARTESIAN_POINT ( 'NONE',  ( -0.3000000000000000999, -2.003129936916423048, -0.4197911229995844873 ) ) ;
#16482 = CARTESIAN_POINT ( 'NONE',  ( 0.1318168234680600626, -0.5697357792748470873, 0.2343947008844321500 ) ) ;
#16484 = EDGE_LOOP ( 'NONE', ( #28595, #11449, #37996, #21012 ) ) ;
#16483 = FACE_OUTER_BOUND ( 'NONE', #19772, .T. ) ;
#16486 = ORIENTED_EDGE ( 'NONE', *, *, #14806, .F. ) ;
#16485 = VERTEX_POINT ( 'NONE', #19344 ) ;
#16487 = DIRECTION ( 'NONE',  ( 0.000000000000000000, 0.000000000000000000, -1.000000000000000000 ) ) ;
#16488 = EDGE_CURVE ( 'NONE', #21610, #3320, #13143, .T. ) ;
#16489 = VERTEX_POINT ( 'NONE', #9455 ) ;
#16490 = ORIENTED_EDGE ( 'NONE', *, *, #3161, .F. ) ;
#16491 = PLANE ( 'NONE',  #1425 ) ;
#16492 = CARTESIAN_POINT ( 'NONE',  ( 0.000000000000000000, -0.05999999999999990757, 0.000000000000000000 ) ) ;
#16493 = SECURITY_CLASSIFICATION_LEVEL ( 'unclassified' ) ;
#16494 = EDGE_CURVE ( 'NONE', #7054, #2060, #7379, .T. ) ;
#16495 = CIRCLE ( 'NONE', #13860, 0.04000000000000000777 ) ;
#16496 = CARTESIAN_POINT ( 'NONE',  ( 0.002000609201561052118, -0.6339827964191878662, -0.01138449076159552854 ) ) ;
#16497 = ORIENTED_EDGE ( 'NONE', *, *, #35051, .T. ) ;
#16498 = EDGE_CURVE ( 'NONE', #3488, #5149, #26012, .T. ) ;
#16499 = CARTESIAN_POINT ( 'NONE',  ( 0.09914491568847688674, -0.8039099662830504478, 0.3344751936899787448 ) ) ;
#16500 = CARTESIAN_POINT ( 'NONE',  ( 0.3638878398920847301, -1.759885569913659964, -0.5002684421424647976 ) ) ;
#16501 = VECTOR ( 'NONE', #38446, 39.37007874015748143 ) ;
#16502 = CARTESIAN_POINT ( 'NONE',  ( 0.1151237624173331725, -0.5938742608929095113, 0.3101306348406044910 ) ) ;
#16503 = CARTESIAN_POINT ( 'NONE',  ( 0.6511295279640838540, -1.603372484741562243, -0.5770581850489380216 ) ) ;
#16504 = DIRECTION ( 'NONE',  ( 0.01455087615875041117, 0.9998941303973198913, 0.000000000000000000 ) ) ;
#16505 = CIRCLE ( 'NONE', #21772, 1.991674066779353769 ) ;
#16506 = CARTESIAN_POINT ( 'NONE',  ( -0.03654368633476864220, 0.08356155710620738475, 0.5047517311408972196 ) ) ;
#16507 = CIRCLE ( 'NONE', #36876, 0.03999999999999964001 ) ;
#16508 = B_SPLINE_CURVE_WITH_KNOTS ( 'NONE', 3,
 ( #4324, #29623, #1675, #32106 ),
 .UNSPECIFIED., .F., .F.,
 ( 4, 4 ),
 ( -6.000000000870814185E-08, 0.001836379686786120558 ),
 .UNSPECIFIED. ) ;
#16509 = CARTESIAN_POINT ( 'NONE',  ( 0.3498557339129456656, -1.754787963452209887, 0.5848441301335288722 ) ) ;
#16510 = CARTESIAN_POINT ( 'NONE',  ( 0.4399767927377957188, -1.641420014575965203, -0.3416704067942654133 ) ) ;
#16511 = B_SPLINE_CURVE_WITH_KNOTS ( 'NONE', 3,
 ( #28133, #40047, #21969, #3042 ),
 .UNSPECIFIED., .F., .F.,
 ( 4, 4 ),
 ( 0.000000000000000000, 0.0006205162911372014709 ),
 .UNSPECIFIED. ) ;
#16512 = CARTESIAN_POINT ( 'NONE',  ( 0.5455881031540377180, -1.595019605959082654, -0.5473203437262895710 ) ) ;
#16513 = CARTESIAN_POINT ( 'NONE',  ( 0.1927291533531542422, -0.7490955637697421787, 0.5554573830606346352 ) ) ;
#16514 = CARTESIAN_POINT ( 'NONE',  ( 3.250805436079486516E-05, -0.6542315385261258109, -0.1016538680321513732 ) ) ;
#16515 = EDGE_CURVE ( 'NONE', #23751, #30709, #40247, .T. ) ;
#16516 =( CONVERSION_BASED_UNIT ( 'INCH', #3156 ) LENGTH_UNIT ( ) NAMED_UNIT ( #32012 ) );
#16517 = CARTESIAN_POINT ( 'NONE',  ( 0.1436225252650951412, -1.283668529478381393, 0.4687417262808780127 ) ) ;
#16518 = CARTESIAN_POINT ( 'NONE',  ( 0.4480646913441768131, -1.099213350020603164, -0.6275147848854655264 ) ) ;
#16519 = CARTESIAN_POINT ( 'NONE',  ( 0.08097120591835743619, -1.368856899881548683, 0.5761801428003342496 ) ) ;
#16520 = CARTESIAN_POINT ( 'NONE',  ( 0.5123549971852071616, -1.116020584419624928, 0.5891410297636010540 ) ) ;
#16521 = APPROVAL_STATUS ( 'not_yet_approved' ) ;
#16522 = CARTESIAN_POINT ( 'NONE',  ( -0.02000000000000000042, -2.548345659627495596, -0.2263512047145338768 ) ) ;
#16523 = VECTOR ( 'NONE', #21322, 39.37007874015748143 ) ;
#16524 = DIRECTION ( 'NONE',  ( 0.4999999999999993894, 0.000000000000000000, -0.8660254037844390407 ) ) ;
#16525 = ADVANCED_FACE ( 'NONE', ( #33085 ), #17253, .T. ) ;
#16526 = CARTESIAN_POINT ( 'NONE',  ( 0.07882260269869785507, -1.330132293077975314, 0.5081289575126681779 ) ) ;
#16527 = CIRCLE ( 'NONE', #11913, 0.1000000000000000194 ) ;
#16528 = ORIENTED_EDGE ( 'NONE', *, *, #3117, .F. ) ;
#16529 = CARTESIAN_POINT ( 'NONE',  ( 0.4625308732612979923, -1.562160397472748707, 0.5754140938433903729 ) ) ;
#16530 = CARTESIAN_POINT ( 'NONE',  ( 0.06045346506656670837, 0.05436763897581790156, 0.1249999999999993477 ) ) ;
#16531 = CIRCLE ( 'NONE', #36231, 0.04000000000000000777 ) ;
#16532 = CARTESIAN_POINT ( 'NONE',  ( 0.1865761819245507769, -0.8562558704779227314, 0.1990025499142320520 ) ) ;
#16533 = ORIENTED_EDGE ( 'NONE', *, *, #2377, .F. ) ;
#16534 = DIRECTION ( 'NONE',  ( -1.000000000000000000, -0.000000000000000000, -0.000000000000000000 ) ) ;
#16535 = B_SPLINE_CURVE_WITH_KNOTS ( 'NONE', 3,
 ( #7499, #14089, #26663, #23577 ),
 .UNSPECIFIED., .F., .F.,
 ( 4, 4 ),
 ( 0.001814668777126959539, 0.002327282627751500917 ),
 .UNSPECIFIED. ) ;
#16536 = CARTESIAN_POINT ( 'NONE',  ( 0.6791962457086077043, -1.401251971513146621, 0.6322342638419099492 ) ) ;
#16538 = EDGE_LOOP ( 'NONE', ( #6416, #5897, #38046, #8235 ) ) ;
#16537 = ORIENTED_EDGE ( 'NONE', *, *, #29388, .F. ) ;
#16539 = DIRECTION ( 'NONE',  ( 1.000000000000000000, 0.000000000000000000, 0.000000000000000000 ) ) ;
#16540 = EDGE_LOOP ( 'NONE', ( #29924, #33511, #26412, #6329 ) ) ;
#16541 = CARTESIAN_POINT ( 'NONE',  ( 0.3620662970392556912, -1.757402016409378875, -0.5213949640471970959 ) ) ;
#16542 = CARTESIAN_POINT ( 'NONE',  ( 0.6022976011930347706, -1.482297354951358503, 0.5545281621470995459 ) ) ;
#16543 = EDGE_CURVE ( 'NONE', #243, #8849, #14690, .T. ) ;
#16544 = DIRECTION ( 'NONE',  ( 1.000000000000000000, -3.287861740168050473E-16, -8.266623803851098360E-16 ) ) ;
#16545 = VERTEX_POINT ( 'NONE', #20157 ) ;
#16546 = VECTOR ( 'NONE', #15947, 39.37007874015748854 ) ;
#16547 = FACE_OUTER_BOUND ( 'NONE', #8725, .T. ) ;
#16548 = CARTESIAN_POINT ( 'NONE',  ( 0.1955653942118278366, -0.8581851384218914802, 0.6256584387592237784 ) ) ;
#16549 = CARTESIAN_POINT ( 'NONE',  ( 0.01941772917732825440, -0.5190691814311400032, 0.4360231708482461555 ) ) ;
#16550 = CARTESIAN_POINT ( 'NONE',  ( 0.4698255749495779399, -1.558011031807577496, 0.5747976326119568213 ) ) ;
#16552 = DIRECTION ( 'NONE',  ( 0.000000000000000000, -6.829619984160655877E-15, -1.000000000000000000 ) ) ;
#16551 = CARTESIAN_POINT ( 'NONE',  ( 0.4829750487733310838, -1.628965326960139848, -0.4293328069181645001 ) ) ;
#16553 = FACE_OUTER_BOUND ( 'NONE', #21416, .T. ) ;
#16554 = ORIENTED_EDGE ( 'NONE', *, *, #26344, .F. ) ;
#16555 = AXIS2_PLACEMENT_3D ( 'NONE', #24877, #25065, #36995 ) ;
#16556 = CARTESIAN_POINT ( 'NONE',  ( 0.4584717390208090659, -1.703043547193806573, -0.5155029497116575543 ) ) ;
#16557 = CARTESIAN_POINT ( 'NONE',  ( 0.4380378120020821942, -1.691746349159306773, -0.5029009121720273701 ) ) ;
#16558 = CARTESIAN_POINT ( 'NONE',  ( -0.05078493045284266511, 0.2374933143169576932, -0.4099093267371657912 ) ) ;
#16559 = VECTOR ( 'NONE', #12447, 39.37007874015748143 ) ;
#16560 = FACE_OUTER_BOUND ( 'NONE', #24719, .T. ) ;
#16561 = ADVANCED_FACE ( 'NONE', ( #32873 ), #17462, .T. ) ;
#16562 = CIRCLE ( 'NONE', #27082, 0.02999999999999996420 ) ;
#16563 = APPLIED_DATE_AND_TIME_ASSIGNMENT ( #7213, #20204, ( #31348 ) ) ;
#16564 = FACE_OUTER_BOUND ( 'NONE', #22688, .T. ) ;
#16565 = EDGE_CURVE ( 'NONE', #6307, #15639, #38931, .T. ) ;
#16566 = CARTESIAN_POINT ( 'NONE',  ( 0.2019795930595086331, -0.6216091269244319317, 0.3384082674912240463 ) ) ;
#16567 = B_SPLINE_SURFACE_WITH_KNOTS ( 'NONE', 5, 5, ( 
 ( #22698, #32530, #1298, #26370, #704, #10521 ),
 ( #7030, #19598, #3935, #32132, #13409, #39121 ),
 ( #7419, #13199, #16707, #13615, #20399, #1495 ),
 ( #38903, #23509, #4536, #16496, #23091, #25985 ),
 ( #35618, #38510, #10338, #10730, #23303, #22901 ),
 ( #17307, #7828, #7214, #4139, #32321, #35828 ) ),
 .UNSPECIFIED., .F., .F., .F.,
 ( 6, 6 ),
 ( 6, 6 ),
 ( -6.761171338546692944, 6.761171338546684950 ),
 ( -2.171890115185114656, 4.589281223359888529 ),
 .UNSPECIFIED. ) ;
#16568 = EDGE_CURVE ( 'NONE', #34456, #33739, #30867, .T. ) ;
#16569 = DIRECTION ( 'NONE',  ( 0.000000000000000000, 0.000000000000000000, -1.000000000000000000 ) ) ;
#16570 = CARTESIAN_POINT ( 'NONE',  ( 0.6069176374591634948, -1.480164522464830990, 0.5706138896049881559 ) ) ;
#16571 = CARTESIAN_POINT ( 'NONE',  ( 0.04285427992853851203, 0.4878399728613546649, -0.08281491827193158961 ) ) ;
#16572 = CARTESIAN_POINT ( 'NONE',  ( 0.4949988758262525157, -1.646761950602083191, -0.6271208291453260752 ) ) ;
#16573 = CARTESIAN_POINT ( 'NONE',  ( 0.3527420388993543487, -1.124787755445947113, 0.7358831224922630643 ) ) ;
#16574 = LINE ( 'NONE', #32005, #15296 ) ;
#16575 = CARTESIAN_POINT ( 'NONE',  ( 0.1834925190845456133, -1.244183424859474307, -0.6222488774890111429 ) ) ;
#16576 = ORIENTED_EDGE ( 'NONE', *, *, #5674, .F. ) ;
#16577 = DIRECTION ( 'NONE',  ( -0.000000000000000000, 0.3807313408632033713, 0.9246857012436752177 ) ) ;
#16578 = CARTESIAN_POINT ( 'NONE',  ( 0.09723417313752830138, -0.6135477923982464166, 0.3092590504431999565 ) ) ;
#16579 = CIRCLE ( 'NONE', #21853, 0.1700000000000000400 ) ;
#16580 = DIRECTION ( 'NONE',  ( -1.000000000000000000, -0.000000000000000000, -0.000000000000000000 ) ) ;
#16581 = CARTESIAN_POINT ( 'NONE',  ( -0.05464101615137773038, -1.599201040860868339, 0.2442182323853691606 ) ) ;
#16582 = CARTESIAN_POINT ( 'NONE',  ( 0.1002847947475375562, -0.9216047912797521446, 0.6044655177918580868 ) ) ;
#16583 = VERTEX_POINT ( 'NONE', #13570 ) ;
#16584 = CARTESIAN_POINT ( 'NONE',  ( -0.1529745177444770954, 0.4738847129974458894, 0.3606502365071836969 ) ) ;
#16585 = AXIS2_PLACEMENT_3D ( 'NONE', #29, #12517, #3467 ) ;
#16586 = CIRCLE ( 'NONE', #6058, 0.1033070866141732880 ) ;
#16587 = DIRECTION ( 'NONE',  ( -1.000000000000000000, -7.857794173099924470E-32, -8.628166150854818811E-32 ) ) ;
#16588 = CARTESIAN_POINT ( 'NONE',  ( 0.4645646215180628258, -1.672710978628429102, 0.4491217904219667045 ) ) ;
#16589 = CARTESIAN_POINT ( 'NONE',  ( -2.112273405726188513E-14, -2.183180860297921466, -0.2737760292030870235 ) ) ;
#16590 = CARTESIAN_POINT ( 'NONE',  ( 0.4534472899590196726, -1.218434779631715204, 0.6820681023121225595 ) ) ;
#16591 = ADVANCED_FACE ( 'NONE', ( #10469 ), #1521, .T. ) ;
#16592 = EDGE_CURVE ( 'NONE', #5913, #2376, #15949, .T. ) ;
#16594 = CARTESIAN_POINT ( 'NONE',  ( 0.3177287329960665208, -1.760453033344018703, 0.4998481136542969883 ) ) ;
#16593 = FACE_OUTER_BOUND ( 'NONE', #28315, .T. ) ;
#16595 = CARTESIAN_POINT ( 'NONE',  ( 0.4922096163030106331, -1.082311226180449504, 0.5799505941865350511 ) ) ;
#16596 = ORIENTED_EDGE ( 'NONE', *, *, #28518, .F. ) ;
#16597 = CARTESIAN_POINT ( 'NONE',  ( 0.06448306067890459403, -1.151813066880623015, 0.7546316310809547678 ) ) ;
#16598 = ORIENTED_EDGE ( 'NONE', *, *, #28755, .T. ) ;
#16599 = CARTESIAN_POINT ( 'NONE',  ( 0.4137764936004748595, -1.589585228628171532, 0.5759508131641624118 ) ) ;
#16601 = CARTESIAN_POINT ( 'NONE',  ( 0.1987655437495040311, -0.5941059772690211460, 0.3236942554273257722 ) ) ;
#16600 = DIRECTION ( 'NONE',  ( 0.000000000000000000, 0.000000000000000000, -1.000000000000000000 ) ) ;
#16602 = CARTESIAN_POINT ( 'NONE',  ( -1.019575837292303166, -0.04310840302197994911, 0.3599999999999993205 ) ) ;
#16603 = VERTEX_POINT ( 'NONE', #39061 ) ;
#16604 = CARTESIAN_POINT ( 'NONE',  ( -0.1206014988277990946, -0.5041571071311168328, 0.1364167062886329496 ) ) ;
#16605 = CARTESIAN_POINT ( 'NONE',  ( 0.5258573571825243542, -1.427028965149156114, 0.7758776250953042242 ) ) ;
#16606 = ORIENTED_EDGE ( 'NONE', *, *, #6121, .T. ) ;
#16607 = CARTESIAN_POINT ( 'NONE',  ( 0.07497864282573103722, -1.322056043867067876, 0.4862695133534068459 ) ) ;
#16608 = CARTESIAN_POINT ( 'NONE',  ( 0.08083978255789368850, -1.392018123601084456, -0.3662540681622217242 ) ) ;
#16609 = CARTESIAN_POINT ( 'NONE',  ( 0.3409152363046956680, -1.516880185093671951, -0.7462941026102620778 ) ) ;
#16610 = CARTESIAN_POINT ( 'NONE',  ( -0.02000000000000000042, -1.723343441215260619, -0.2604803408413784993 ) ) ;
#16611 = TOROIDAL_SURFACE ( 'NONE', #17886, 0.04500000000000032446, 0.01499999999999999944 ) ;
#16612 = CARTESIAN_POINT ( 'NONE',  ( 0.1614670899430008522, -0.7569536277469717245, 0.1022936816274460647 ) ) ;
#16613 = CARTESIAN_POINT ( 'NONE',  ( 0.3760351885562613350, -1.762179279381401731, -0.5696997652324998773 ) ) ;
#16614 = B_SPLINE_CURVE_WITH_KNOTS ( 'NONE', 3,
 ( #674, #38261, #22061, #34583 ),
 .UNSPECIFIED., .F., .F.,
 ( 4, 4 ),
 ( -6.000000000230091993E-08, 0.001780663706559377666 ),
 .UNSPECIFIED. ) ;
#16615 = CARTESIAN_POINT ( 'NONE',  ( 0.5640992009001688512, -1.512213347522166185, 0.5182417262812423209 ) ) ;
#16616 = AXIS2_PLACEMENT_3D ( 'NONE', #10259, #22825, #35345 ) ;
#16617 = CARTESIAN_POINT ( 'NONE',  ( 0.3871590699894606469, -1.829451072714431525, -0.6982937763513055174 ) ) ;
#16618 = CIRCLE ( 'NONE', #8059, 0.1000000000000000194 ) ;
#16619 = CARTESIAN_POINT ( 'NONE',  ( 0.7002079545642244662, -1.577973572399679725, 0.5182417262812423209 ) ) ;
#16620 = CARTESIAN_POINT ( 'NONE',  ( 0.1943567346968996801, -1.255085851118643125, -0.7153666112938226185 ) ) ;
#16621 = COORDINATED_UNIVERSAL_TIME_OFFSET ( 0, 0, .AHEAD. ) ;
#16622 = AXIS2_PLACEMENT_3D ( 'NONE', #7978, #11281, #23848 ) ;
#16623 = ADVANCED_FACE ( 'NONE', ( #23461 ), #35562, .T. ) ;
#16624 = CARTESIAN_POINT ( 'NONE',  ( 0.6637426744281501589, -1.463151821187066437, -0.6174834252971218573 ) ) ;
#16625 = CARTESIAN_POINT ( 'NONE',  ( 0.03674078017396109619, 0.2486088097086621151, 0.4115158447297205258 ) ) ;
#16626 = DIRECTION ( 'NONE',  ( 1.000000000000000000, 0.000000000000000000, 0.000000000000000000 ) ) ;
#16627 = DIRECTION ( 'NONE',  ( 1.000000000000000000, 2.341930812374887555E-31, -1.664003471950578127E-31 ) ) ;
#16628 = CARTESIAN_POINT ( 'NONE',  ( 0.000000000000000000, 0.5632502439596359656, -0.2139757610878384453 ) ) ;
#16629 = AXIS2_PLACEMENT_3D ( 'NONE', #24312, #27595, #30880 ) ;
#16630 = CARTESIAN_POINT ( 'NONE',  ( 0.07582666994630285484, -1.068917391567854036, 0.8049195030047635591 ) ) ;
#16631 = CARTESIAN_POINT ( 'NONE',  ( -0.0003059967544939336411, -0.9037512443581188215, 0.02100609841003503453 ) ) ;
#16632 = DIRECTION ( 'NONE',  ( 0.000000000000000000, 3.330669073875470114E-16, 1.000000000000000000 ) ) ;
#16633 = CARTESIAN_POINT ( 'NONE',  ( 0.4209912206648682154, -1.078067379053157193, -0.5155029497116575543 ) ) ;
#16634 = DIRECTION ( 'NONE',  ( -1.000000000000000000, -0.000000000000000000, -0.000000000000000000 ) ) ;
#16635 = APPLICATION_CONTEXT ( 'configuration controlled 3d designs of mechanical parts and assemblies' ) ;
#16636 = ORIENTED_EDGE ( 'NONE', *, *, #40075, .T. ) ;
#16637 = VERTEX_POINT ( 'NONE', #14166 ) ;
#16638 = DIRECTION ( 'NONE',  ( 0.9998941247116546194, -0.01455087607601020412, 0.0001066420868422379362 ) ) ;
#16639 = ORIENTED_EDGE ( 'NONE', *, *, #25219, .F. ) ;
#16640 = CARTESIAN_POINT ( 'NONE',  ( -0.03868264068766702479, -0.03360988006411878837, 0.4753775160315156789 ) ) ;
#16641 = DIRECTION ( 'NONE',  ( 0.9766636885342073748, -0.2147743920926257488, 0.000000000000000000 ) ) ;
#16642 = CIRCLE ( 'NONE', #26484, 0.06819284191469469902 ) ;
#16643 = CARTESIAN_POINT ( 'NONE',  ( 0.4981282648377903244, -1.293502761169403881, 0.7428242663174567939 ) ) ;
#16645 = ORIENTED_EDGE ( 'NONE', *, *, #29833, .T. ) ;
#16644 = DIRECTION ( 'NONE',  ( 0.000000000000000000, 0.000000000000000000, -1.000000000000000000 ) ) ;
#16646 = CARTESIAN_POINT ( 'NONE',  ( 0.5416676161616581497, -1.167047932790743037, 0.6420073683128293407 ) ) ;
#16647 = CARTESIAN_POINT ( 'NONE',  ( 0.3466435857699784462, -1.701529685981289175, -0.5540514338380616577 ) ) ;
#16648 = ORIENTED_EDGE ( 'NONE', *, *, #30591, .T. ) ;
#16649 = CARTESIAN_POINT ( 'NONE',  ( 0.2031820619477883449, -0.6660346396928469304, 0.3462152820027419864 ) ) ;
#16650 = AXIS2_PLACEMENT_3D ( 'NONE', #17829, #30598, #21353 ) ;
#16651 = ORIENTED_EDGE ( 'NONE', *, *, #9733, .F. ) ;
#16652 = AXIS2_PLACEMENT_3D ( 'NONE', #35357, #10871, #20335 ) ;
#16653 = CARTESIAN_POINT ( 'NONE',  ( 0.2817677660706678910, -1.487235381464147910, 0.8882017575617421334 ) ) ;
#16655 = CARTESIAN_POINT ( 'NONE',  ( 0.1734973056165642902, -1.209394307038482719, -0.5155029497116575543 ) ) ;
#16654 = CARTESIAN_POINT ( 'NONE',  ( 0.5348150208694708585, -1.670518664781361240, -0.4558810860387588759 ) ) ;
#16656 = CARTESIAN_POINT ( 'NONE',  ( 0.3088664963667261398, -1.757905065063135597, 0.5295467280985148850 ) ) ;
#16657 = CARTESIAN_POINT ( 'NONE',  ( 0.0005464815904230041358, -1.956929671832038808, -0.3304605512727917804 ) ) ;
#16658 = EDGE_LOOP ( 'NONE', ( #27402, #6508, #9324 ) ) ;
#16659 = LINE ( 'NONE', #32481, #31650 ) ;
#16660 = CARTESIAN_POINT ( 'NONE',  ( 0.2362093653773955082, -0.9997838659200906086, 0.5753361218662520482 ) ) ;
#16661 = AXIS2_PLACEMENT_3D ( 'NONE', #20327, #7952, #29990 ) ;
#16662 = CARTESIAN_POINT ( 'NONE',  ( -0.02231181081520831194, 0.07006449514257646893, -0.5077922075898729792 ) ) ;
#16663 = CARTESIAN_POINT ( 'NONE',  ( 0.6076235955870944450, -1.477448194379718194, 0.6267975502367186813 ) ) ;
#16664 = AXIS2_PLACEMENT_3D ( 'NONE', #19048, #9982, #25837 ) ;
#16665 = CARTESIAN_POINT ( 'NONE',  ( 0.1627620917790547350, -0.9015321819263497627, 0.5877156909771449333 ) ) ;
#16666 = CARTESIAN_POINT ( 'NONE',  ( 0.4867251962510119045, -1.680960026995096612, -0.6125153944539966089 ) ) ;
#16667 = CARTESIAN_POINT ( 'NONE',  ( 0.4410077156479240146, -1.144291324537809462, 0.4235185031147128409 ) ) ;
#16668 = CARTESIAN_POINT ( 'NONE',  ( -0.1508021419688953257, 0.4665171419162804645, 0.3606502365330822579 ) ) ;
#16669 = DIRECTION ( 'NONE',  ( 1.000000000000000000, -0.000000000000000000, -0.000000000000000000 ) ) ;
#16670 = CARTESIAN_POINT ( 'NONE',  ( 0.6335034399251443515, -1.559158136585290233, 0.4182417262808776903 ) ) ;
#16671 = CARTESIAN_POINT ( 'NONE',  ( 0.01548846960707309615, -0.3772621329473452301, 0.3651003739302747242 ) ) ;
#16672 = AXIS2_PLACEMENT_3D ( 'NONE', #25809, #22519, #35446 ) ;
#16673 = CARTESIAN_POINT ( 'NONE',  ( 0.03301162916268218783, -0.3732432789822014985, 0.3635092914618219262 ) ) ;
#16674 = ADVANCED_FACE ( 'NONE', ( #23036 ), #15300, .F. ) ;
#16675 = EDGE_CURVE ( 'NONE', #28193, #3229, #12012, .T. ) ;
#16676 = DIRECTION ( 'NONE',  ( 0.2637677594038911888, 0.000000000000000000, -0.9645862165193171966 ) ) ;
#16677 = CARTESIAN_POINT ( 'NONE',  ( 0.2262803116713057172, -1.604565100197093308, -0.6672799576086320128 ) ) ;
#16678 = CIRCLE ( 'NONE', #25891, 0.009999999999999930819 ) ;
#16679 = PRODUCT_DEFINITION_SHAPE ( 'NONE', 'NONE',  #38779 ) ;
#16680 = CARTESIAN_POINT ( 'NONE',  ( 0.4311296713360665001, -1.704400165977600468, 0.4305790789625640880 ) ) ;
#16681 = CARTESIAN_POINT ( 'NONE',  ( 0.3613318213999966999, -1.782164263199393694, -0.6704317764855626249 ) ) ;
#16682 = ADVANCED_FACE ( 'NONE', ( #36168 ), #30429, .F. ) ;
#16683 = CARTESIAN_POINT ( 'NONE',  ( 0.3026265312661224893, -1.684849445872222296, 0.8620389816118222415 ) ) ;
#16684 = CARTESIAN_POINT ( 'NONE',  ( 0.7072999403808241103, -1.506214808821535023, 0.5537687555486060509 ) ) ;
#16685 = EDGE_CURVE ( 'NONE', #24957, #24018, #34790, .T. ) ;
#16686 = CIRCLE ( 'NONE', #31168, 0.06250000000000001388 ) ;
#16687 = CIRCLE ( 'NONE', #291, 0.01499999999999998904 ) ;
#16688 = ORIENTED_EDGE ( 'NONE', *, *, #3438, .T. ) ;
#16689 = CYLINDRICAL_SURFACE ( 'NONE', #26951, 0.08000000000000002942 ) ;
#16690 = EDGE_LOOP ( 'NONE', ( #26574, #5327, #33094, #31334 ) ) ;
#16691 = CARTESIAN_POINT ( 'NONE',  ( 0.2626259013267802644, -1.679529066113947700, 0.6053279492784264804 ) ) ;
#16692 = CARTESIAN_POINT ( 'NONE',  ( 0.2816542641881043529, -0.9456696404293912783, 0.7252052400065256421 ) ) ;
#16694 = EDGE_LOOP ( 'NONE', ( #37943, #26771, #27679, #40525 ) ) ;
#16693 = CARTESIAN_POINT ( 'NONE',  ( -0.01548846960707524721, 0.000000000000000000, 0.000000000000000000 ) ) ;
#16696 = ORIENTED_EDGE ( 'NONE', *, *, #23188, .F. ) ;
#16695 = ORIENTED_EDGE ( 'NONE', *, *, #11938, .F. ) ;
#16697 = ADVANCED_BREP_SHAPE_REPRESENTATION ( '', ( #18435, #27819 ), #12683 ) ;
#16698 = CARTESIAN_POINT ( 'NONE',  ( 0.6641929375487872766, -1.545761309749121848, 0.6885940231374464426 ) ) ;
#16699 =( BOUNDED_SURFACE ( )  B_SPLINE_SURFACE ( 3, 2, ( 
 ( #29986, #1820, #40452 ),
 ( #15750, #21346, #18035 ),
 ( #15142, #34069, #15356 ),
 ( #30984, #27703, #27914 ),
 ( #2807, #30785, #12277 ),
 ( #24835, #21549, #37357 ),
 ( #9169, #21733, #168 ),
 ( #34267, #6075, #11854 ),
 ( #33883, #24420, #28299 ),
 ( #18645, #27505, #25016 ),
 ( #31205, #37767, #40235 ),
 ( #12072, #6290, #3022 ),
 ( #2605, #12658, #36951 ),
 ( #22165, #34679, #30590 ),
 ( #25223, #21952, #15567 ),
 ( #24635, #8770, #2414 ),
 ( #5870, #9586, #14952 ),
 ( #28114, #12461, #37165 ),
 ( #5685, #8979, #34479 ),
 ( #40645, #40030, #18430 ),
 ( #37548, #9370, #18863 ),
 ( #31403, #3205, #18241 ) ),
 .UNSPECIFIED., .F., .F., .T. ) 
 B_SPLINE_SURFACE_WITH_KNOTS ( ( 4, 2, 2, 2, 2, 2, 2, 2, 2, 2, 4 ),
 ( 3, 3 ),
 ( 0.002013519961495849157, 0.002780892266055757373, 0.003548264570615666021, 0.004315636875175574670, 0.004699323027455529211, 0.005083009179735482885, 0.005466695332015436559, 0.005850381484295391100, 0.006617753788855299316, 0.007385126093415207531, 0.008152498397975115746 ),
 ( 0.000000000000000000, 1.000000000000000000 ),
 .UNSPECIFIED. ) 
 GEOMETRIC_REPRESENTATION_ITEM ( )  RATIONAL_B_SPLINE_SURFACE ( (
 ( 1.000000000000000000, 0.7283825911960390975, 1.000000000000000000),
 ( 1.000000000000000000, 0.7404375345927893814, 1.000000000000000000),
 ( 1.000000000000000000, 0.7521483142434828295, 1.000000000000000000),
 ( 1.000000000000000000, 0.7744460733777598360, 1.000000000000000000),
 ( 1.000000000000000000, 0.7845612039380338576, 1.000000000000000000),
 ( 1.000000000000000000, 0.8022035258263804369, 1.000000000000000000),
 ( 1.000000000000000000, 0.8093965293320565246, 1.000000000000000000),
 ( 1.000000000000000000, 0.8169028692726039154, 1.000000000000000000),
 ( 1.000000000000000000, 0.8188329634863094064, 1.000000000000000000),
 ( 1.000000000000000000, 0.8214004505364274067, 1.000000000000000000),
 ( 1.000000000000000000, 0.8220602406260869577, 1.000000000000000000),
 ( 1.000000000000000000, 0.8220736605435746691, 1.000000000000000000),
 ( 1.000000000000000000, 0.8214126668415572263, 1.000000000000000000),
 ( 1.000000000000000000, 0.8188520474558432793, 1.000000000000000000),
 ( 1.000000000000000000, 0.8169545908333754047, 1.000000000000000000),
 ( 1.000000000000000000, 0.8094771004220963073, 1.000000000000000000),
 ( 1.000000000000000000, 0.8022723753809752889, 1.000000000000000000),
 ( 1.000000000000000000, 0.7845733350635248904, 1.000000000000000000),
 ( 1.000000000000000000, 0.7744472902494010658, 1.000000000000000000),
 ( 1.000000000000000000, 0.7522916829162722419, 1.000000000000000000),
 ( 1.000000000000000000, 0.7403553004666372228, 1.000000000000000000),
 ( 1.000000000000000000, 0.7283825911960403188, 1.000000000000000000) ) ) 
 REPRESENTATION_ITEM ( '' )  SURFACE ( )  );
#16700 = EDGE_LOOP ( 'NONE', ( #16606, #17087, #23943, #9897 ) ) ;
#16701 = EDGE_CURVE ( 'NONE', #32303, #32272, #10717, .T. ) ;
#16702 = CARTESIAN_POINT ( 'NONE',  ( -0.01061162201870326748, -0.5808848742743736304, 0.3378471357688186960 ) ) ;
#16703 = APPLIED_PERSON_AND_ORGANIZATION_ASSIGNMENT ( #19081, #3050, ( #22077 ) ) ;
#16704 = DIRECTION ( 'NONE',  ( -7.000205099780314469E-17, -1.000000000000000000, 6.590151126658399604E-16 ) ) ;
#16705 = PERSON_AND_ORGANIZATION ( #3929, #9632 ) ;
#16706 = TOROIDAL_SURFACE ( 'NONE', #17343, 1.971674066779348866, 0.02999999999999999889 ) ;
#16707 = CARTESIAN_POINT ( 'NONE',  ( -0.002842236103788325745, -0.7404579356088996089, 0.04185307883324737577 ) ) ;
#16708 = VERTEX_POINT ( 'NONE', #6460 ) ;
#16709 = CARTESIAN_POINT ( 'NONE',  ( 0.2612906772968546787, -0.9851395584723477983, 0.6798953947484819293 ) ) ;
#16710 = VECTOR ( 'NONE', #35308, 39.37007874015748143 ) ;
#16711 = CARTESIAN_POINT ( 'NONE',  ( 0.06927010083464776868, -0.5404361519564938598, 0.1579025348389868078 ) ) ;
#16712 = AXIS2_PLACEMENT_3D ( 'NONE', #18886, #38387, #7107 ) ;
#16713 = CARTESIAN_POINT ( 'NONE',  ( 0.5335437526992924395, -1.503445527284964500, 0.6930812907888218577 ) ) ;
#16714 = EDGE_LOOP ( 'NONE', ( #17508, #32775, #9701, #31930 ) ) ;
#16715 = LINE ( 'NONE', #7430, #15144 ) ;
#16716 = CYLINDRICAL_SURFACE ( 'NONE', #10650, 0.1033070866141732880 ) ;
#16717 = APPROVAL_PERSON_ORGANIZATION ( #25130, #27757, #6195 ) ;
#16718 = CARTESIAN_POINT ( 'NONE',  ( 0.6786717105919251036, -1.448527022901674233, 0.4644334021538232826 ) ) ;
#16719 = DIRECTION ( 'NONE',  ( 1.000000000000000000, 0.000000000000000000, 0.000000000000000000 ) ) ;
#16720 = TOROIDAL_SURFACE ( 'NONE', #4222, 0.5250000000000000222, 0.01499999999999999944 ) ;
#16721 = FACE_OUTER_BOUND ( 'NONE', #16953, .T. ) ;
#16722 = CARTESIAN_POINT ( 'NONE',  ( -0.01548846960707477016, 0.2306506793134060762, 0.4716198300880319882 ) ) ;
#16723 = CARTESIAN_POINT ( 'NONE',  ( 0.3480859549341126513, -1.062997586067646827, 0.7846658571238425139 ) ) ;
#16724 = AXIS2_PLACEMENT_3D ( 'NONE', #22112, #34634, #13221 ) ;
#16725 = CARTESIAN_POINT ( 'NONE',  ( -0.0003596754992817568900, -0.9247255903860709392, 0.06913601831629608008 ) ) ;
#16726 = CARTESIAN_POINT ( 'NONE',  ( 0.06928988850528894350, -0.5407624024163444343, 0.1615399141407840300 ) ) ;
#16727 = CARTESIAN_POINT ( 'NONE',  ( 0.006645421451714178529, -0.8246033869726616672, 0.06648983423800172710 ) ) ;
#16728 = CARTESIAN_POINT ( 'NONE',  ( 0.4634865284762402782, -1.134362257022321518, -0.3648515278348755109 ) ) ;
#16729 = EDGE_CURVE ( 'NONE', #40221, #23093, #30327, .T. ) ;
#16730 = CARTESIAN_POINT ( 'NONE',  ( 0.004566372195762857279, -0.8656213538948328567, 0.4622093217984943880 ) ) ;
#16731 = CARTESIAN_POINT ( 'NONE',  ( 0.4929465528686921560, -1.082715557938388029, 0.5685663778595840823 ) ) ;
#16732 = EDGE_CURVE ( 'NONE', #1802, #25148, #12673, .T. ) ;
#16733 = COORDINATED_UNIVERSAL_TIME_OFFSET ( 0, 0, .AHEAD. ) ;
#16734 = EDGE_CURVE ( 'NONE', #33009, #16401, #5346, .T. ) ;
#16735 = CIRCLE ( 'NONE', #39720, 0.01000000000000002970 ) ;
#16736 = DIRECTION ( 'NONE',  ( 0.000000000000000000, -0.8438867430782093226, -0.5365213554527464845 ) ) ;
#16737 = EDGE_CURVE ( 'NONE', #2772, #13785, #2084, .T. ) ;
#16738 = DIRECTION ( 'NONE',  ( 1.000000000000000000, 1.450080480853946466E-15, -8.881784197001242463E-16 ) ) ;
#16739 = CIRCLE ( 'NONE', #28576, 0.01000000000000003143 ) ;
#16740 = AXIS2_PLACEMENT_3D ( 'NONE', #23249, #9861, #7166 ) ;
#16741 = ORIENTED_EDGE ( 'NONE', *, *, #37649, .F. ) ;
#16742 = CARTESIAN_POINT ( 'NONE',  ( -0.1023754337098981698, 0.06118878220587095629, -0.07268054736755635847 ) ) ;
#16743 = APPLIED_APPROVAL_ASSIGNMENT ( #906, ( #33155 ) ) ;
#16744 = CARTESIAN_POINT ( 'NONE',  ( 0.002392601678638947398, -0.5315622534075540306, 0.1816553975050167746 ) ) ;
#16745 = DIRECTION ( 'NONE',  ( 1.000000000000000000, 0.000000000000000000, 0.000000000000000000 ) ) ;
#16746 = ORIENTED_EDGE ( 'NONE', *, *, #36869, .T. ) ;
#16747 = CARTESIAN_POINT ( 'NONE',  ( 0.5432023227565030421, -1.654074096829117879, -0.4765337786301755418 ) ) ;
#16748 = AXIS2_PLACEMENT_3D ( 'NONE', #7129, #19697, #16827 ) ;
#16749 = CARTESIAN_POINT ( 'NONE',  ( 0.6809224168725948045, -1.405736369044236378, 0.6042223006942389896 ) ) ;
#16751 = ORIENTED_EDGE ( 'NONE', *, *, #7469, .F. ) ;
#16750 = VERTEX_POINT ( 'NONE', #27344 ) ;
#16752 = DIRECTION ( 'NONE',  ( -7.771561172376107616E-16, 7.170354002788761615E-17, -1.000000000000000000 ) ) ;
#16753 = ORIENTED_EDGE ( 'NONE', *, *, #23245, .F. ) ;
#16754 = CARTESIAN_POINT ( 'NONE',  ( 0.3569144835062229015, -1.786313658517578951, -0.4887759019995990273 ) ) ;
#16755 = EDGE_CURVE ( 'NONE', #1932, #5913, #35744, .T. ) ;
#16756 = SPHERICAL_SURFACE ( 'NONE', #3568, 0.01499999999999999944 ) ;
#16757 = DIRECTION ( 'NONE',  ( 0.000000000000000000, 0.000000000000000000, -1.000000000000000000 ) ) ;
#16758 = ORIENTED_EDGE ( 'NONE', *, *, #20803, .T. ) ;
#16759 = CARTESIAN_POINT ( 'NONE',  ( -0.2399999999999999079, -3.811657270145150989, -0.1642545796697100491 ) ) ;
#16760 = CARTESIAN_POINT ( 'NONE',  ( 0.09446234534901919166, -0.6589171955595342078, 0.2802060902332455528 ) ) ;
#16761 = CARTESIAN_POINT ( 'NONE',  ( 0.1037934690335643728, -0.9534350347034203921, 0.9068416015443596656 ) ) ;
#16762 = CARTESIAN_POINT ( 'NONE',  ( 0.09694864982818704457, -0.6210372448765658637, 0.3796554584802787624 ) ) ;
#16764 = DIRECTION ( 'NONE',  ( -8.881784197001246407E-16, 2.361472542561082612E-16, -1.000000000000000000 ) ) ;
#16763 = CARTESIAN_POINT ( 'NONE',  ( 0.2665433607519571702, -1.687828102416362830, 0.5925423054000314993 ) ) ;
#16765 = CARTESIAN_POINT ( 'NONE',  ( 0.2764337282391635120, -1.207704344519197504, 0.5682417262808777680 ) ) ;
#16766 = ORIENTED_EDGE ( 'NONE', *, *, #10133, .F. ) ;
#16767 = EDGE_LOOP ( 'NONE', ( #11880, #19144, #21586, #7525 ) ) ;
#16768 = VECTOR ( 'NONE', #38460, 39.37007874015748854 ) ;
#16769 = CARTESIAN_POINT ( 'NONE',  ( 0.3186278594696675404, -1.645101200862095325, 0.5280450199627192420 ) ) ;
#16770 = CARTESIAN_POINT ( 'NONE',  ( 0.2627070462085436264, -0.7490940406976871468, 0.5657688020081199642 ) ) ;
#16771 = CARTESIAN_POINT ( 'NONE',  ( -0.02872242845530537450, 0.2464193076120113624, -0.4721747535844844079 ) ) ;
#16772 = VECTOR ( 'NONE', #6849, 39.37007874015748143 ) ;
#16773 = APPLIED_APPROVAL_ASSIGNMENT ( #22019, ( #7563 ) ) ;
#16774 = CARTESIAN_POINT ( 'NONE',  ( -0.04762200653274385048, -0.4700406811250516514, -0.1075684398553596738 ) ) ;
#16775 = CARTESIAN_POINT ( 'NONE',  ( 0.08058916068514938857, -1.309220013881621680, 0.4727703015479236548 ) ) ;
#16776 = CIRCLE ( 'NONE', #39760, 0.01499999999999999251 ) ;
#16777 = CARTESIAN_POINT ( 'NONE',  ( 0.1037539007929738771, -1.411184382869408616, 0.5260835464586457455 ) ) ;
#16778 = CARTESIAN_POINT ( 'NONE',  ( 0.3979743647030599130, -0.9582897341353557863, 0.7577590062044536889 ) ) ;
#16779 = EDGE_CURVE ( 'NONE', #32303, #7929, #19031, .T. ) ;
#16780 = CARTESIAN_POINT ( 'NONE',  ( 0.4019978477689601370, -1.758738184043603603, -0.4821875037442184819 ) ) ;
#16781 = CARTESIAN_POINT ( 'NONE',  ( 0.004845387396406415983, -0.8792891026250457820, 0.4619221541178868962 ) ) ;
#16782 = EDGE_CURVE ( 'NONE', #32375, #27977, #8582, .T. ) ;
#16783 = B_SPLINE_CURVE_WITH_KNOTS ( 'NONE', 3,
 ( #21163, #40061, #9020, #34103 ),
 .UNSPECIFIED., .F., .F.,
 ( 4, 4 ),
 ( 0.000000000000000000, 0.005247268741964242027 ),
 .UNSPECIFIED. ) ;
#16784 = CARTESIAN_POINT ( 'NONE',  ( 0.03647060353176048014, 0.5060729159580583669, -0.07645842516611377204 ) ) ;
#16785 = DIRECTION ( 'NONE',  ( 1.000000000000000000, 0.000000000000000000, 0.000000000000000000 ) ) ;
#16786 = VERTEX_POINT ( 'NONE', #33688 ) ;
#16787 = CARTESIAN_POINT ( 'NONE',  ( 0.2631241314290992395, -0.9694475436486175157, 0.6931444287947289284 ) ) ;
#16788 = CARTESIAN_POINT ( 'NONE',  ( 0.03159140494780099395, 0.05458666898339488427, 0.4890560705835249600 ) ) ;
#16789 = EDGE_CURVE ( 'NONE', #18610, #27000, #28481, .T. ) ;
#16790 = CARTESIAN_POINT ( 'NONE',  ( 0.4679778500672936992, -1.237826332153874942, 0.6057417262809768888 ) ) ;
#16791 = ORIENTED_EDGE ( 'NONE', *, *, #3885, .T. ) ;
#16792 = EDGE_CURVE ( 'NONE', #13556, #33386, #4832, .T. ) ;
#16793 = CARTESIAN_POINT ( 'NONE',  ( 0.4685502202651029569, -1.116536938686066183, 0.5688043585934901003 ) ) ;
#16794 = CARTESIAN_POINT ( 'NONE',  ( 0.5382177704477151270, -1.161136986456818176, 0.5551899235458804815 ) ) ;
#16795 = CARTESIAN_POINT ( 'NONE',  ( 0.3641524999503367721, -1.715784215955702852, -0.4585743496845985923 ) ) ;
#16796 = FACE_OUTER_BOUND ( 'NONE', #17612, .T. ) ;
#16797 = CARTESIAN_POINT ( 'NONE',  ( 0.06954336310279328470, -0.8599038886713844532, 0.4255655716258943122 ) ) ;
#16798 = ORIENTED_EDGE ( 'NONE', *, *, #28134, .F. ) ;
#16799 = CARTESIAN_POINT ( 'NONE',  ( -0.1617502512268847170, 0.4682890762661567896, 0.3382895567546961857 ) ) ;
#16800 = ADVANCED_FACE ( 'NONE', ( #16547 ), #4124, .F. ) ;
#16801 = DIRECTION ( 'NONE',  ( 7.771561172376107616E-16, -7.170354002788761615E-17, 1.000000000000000000 ) ) ;
#16802 = LOCAL_TIME ( 0, 53, 7.000000000000000000, #36262 ) ;
#16803 = CARTESIAN_POINT ( 'NONE',  ( -2.112273405726188513E-14, -2.097675824466503691, -0.2907077406111384099 ) ) ;
#16804 = ADVANCED_FACE ( 'NONE', ( #23142 ), #40251, .F. ) ;
#16805 = CARTESIAN_POINT ( 'NONE',  ( 0.03113248654051816583, 0.8492681979939306069, -0.2138253033704805295 ) ) ;
#16806 = CARTESIAN_POINT ( 'NONE',  ( 0.4561128394006527254, -1.223906212898765222, 0.6959908130051005726 ) ) ;
#16808 = DIRECTION ( 'NONE',  ( 8.881784197001246407E-16, -2.361472542561082612E-16, 1.000000000000000000 ) ) ;
#16807 = LINE ( 'NONE', #4830, #25257 ) ;
#16809 = CARTESIAN_POINT ( 'NONE',  ( 0.5714440434361192089, -1.545267987928362841, -0.5204514232545197627 ) ) ;
#16810 = ORIENTED_EDGE ( 'NONE', *, *, #32050, .T. ) ;
#16811 = ADVANCED_FACE ( 'NONE', ( #3592 ), #13058, .T. ) ;
#16812 = CIRCLE ( 'NONE', #3679, 0.01000000000000001756 ) ;
#16813 = CARTESIAN_POINT ( 'NONE',  ( -0.1515422989582873303, 0.4690188198402805986, 0.3602693336111430500 ) ) ;
#16814 = ORIENTED_EDGE ( 'NONE', *, *, #7022, .T. ) ;
#16815 = CARTESIAN_POINT ( 'NONE',  ( 0.4131346768878386144, -1.589365865636619191, 0.5663133035555527606 ) ) ;
#16817 = CARTESIAN_POINT ( 'NONE',  ( 0.2011461926870026229, -0.7184356070491879631, 0.3342384739243060010 ) ) ;
#16816 = CARTESIAN_POINT ( 'NONE',  ( 0.08593876023563185029, -0.8031142711107595034, 0.05926891841886761103 ) ) ;
#16818 = DIRECTION ( 'NONE',  ( 1.000000000000000000, 2.341930812374887555E-31, -1.664003471950578127E-31 ) ) ;
#16819 = ORIENTED_EDGE ( 'NONE', *, *, #15994, .F. ) ;
#16820 = ORIENTED_EDGE ( 'NONE', *, *, #29825, .F. ) ;
#16821 = CARTESIAN_POINT ( 'NONE',  ( -0.1999999999999997891, 0.5182417262804744906, 0.3749999999999995559 ) ) ;
#16822 = CARTESIAN_POINT ( 'NONE',  ( 0.5748457419294008552, -1.497445084182354114, 0.6198248605900839037 ) ) ;
#16823 = ORIENTED_EDGE ( 'NONE', *, *, #10258, .F. ) ;
#16824 = CARTESIAN_POINT ( 'NONE',  ( 0.4946724348411004057, -1.646204522746663956, -0.4040971505047686874 ) ) ;
#16825 = CARTESIAN_POINT ( 'NONE',  ( 0.02872242845530265445, -0.4768947642620242067, 0.2371557650701879294 ) ) ;
#16826 = CARTESIAN_POINT ( 'NONE',  ( 0.1856725227377205856, -0.8111418809926428386, 0.1833442776911899941 ) ) ;
#16827 = DIRECTION ( 'NONE',  ( 0.000000000000000000, 0.9343694307158671997, -0.3563057211773426602 ) ) ;
#16828 = B_SPLINE_CURVE_WITH_KNOTS ( 'NONE', 3,
 ( #27299, #39828, #21112, #5668, #20923, #18223, #2793, #21328, #36541, #36734, #11839, #5056 ),
 .UNSPECIFIED., .F., .F.,
 ( 4, 2, 2, 2, 2, 4 ),
 ( 3.088587339835645537E-17, 0.0003359336526506150403, 0.0006718673053011991808, 0.001343734610602367353, 0.002015601915903535418, 0.002687469221204703915 ),
 .UNSPECIFIED. ) ;
#16829 = DIRECTION ( 'NONE',  ( 1.000000000000000000, 0.000000000000000000, 0.000000000000000000 ) ) ;
#16830 = CIRCLE ( 'NONE', #39804, 0.1499999999999990785 ) ;
#16831 = AXIS2_PLACEMENT_3D ( 'NONE', #38922, #26392, #23326 ) ;
#16832 = B_SPLINE_CURVE_WITH_KNOTS ( 'NONE', 3,
 ( #21178, #26754, #30216, #14376, #36188, #24082, #36792, #30643, #39283, #8602 ),
 .UNSPECIFIED., .F., .F.,
 ( 4, 2, 2, 2, 4 ),
 ( 0.000000000000000000, 0.0004973432167690093435, 0.0009946864335380186870, 0.001492029650307028030, 0.001989372867076037374 ),
 .UNSPECIFIED. ) ;
#16833 = CARTESIAN_POINT ( 'NONE',  ( 0.6221473432577675489, -1.308691071842436493, 0.8644659521288400317 ) ) ;
#16834 = DIRECTION ( 'NONE',  ( -8.881784197001246407E-16, 2.361472542561082612E-16, -1.000000000000000000 ) ) ;
#16835 = CARTESIAN_POINT ( 'NONE',  ( -0.2666757540196698084, 0.4921670437878978843, 0.3749999999999990008 ) ) ;
#16836 = DATE_AND_TIME ( #13542, #20033 ) ;
#16837 = APPLIED_SECURITY_CLASSIFICATION_ASSIGNMENT ( #24074, ( #40652 ) ) ;
#16838 = ADVANCED_FACE ( 'NONE', ( #32980 ), #39771, .T. ) ;
#16839 = CARTESIAN_POINT ( 'NONE',  ( 0.6427025470096586757, -1.447461895507986762, -0.6319542925746485240 ) ) ;
#16840 = CARTESIAN_POINT ( 'NONE',  ( 0.03643058821097294731, 0.3645913838654474270, 0.3593578898915228415 ) ) ;
#16841 = DIRECTION ( 'NONE',  ( 0.000000000000000000, 0.000000000000000000, 1.000000000000000000 ) ) ;
#16842 = EDGE_CURVE ( 'NONE', #30237, #2983, #28368, .T. ) ;
#16843 = CARTESIAN_POINT ( 'NONE',  ( 0.2590277710115678755, -1.679485505736613149, 0.4634944759858370955 ) ) ;
#16844 = CIRCLE ( 'NONE', #18147, 0.01499999999999995955 ) ;
#16845 = CARTESIAN_POINT ( 'NONE',  ( 0.1252549559024136727, -1.296835781121829845, 0.4238276788641243131 ) ) ;
#16846 = CARTESIAN_POINT ( 'NONE',  ( 0.003124719664520433666, -0.5686731593868930013, 0.1115160683991335139 ) ) ;
#16847 = CARTESIAN_POINT ( 'NONE',  ( 0.5716576001687232456, -1.545079331453066418, -0.5060932645805602537 ) ) ;
#16848 = CARTESIAN_POINT ( 'NONE',  ( 0.4219866632171688225, -1.610104465087698777, -0.3647299066799567502 ) ) ;
#16849 = DIRECTION ( 'NONE',  ( -1.000000000000000000, -0.000000000000000000, -0.000000000000000000 ) ) ;
#16850 = CARTESIAN_POINT ( 'NONE',  ( -0.05186792262757310146, -0.2910804482542292959, 0.3700673534428200462 ) ) ;
#16851 = ORIENTED_EDGE ( 'NONE', *, *, #21749, .F. ) ;
#16852 = VERTEX_POINT ( 'NONE', #29700 ) ;
#16853 = CARTESIAN_POINT ( 'NONE',  ( 0.3666228249977095399, -1.767104007576765001, -0.5848508674883445835 ) ) ;
#16854 = ORIENTED_EDGE ( 'NONE', *, *, #1920, .F. ) ;
#16855 = LINE ( 'NONE', #29398, #768 ) ;
#16856 = CARTESIAN_POINT ( 'NONE',  ( 0.01548846960707528191, 0.2306506793134049660, -0.4716198300880325434 ) ) ;
#16857 = CARTESIAN_POINT ( 'NONE',  ( 0.4638821911974275181, -1.242580118564127645, 0.7881282199712437153 ) ) ;
#16859 = ORIENTED_EDGE ( 'NONE', *, *, #39388, .T. ) ;
#16858 = CARTESIAN_POINT ( 'NONE',  ( -0.2399999999999999079, -3.745280840418592661, 0.04438736989695814261 ) ) ;
#16860 = CARTESIAN_POINT ( 'NONE',  ( 0.4384178598954188155, -1.040563892421024983, 0.6900182345289431751 ) ) ;
#16861 = AXIS2_PLACEMENT_3D ( 'NONE', #28602, #15839, #10294 ) ;
#16862 = CARTESIAN_POINT ( 'NONE',  ( 0.1399722631084863167, -0.4537238383118586404, 0.1457373701026924706 ) ) ;
#16863 = EDGE_LOOP ( 'NONE', ( #15333, #7462, #35661, #29487 ) ) ;
#16864 = DIRECTION ( 'NONE',  ( 1.000000000000000000, 2.341930812374887555E-31, -1.664003471950578127E-31 ) ) ;
#16865 = CARTESIAN_POINT ( 'NONE',  ( 0.3276507143392576316, -1.639361389215603371, 0.5824061036618035647 ) ) ;
#16867 = CARTESIAN_POINT ( 'NONE',  ( 0.1131241454731939100, -0.6872203660140440151, -0.09530310615070609892 ) ) ;
#16866 = CARTESIAN_POINT ( 'NONE',  ( 0.6280878869109404183, -1.573568221354046281, 0.4189938828952650685 ) ) ;
#16868 = DIRECTION ( 'NONE',  ( -1.000000000000000000, -2.341930812374887555E-31, 1.664003471950578127E-31 ) ) ;
#16869 = CARTESIAN_POINT ( 'NONE',  ( 0.3623580354614820420, -1.967894635670391912, -0.4765942900942761740 ) ) ;
#16870 = CARTESIAN_POINT ( 'NONE',  ( 0.08756027987733720763, -1.379929391113575043, -0.3337043114794515097 ) ) ;
#16871 = ORIENTED_EDGE ( 'NONE', *, *, #32041, .T. ) ;
#16872 = CARTESIAN_POINT ( 'NONE',  ( 0.3211449588372387587, -1.297375842027792325, 0.4762509439642684250 ) ) ;
#16873 = CIRCLE ( 'NONE', #18842, 0.2149999999999999967 ) ;
#16874 = CARTESIAN_POINT ( 'NONE',  ( 0.1574420996541403550, -0.9545193198765702380, 0.4442515449357353763 ) ) ;
#16875 = DIRECTION ( 'NONE',  ( -1.000000000000000000, -0.000000000000000000, -0.000000000000000000 ) ) ;
#16876 = CARTESIAN_POINT ( 'NONE',  ( 0.02953079040095687308, 0.5250338024619264354, 0.07436286310882474215 ) ) ;
#16877 = CARTESIAN_POINT ( 'NONE',  ( 0.3838258328925114871, -1.260744394557325121, 0.5882158180126604297 ) ) ;
#16878 = CARTESIAN_POINT ( 'NONE',  ( 0.4642954988900184210, -1.156858560228702260, 0.4182417262808743597 ) ) ;
#16879 = FACE_OUTER_BOUND ( 'NONE', #22983, .T. ) ;
#16880 = CARTESIAN_POINT ( 'NONE',  ( -0.1212602504878787929, -0.5073146173917494339, 0.1528658435936968152 ) ) ;
#16881 = CARTESIAN_POINT ( 'NONE',  ( 0.04293701532779526514, 0.4875995331660214482, 0.08291810260646446940 ) ) ;
#16882 = CARTESIAN_POINT ( 'NONE',  ( 0.4480646913441768131, -1.099213350020603164, -0.6275147848854655264 ) ) ;
#16883 = CARTESIAN_POINT ( 'NONE',  ( 0.05999999999999990757, 0.6304109427692223822, -0.1442409525262416947 ) ) ;
#16884 =( CONVERSION_BASED_UNIT ( 'INCH', #32497 ) LENGTH_UNIT ( ) NAMED_UNIT ( #29672 ) );
#16885 = AXIS2_PLACEMENT_3D ( 'NONE', #39341, #11160, #1523 ) ;
#16886 = CARTESIAN_POINT ( 'NONE',  ( 0.04152565108029027119, -1.188198874194366761, 0.6784721777313348356 ) ) ;
#16887 = CARTESIAN_POINT ( 'NONE',  ( -0.3000000000000000999, -3.220869926774937664, -0.5656276768926112863 ) ) ;
#16888 = CARTESIAN_POINT ( 'NONE',  ( 0.1046051313612698097, -1.402039145303610734, 0.6143806765046105900 ) ) ;
#16889 = APPROVAL_PERSON_ORGANIZATION ( #9463, #38939, #22437 ) ;
#16890 = CARTESIAN_POINT ( 'NONE',  ( 0.4841487358689927634, -1.673745430023940717, 0.5182417262823179049 ) ) ;
#16891 = CARTESIAN_POINT ( 'NONE',  ( 0.3994067150627959029, -1.748687336150827276, -0.5749207012357768765 ) ) ;
#16892 = CARTESIAN_POINT ( 'NONE',  ( 0.3066092890089989198, -1.757470180272292959, 0.5913806063715120187 ) ) ;
#16893 = CARTESIAN_POINT ( 'NONE',  ( 0.7075884434940304946, -1.499667991049689952, 0.5400310817953950515 ) ) ;
#16894 = ORIENTED_EDGE ( 'NONE', *, *, #33510, .T. ) ;
#16895 = CARTESIAN_POINT ( 'NONE',  ( 0.1826337464091716545, -0.5596885952557434374, 0.2690888922271704176 ) ) ;
#16896 = ORIENTED_EDGE ( 'NONE', *, *, #820, .T. ) ;
#16897 = CARTESIAN_POINT ( 'NONE',  ( 0.2657064854856445724, -1.675227424430884238, 0.6641665367988364155 ) ) ;
#16898 = CARTESIAN_POINT ( 'NONE',  ( 0.6019823243568848126, -1.483134150572406940, 0.5732773657679698376 ) ) ;
#16901 = ORIENTED_EDGE ( 'NONE', *, *, #2257, .F. ) ;
#16900 = B_SPLINE_CURVE_WITH_KNOTS ( 'NONE', 3,
 ( #20305, #32825, #4631, #33038, #17207, #26693 ),
 .UNSPECIFIED., .F., .F.,
 ( 4, 2, 4 ),
 ( 2.660867628118834816, 5.798205611760163691, 8.935543595401492567 ),
 .UNSPECIFIED. ) ;
#16899 = CARTESIAN_POINT ( 'NONE',  ( 0.5128132487356600322, -1.640511253658597957, -0.4146624397426829089 ) ) ;
#16902 = B_SPLINE_CURVE_WITH_KNOTS ( 'NONE', 3,
 ( #29004, #35579, #36183, #39079, #35991, #26937, #36390, #2258, #7797, #4504 ),
 .UNSPECIFIED., .F., .F.,
 ( 4, 2, 2, 2, 4 ),
 ( 8.771195575407730871E-17, 0.0007834172717712188216, 0.001566834543542350040, 0.002350251815313481474, 0.003133669087084613343 ),
 .UNSPECIFIED. ) ;
#16904 = VERTEX_POINT ( 'NONE', #1544 ) ;
#16903 = ORIENTED_EDGE ( 'NONE', *, *, #14485, .T. ) ;
#16905 = CARTESIAN_POINT ( 'NONE',  ( 0.3114253368378466225, -1.187765832548442813, 0.5446703740600618016 ) ) ;
#16906 = VERTEX_POINT ( 'NONE', #11182 ) ;
#16907 = CARTESIAN_POINT ( 'NONE',  ( 0.06342771192242831202, -0.9335166984577768501, 0.7937027791328541415 ) ) ;
#16908 = CARTESIAN_POINT ( 'NONE',  ( -0.2300000000000002043, 0.5182417262804744906, 0.08500000000000018652 ) ) ;
#16909 = CARTESIAN_POINT ( 'NONE',  ( -0.08000000000000000167, -2.332630956013932888, -0.5701767140373721343 ) ) ;
#16910 = LINE ( 'NONE', #38292, #22477 ) ;
#16912 = ORIENTED_EDGE ( 'NONE', *, *, #11441, .F. ) ;
#16911 = VERTEX_POINT ( 'NONE', #14456 ) ;
#16913 = CARTESIAN_POINT ( 'NONE',  ( 0.2482514041270085792, -0.9705348356143717048, 0.6681873673986314932 ) ) ;
#16914 = CARTESIAN_POINT ( 'NONE',  ( 0.09015534308186123891, -0.5467265198224540157, 0.1782017856848721049 ) ) ;
#16915 = CARTESIAN_POINT ( 'NONE',  ( 0.5390489187139376748, -1.519039902820679133, 0.5725961793155519564 ) ) ;
#16916 = VERTEX_POINT ( 'NONE', #14065 ) ;
#16917 = CARTESIAN_POINT ( 'NONE',  ( 0.03360078502195575773, -1.082923033457784401, 0.6287642814980498596 ) ) ;
#16918 = FACE_OUTER_BOUND ( 'NONE', #10060, .T. ) ;
#16919 = CARTESIAN_POINT ( 'NONE',  ( -0.02953079040095652960, 0.09152108205202803826, 0.5223162075576412988 ) ) ;
#16920 = CARTESIAN_POINT ( 'NONE',  ( 0.3610463218409277197, -1.748328711707529459, 0.5952565890379123426 ) ) ;
#16921 = CARTESIAN_POINT ( 'NONE',  ( 0.4387252196728761433, -1.612896326537896829, -0.6609064949533233202 ) ) ;
#16922 = CARTESIAN_POINT ( 'NONE',  ( 0.5085763096842138564, -1.618730835354739828, -0.5737883394389590164 ) ) ;
#16923 = CARTESIAN_POINT ( 'NONE',  ( -0.3000000000000000999, -3.723902497147952406, 0.1004495357399106253 ) ) ;
#16924 = DIRECTION ( 'NONE',  ( 1.000000000000000000, 0.000000000000000000, 0.000000000000000000 ) ) ;
#16925 = CARTESIAN_POINT ( 'NONE',  ( 0.01170413314921280555, -0.7214729979845280194, -0.1114895720740121249 ) ) ;
#16926 = CARTESIAN_POINT ( 'NONE',  ( 0.5575849190334257743, -1.430655059094382731, 0.7536012745007747426 ) ) ;
#16927 = CARTESIAN_POINT ( 'NONE',  ( 0.4189043378923988925, -1.737431724743732753, -0.5872665585884508932 ) ) ;
#16928 = FACE_OUTER_BOUND ( 'NONE', #8428, .T. ) ;
#16929 = CARTESIAN_POINT ( 'NONE',  ( 0.1799043607419438529, -1.488798643046104875, 0.7589116457392215409 ) ) ;
#16930 = B_SPLINE_CURVE_WITH_KNOTS ( 'NONE', 3,
 ( #30799, #20751, #11476, #5080, #18048, #30603, #17832, #8173, #15156, #8376, #2226, #33899, #20533, #33067, #14963, #27518 ),
 .UNSPECIFIED., .F., .F.,
 ( 4, 2, 2, 2, 2, 2, 2, 4 ),
 ( 0.002977954013962045166, 0.003350115589110935245, 0.003722277164259825757, 0.004094438739408716270, 0.004466600314557606782, 0.004838761889706495560, 0.005210923464855384338, 0.005955246615153174036 ),
 .UNSPECIFIED. ) ;
#16931 = CARTESIAN_POINT ( 'NONE',  ( 0.2246580631734754474, -0.8968525156641222740, 0.4249663362035034364 ) ) ;
#16932 = COORDINATED_UNIVERSAL_TIME_OFFSET ( 0, 0, .AHEAD. ) ;
#16933 = EDGE_CURVE ( 'NONE', #3626, #3536, #26938, .T. ) ;
#16934 = APPLIED_PERSON_AND_ORGANIZATION_ASSIGNMENT ( #33801, #27236, ( #25389 ) ) ;
#16935 = CARTESIAN_POINT ( 'NONE',  ( -2.372745691485074626E-32, 5.828670879282072084E-17, 0.1749999999999999889 ) ) ;
#16936 = PLANE ( 'NONE',  #15354 ) ;
#16937 =( BOUNDED_SURFACE ( )  B_SPLINE_SURFACE ( 3, 2, ( 
 ( #20277, #38367, #32607 ),
 ( #26444, #29721, #7899 ),
 ( #23166, #32395, #10396 ),
 ( #1565, #33001, #29942 ),
 ( #7710, #22959, #4008 ),
 ( #39197, #13678, #10206 ),
 ( #1358, #4420, #32799 ),
 ( #26240, #32194, #7283 ),
 ( #22773, #35902, #35296 ),
 ( #16572, #38980, #16979 ),
 ( #4808, #10812, #977 ),
 ( #13492, #26057, #38577 ) ),
 .UNSPECIFIED., .F., .F., .F. ) 
 B_SPLINE_SURFACE_WITH_KNOTS ( ( 4, 2, 2, 2, 2, 4 ),
 ( 3, 3 ),
 ( 0.000000000000000000, 0.0009043136984160567724, 0.001356470547624085213, 0.001808627396832113545, 0.002712941095248170426, 0.003617254793664227090 ),
 ( 0.000000000000000000, 1.000000000000000000 ),
 .UNSPECIFIED. ) 
 GEOMETRIC_REPRESENTATION_ITEM ( )  RATIONAL_B_SPLINE_SURFACE ( (
 ( 1.000000000000000000, 0.7071067811865457964, 1.000000000000000000),
 ( 1.000000000000000000, 0.7141572841065146893, 1.000000000000000000),
 ( 1.000000000000000000, 0.7219308286147578801, 1.000000000000000000),
 ( 1.000000000000000000, 0.7336727792982185026, 1.000000000000000000),
 ( 1.000000000000000000, 0.7376634957069627685, 1.000000000000000000),
 ( 1.000000000000000000, 0.7456484326271539675, 1.000000000000000000),
 ( 1.000000000000000000, 0.7496697957975114734, 1.000000000000000000),
 ( 1.000000000000000000, 0.7619968371056987655, 1.000000000000000000),
 ( 1.000000000000000000, 0.7706756004923445147, 1.000000000000000000),
 ( 1.000000000000000000, 0.7883272815239725784, 1.000000000000000000),
 ( 1.000000000000000000, 0.7974260126898345957, 1.000000000000000000),
 ( 1.000000000000000000, 0.8067368806807374559, 1.000000000000000000) ) ) 
 REPRESENTATION_ITEM ( '' )  SURFACE ( )  );
#16938 = EDGE_LOOP ( 'NONE', ( #24951, #14156, #9858, #14838 ) ) ;
#16939 = CARTESIAN_POINT ( 'NONE',  ( 0.02559308416905495959, -1.400621020312459830, -0.6538911019815975001 ) ) ;
#16940 = CARTESIAN_POINT ( 'NONE',  ( 0.01056076242565423713, -0.5297871112653679271, 0.1536645982759194395 ) ) ;
#16941 = CARTESIAN_POINT ( 'NONE',  ( 0.2209956536232957902, -1.227897296991992793, 0.5182417262820130377 ) ) ;
#16942 = ORIENTED_EDGE ( 'NONE', *, *, #33135, .F. ) ;
#16943 = CARTESIAN_POINT ( 'NONE',  ( 0.1499999999999996336, 0.2450655194479851862, 0.4674710490749264258 ) ) ;
#16944 = CARTESIAN_POINT ( 'NONE',  ( 0.6775446752225827707, -1.407456786189307696, 0.5068639979343774193 ) ) ;
#16946 = ORIENTED_EDGE ( 'NONE', *, *, #21550, .F. ) ;
#16945 = ORIENTED_EDGE ( 'NONE', *, *, #5045, .T. ) ;
#16947 = CARTESIAN_POINT ( 'NONE',  ( 0.1499999999999990508, -0.4638115001431039053, -0.2459753896937787732 ) ) ;
#16948 = ADVANCED_FACE ( 'NONE', ( #33197 ), #23556, .T. ) ;
#16949 = VERTEX_POINT ( 'NONE', #36073 ) ;
#16950 = CARTESIAN_POINT ( 'NONE',  ( 0.3624061103390756600, -1.968824918581865591, -0.4968426515054816806 ) ) ;
#16951 = DIRECTION ( 'NONE',  ( 0.4999999999999972244, 0.000000000000000000, -0.8660254037844402619 ) ) ;
#16952 = DIRECTION ( 'NONE',  ( -8.881784197001246407E-16, 2.361472542561082612E-16, -1.000000000000000000 ) ) ;
#16953 = EDGE_LOOP ( 'NONE', ( #25302, #15015, #4257, #5242 ) ) ;
#16954 = CARTESIAN_POINT ( 'NONE',  ( 0.1875000000000003331, -0.4943738020624263707, 0.3123409581947972358 ) ) ;
#16955 = EDGE_CURVE ( 'NONE', #23240, #13700, #38863, .T. ) ;
#16956 = CARTESIAN_POINT ( 'NONE',  ( 0.08753440268785939171, -0.6845692626716118889, 0.1457185332388692967 ) ) ;
#16957 = EDGE_CURVE ( 'NONE', #29368, #28841, #21033, .T. ) ;
#16958 = CARTESIAN_POINT ( 'NONE',  ( 0.01220488679410611232, -0.4284039384462490774, 0.1900330486215427162 ) ) ;
#16959 = CARTESIAN_POINT ( 'NONE',  ( 0.4698606666588109326, -1.558018086733606200, 0.5753270877166933861 ) ) ;
#16961 = DIRECTION ( 'NONE',  ( 0.3468893892380796595, 0.7770416411309266635, -0.5252371270032120121 ) ) ;
#16960 = CARTESIAN_POINT ( 'NONE',  ( 0.1148172011972283663, -0.4713019633547693155, 0.03899715547817009936 ) ) ;
#16962 = CARTESIAN_POINT ( 'NONE',  ( 0.1230772935360478215, -0.9703466098372804938, 0.4773990857995715764 ) ) ;
#16963 = ORIENTED_EDGE ( 'NONE', *, *, #28518, .T. ) ;
#16964 = EDGE_CURVE ( 'NONE', #556, #7698, #11362, .T. ) ;
#16965 = EDGE_CURVE ( 'NONE', #36975, #20955, #27025, .T. ) ;
#16966 = CARTESIAN_POINT ( 'NONE',  ( -0.2746410161513770931, -2.909786385774835171, -0.3705357231075770419 ) ) ;
#16967 = CARTESIAN_POINT ( 'NONE',  ( 0.2702030311564788123, -0.6895941179718233505, 0.6181208260419542855 ) ) ;
#16968 = EDGE_CURVE ( 'NONE', #7866, #12909, #20183, .T. ) ;
#16969 = CARTESIAN_POINT ( 'NONE',  ( -0.05281452789367979683, 0.2421206024358339981, -0.4009379267244608247 ) ) ;
#16970 = CARTESIAN_POINT ( 'NONE',  ( 0.1499999999999996059, -0.2372406987223689145, -0.4850946823762606330 ) ) ;
#16971 = CARTESIAN_POINT ( 'NONE',  ( 0.0004750592482352814579, -0.4386115460793976739, 0.1457185332388683252 ) ) ;
#16972 = AXIS2_PLACEMENT_3D ( 'NONE', #32373, #7264, #752 ) ;
#16973 = DIRECTION ( 'NONE',  ( -1.000000000000000000, 0.000000000000000000, 0.000000000000000000 ) ) ;
#16974 = CARTESIAN_POINT ( 'NONE',  ( 0.4340563226180833012, -1.025953197730038458, 0.7364845616659437821 ) ) ;
#16975 = DIRECTION ( 'NONE',  ( 5.551115123125868984E-17, -5.531779426422974156E-16, -1.000000000000000000 ) ) ;
#16976 = EDGE_CURVE ( 'NONE', #12586, #24566, #10172, .T. ) ;
#16977 = CARTESIAN_POINT ( 'NONE',  ( 0.01522254512315708574, -0.9178457916527728022, 0.5707280127493563615 ) ) ;
#16978 = DIRECTION ( 'NONE',  ( 9.571496092079945511E-16, -0.7692307692307691624, 0.6389710663783134681 ) ) ;
#16979 = CARTESIAN_POINT ( 'NONE',  ( 0.4958723899955516101, -1.679082390730774144, -0.6092321650988190562 ) ) ;
#16980 = ORIENTED_EDGE ( 'NONE', *, *, #17010, .T. ) ;
#16981 = CARTESIAN_POINT ( 'NONE',  ( 0.2764424605908987753, -0.9705060276339172454, 0.7215845397199748268 ) ) ;
#16982 = CARTESIAN_POINT ( 'NONE',  ( 0.01548846960721255751, -0.07651041855108323131, 0.5222379212565277928 ) ) ;
#16983 = CARTESIAN_POINT ( 'NONE',  ( -0.02953079040095601959, -0.2329676531120513372, -0.4763574306556331295 ) ) ;
#16984 = ORIENTED_EDGE ( 'NONE', *, *, #26367, .T. ) ;
#16985 = CARTESIAN_POINT ( 'NONE',  ( -0.1743922129835733803, -0.5166151207188712791, 0.3749999999999999445 ) ) ;
#16986 = VERTEX_POINT ( 'NONE', #4515 ) ;
#16987 = CARTESIAN_POINT ( 'NONE',  ( 0.09587083108297865530, -0.6074767732719537072, 0.2950264738744098891 ) ) ;
#16988 = CARTESIAN_POINT ( 'NONE',  ( 0.3088664963667261398, -1.757905065063135597, 0.5295467280985148850 ) ) ;
#16989 = DIRECTION ( 'NONE',  ( -0.9998941247116546194, 0.01455087607601020239, -0.0001066420868422379362 ) ) ;
#16990 = CARTESIAN_POINT ( 'NONE',  ( 0.1420085715566430373, -1.022094752421645492, 0.7158645833976974293 ) ) ;
#16991 = ORIENTED_EDGE ( 'NONE', *, *, #769, .F. ) ;
#16992 = CARTESIAN_POINT ( 'NONE',  ( -0.1608142870581997230, 0.4995150451154461990, 0.3323678566780360333 ) ) ;
#16993 = CARTESIAN_POINT ( 'NONE',  ( 0.6335899703865320864, -1.596177751663357736, -0.4443638777805991591 ) ) ;
#16994 = CARTESIAN_POINT ( 'NONE',  ( 0.4619737557705557163, -1.656318618979952584, -0.6360981484938359465 ) ) ;
#16995 = CARTESIAN_POINT ( 'NONE',  ( 0.2161879510971927709, -1.277123080371499020, -0.7187326247832955817 ) ) ;
#16996 = CARTESIAN_POINT ( 'NONE',  ( 0.3506455678375485219, -1.087518136233734278, 0.7199871270596691630 ) ) ;
#16998 = CARTESIAN_POINT ( 'NONE',  ( 0.3597996879153266270, -1.933544513296585166, -0.4937070853543361060 ) ) ;
#16997 = CYLINDRICAL_SURFACE ( 'NONE', #34432, 0.1000000000000000056 ) ;
#16999 = CARTESIAN_POINT ( 'NONE',  ( 0.5840964882222685617, -1.491811162635231058, -0.4356935235874836998 ) ) ;
#17000 = ORIENTED_EDGE ( 'NONE', *, *, #21836, .T. ) ;
#17001 = DIRECTION ( 'NONE',  ( -1.000000000000000000, 0.000000000000000000, 0.000000000000000000 ) ) ;
#17002 = ORIENTED_EDGE ( 'NONE', *, *, #721, .F. ) ;
#17003 = EDGE_CURVE ( 'NONE', #24257, #24870, #13598, .T. ) ;
#17004 = ORIENTED_EDGE ( 'NONE', *, *, #2221, .F. ) ;
#17005 = CARTESIAN_POINT ( 'NONE',  ( 0.3994775562665067725, -1.543474704417578502, 0.7765694768245218205 ) ) ;
#17007 = CARTESIAN_POINT ( 'NONE',  ( 0.4460751111563584503, -1.103507073082631074, -0.6308736239710884819 ) ) ;
#17006 = CARTESIAN_POINT ( 'NONE',  ( 0.08840096076972359107, -0.6251151962830620024, 0.03934731828055227504 ) ) ;
#17008 = CARTESIAN_POINT ( 'NONE',  ( 0.1825980849618502877, -1.261391773294454399, 0.5182417262812422099 ) ) ;
#17009 = ORIENTED_EDGE ( 'NONE', *, *, #1442, .T. ) ;
#17010 = EDGE_CURVE ( 'NONE', #34558, #38795, #23865, .T. ) ;
#17011 = ORIENTED_EDGE ( 'NONE', *, *, #4199, .T. ) ;
#17012 = LINE ( 'NONE', #1395, #27392 ) ;
#17013 = EDGE_CURVE ( 'NONE', #19731, #9282, #14098, .T. ) ;
#17014 = CARTESIAN_POINT ( 'NONE',  ( 0.5500705290592691199, -1.461052471298058375, 0.7365222812456531098 ) ) ;
#17015 = ORIENTED_EDGE ( 'NONE', *, *, #21052, .F. ) ;
#17016 = CARTESIAN_POINT ( 'NONE',  ( 0.05999999999999990757, 0.000000000000000000, 0.000000000000000000 ) ) ;
#17017 = DIRECTION ( 'NONE',  ( -0.4999551463232377313, 0.8660512985181132439, -0.000000000000000000 ) ) ;
#17018 = CARTESIAN_POINT ( 'NONE',  ( 2.845524969048586056E-18, 0.2900000000000004796, 0.04249999999999948957 ) ) ;
#17019 = PRODUCT_DEFINITION_SHAPE ( 'NONE', 'NONE',  #40656 ) ;
#17020 = CARTESIAN_POINT ( 'NONE',  ( 0.1811801731470885635, -1.262447345873583426, 0.4381703640825295731 ) ) ;
#17021 = CARTESIAN_POINT ( 'NONE',  ( 0.3842063748693837488, -1.733091723360132841, 0.4185254220199500774 ) ) ;
#17022 = B_SPLINE_CURVE_WITH_KNOTS ( 'NONE', 3,
 ( #37363, #9174, #25022, #37172, #18650, #37553, #31408, #8987, #21555, #25230, #34074, #24640, #13681, #26244 ),
 .UNSPECIFIED., .F., .F.,
 ( 4, 2, 2, 2, 2, 2, 4 ),
 ( 5.637184056103667372E-17, 0.0004877684492138178052, 0.0007316526738207009039, 0.0008535947861241437000, 0.0009145658422758637428, 0.0009450513703517257700, 0.0009755368984275879056 ),
 .UNSPECIFIED. ) ;
#17023 = DIRECTION ( 'NONE',  ( 0.000000000000000000, 3.330669073875470114E-16, 1.000000000000000000 ) ) ;
#17024 = CARTESIAN_POINT ( 'NONE',  ( 0.1893427799090355301, -0.4853919354581605061, 0.2707563002020392240 ) ) ;
#17025 = CARTESIAN_POINT ( 'NONE',  ( 0.1734973056165642902, -1.209394307038482719, -0.5155029497116575543 ) ) ;
#17026 = ADVANCED_FACE ( 'NONE', ( #16474 ), #21895, .F. ) ;
#17027 = CARTESIAN_POINT ( 'NONE',  ( 0.08110577511515054683, -1.318921603477608118, 0.5655786468447775439 ) ) ;
#17028 = APPLICATION_PROTOCOL_DEFINITION ( 'international standard', 'automotive_design', 2000, #26376 ) ;
#17029 = B_SPLINE_CURVE_WITH_KNOTS ( 'NONE', 3,
 ( #4997, #33388, #14452, #36069, #17746, #7468, #1540, #32578, #14062, #26639, #39168, #5604 ),
 .UNSPECIFIED., .F., .F.,
 ( 4, 2, 2, 2, 2, 4 ),
 ( 0.000000000000000000, 0.0002481559604999103051, 0.0004963119209998206102, 0.0007444678814997309152, 0.0008685458617496860136, 0.0009926238419996412203 ),
 .UNSPECIFIED. ) ;
#17030 = CARTESIAN_POINT ( 'NONE',  ( 0.3174141940625345160, -1.772900390203313137, 0.5327102575848723376 ) ) ;
#17031 = EDGE_CURVE ( 'NONE', #17308, #25560, #880, .T. ) ;
#17032 = CARTESIAN_POINT ( 'NONE',  ( 0.04308611741967655756, 0.2425947520953613545, 0.4306844107907248920 ) ) ;
#17033 = CARTESIAN_POINT ( 'NONE',  ( -0.1157923916715156154, -0.5295015842444055210, 0.3181161673586314631 ) ) ;
#17034 = FACE_OUTER_BOUND ( 'NONE', #4684, .T. ) ;
#17035 = CARTESIAN_POINT ( 'NONE',  ( 0.1001698831744081003, -1.307806316238550703, 0.4450799649317093709 ) ) ;
#17036 = VERTEX_POINT ( 'NONE', #32504 ) ;
#17037 = CARTESIAN_POINT ( 'NONE',  ( 0.1576987512544144876, -1.257723164589890308, 0.9396174402501648038 ) ) ;
#17038 = CARTESIAN_POINT ( 'NONE',  ( 0.5777123731605773305, -1.533644566602507142, -0.4683381307628363688 ) ) ;
#17039 = CARTESIAN_POINT ( 'NONE',  ( -0.2399999999999999079, -4.233163482269810096, -0.5148221395285308422 ) ) ;
#17040 = CARTESIAN_POINT ( 'NONE',  ( -0.2746410161513782033, -2.253314830856113726, -0.6753616220517687507 ) ) ;
#17041 = CARTESIAN_POINT ( 'NONE',  ( -0.05544444631433697451, -0.2544607094502361333, 0.3847718460475692548 ) ) ;
#17042 = ORIENTED_EDGE ( 'NONE', *, *, #32785, .F. ) ;
#17043 = VERTEX_POINT ( 'NONE', #17078 ) ;
#17044 = CARTESIAN_POINT ( 'NONE',  ( 0.4971324743577882899, -1.079965756743124006, 0.4177417262808780229 ) ) ;
#17045 = ORIENTED_EDGE ( 'NONE', *, *, #15801, .F. ) ;
#17046 = FACE_OUTER_BOUND ( 'NONE', #32692, .T. ) ;
#17047 = DIRECTION ( 'NONE',  ( -0.4999551463232372317, 0.8660512985181135770, -0.000000000000000000 ) ) ;
#17048 = CARTESIAN_POINT ( 'NONE',  ( 0.5153315922689613027, -1.320405065595526839, 0.7260202612431515545 ) ) ;
#17049 = ORIENTED_EDGE ( 'NONE', *, *, #201, .T. ) ;
#17050 = CARTESIAN_POINT ( 'NONE',  ( 0.2577558225373174916, -0.8624250852862554995, 0.5195666343558283939 ) ) ;
#17051 = CARTESIAN_POINT ( 'NONE',  ( -0.2399999999999999079, -2.511040369707300268, -0.6548468226404909887 ) ) ;
#17052 = EDGE_LOOP ( 'NONE', ( #23231, #40318, #18218, #35266 ) ) ;
#17053 = CARTESIAN_POINT ( 'NONE',  ( -0.01548846960707463312, 0.4638115001430995199, 0.2459753896937826034 ) ) ;
#17054 = CARTESIAN_POINT ( 'NONE',  ( 0.3183059118147241184, -1.589430717261796744, 0.7981046197357909433 ) ) ;
#17056 = CARTESIAN_POINT ( 'NONE',  ( -0.03662792686184479507, -0.4685177067346103508, 0.1089945633920634538 ) ) ;
#17055 = CARTESIAN_POINT ( 'NONE',  ( 0.6732088238915016065, -1.530595336554058550, 0.4388990213126219841 ) ) ;
#17057 = CARTESIAN_POINT ( 'NONE',  ( 0.2320755761173002307, -1.232873731908348480, 0.4177417262808779674 ) ) ;
#17058 = EDGE_CURVE ( 'NONE', #10109, #35064, #27145, .T. ) ;
#17059 = CARTESIAN_POINT ( 'NONE',  ( 0.1190035864140202432, -1.325422344506462125, -0.3481589277964427520 ) ) ;
#17060 = VERTEX_POINT ( 'NONE', #25963 ) ;
#17061 = CARTESIAN_POINT ( 'NONE',  ( 0.4844396616870721428, -1.590460616370065194, -0.5829707516598297001 ) ) ;
#17062 = CARTESIAN_POINT ( 'NONE',  ( 0.07931082089408725277, -1.397336969168096577, -0.6634856036505109023 ) ) ;
#17063 = CYLINDRICAL_SURFACE ( 'NONE', #20737, 0.1033070866141732880 ) ;
#17064 = CARTESIAN_POINT ( 'NONE',  ( 0.2857211932547981115, -1.109133886523115731, 0.7441438648489260288 ) ) ;
#17065 = DIRECTION ( 'NONE',  ( 0.01265474379914258672, 0.8659329421511292590, -0.4999999971568669932 ) ) ;
#17066 = CARTESIAN_POINT ( 'NONE',  ( -0.1399999999999997358, -9.793929126999064681E-17, -0.2150000000000000244 ) ) ;
#17067 = DIRECTION ( 'NONE',  ( 0.000000000000000000, -0.5781348229923759519, 0.8159412518334724362 ) ) ;
#17068 = CARTESIAN_POINT ( 'NONE',  ( 0.6652959480876716736, -1.517233971325829600, 0.4231557572046961146 ) ) ;
#17069 = DIRECTION ( 'NONE',  ( 7.771561172376107616E-16, -7.170354002788761615E-17, 1.000000000000000000 ) ) ;
#17070 = DIRECTION ( 'NONE',  ( 1.000000000000000000, 0.000000000000000000, 0.000000000000000000 ) ) ;
#17071 = DIRECTION ( 'NONE',  ( 1.000000000000000000, 6.779273404243070203E-32, 4.314083075427407763E-32 ) ) ;
#17072 = DATE_AND_TIME ( #29224, #9483 ) ;
#17073 = EDGE_CURVE ( 'NONE', #15505, #22378, #10917, .T. ) ;
#17074 = EDGE_CURVE ( 'NONE', #9066, #7581, #29432, .T. ) ;
#17075 = CARTESIAN_POINT ( 'NONE',  ( 0.3881929885797955615, -1.150008520685900315, 0.4234575807221065968 ) ) ;
#17076 = FACE_OUTER_BOUND ( 'NONE', #25181, .T. ) ;
#17077 = CARTESIAN_POINT ( 'NONE',  ( 0.2161879510971928264, -1.277123080371499020, -0.3144976166544468099 ) ) ;
#17078 = CARTESIAN_POINT ( 'NONE',  ( 0.05999999999999990757, 7.654042494670954463E-18, -0.06250000000000000000 ) ) ;
#17079 = LINE ( 'NONE', #11527, #25203 ) ;
#17080 = DIRECTION ( 'NONE',  ( 1.000000000000000000, 2.280301054154495132E-31, -1.664003471950577689E-31 ) ) ;
#17081 = AXIS2_PLACEMENT_3D ( 'NONE', #9210, #6122, #18475 ) ;
#17082 = DIRECTION ( 'NONE',  ( 1.776356839400255198E-15, 2.542300904468944507E-15, 1.000000000000000000 ) ) ;
#17083 = VERTEX_POINT ( 'NONE', #35398 ) ;
#17084 = VERTEX_POINT ( 'NONE', #38874 ) ;
#17085 = VECTOR ( 'NONE', #18101, 39.37007874015748143 ) ;
#17086 = CARTESIAN_POINT ( 'NONE',  ( 0.3921921748761933446, -1.728262305561636181, 0.4265845344340060685 ) ) ;
#17087 = ORIENTED_EDGE ( 'NONE', *, *, #29614, .F. ) ;
#17088 = CARTESIAN_POINT ( 'NONE',  ( 0.5347516980328250735, -1.174037678574211263, -0.6056023639864149821 ) ) ;
#17089 = CARTESIAN_POINT ( 'NONE',  ( 0.1459722773112856753, -0.6340201870151221941, 0.3850682184254722862 ) ) ;
#17090 = B_SPLINE_CURVE_WITH_KNOTS ( 'NONE', 3,
 ( #38262, #4319, #7182, #16670, #39084, #675, #10696, #29222 ),
 .UNSPECIFIED., .F., .F.,
 ( 4, 2, 2, 4 ),
 ( 0.000000000000000000, 0.0004476527168006422686, 0.0008953054336012845373, 0.001790610867202582519 ),
 .UNSPECIFIED. ) ;
#17092 = ORIENTED_EDGE ( 'NONE', *, *, #904, .T. ) ;
#17091 = CARTESIAN_POINT ( 'NONE',  ( -0.0008433103373208181977, -0.7682816629019912913, 0.007858431574465824659 ) ) ;
#17094 = VERTEX_POINT ( 'NONE', #13781 ) ;
#17093 = ORIENTED_EDGE ( 'NONE', *, *, #29097, .T. ) ;
#17095 = CARTESIAN_POINT ( 'NONE',  ( -0.2399999999999999079, -3.941790907013290823, -0.4709369376873030477 ) ) ;
#17096 = VERTEX_POINT ( 'NONE', #10705 ) ;
#17097 = CARTESIAN_POINT ( 'NONE',  ( 0.2154282780885227178, -1.466805515833779383, 0.9278870098542323364 ) ) ;
#17099 = DIRECTION ( 'NONE',  ( 0.000000000000000000, 0.5365213554527455964, -0.8438867430782097667 ) ) ;
#17098 = CARTESIAN_POINT ( 'NONE',  ( 0.04211812644076717155, 0.4433543613217461599, 0.1530385388104468225 ) ) ;
#17100 = DIRECTION ( 'NONE',  ( -1.000000000000000000, -2.280301054154495132E-31, 1.664003471950577689E-31 ) ) ;
#17101 = PERSON_AND_ORGANIZATION ( #578, #36593 ) ;
#17102 = ADVANCED_FACE ( 'NONE', ( #26347 ), #38269, .T. ) ;
#17103 = DIRECTION ( 'NONE',  ( 1.000000000000000000, 6.779273404243070203E-32, 4.314083075427408311E-32 ) ) ;
#17105 = EDGE_LOOP ( 'NONE', ( #10615, #2350, #7191, #35038 ) ) ;
#17104 = ORIENTED_EDGE ( 'NONE', *, *, #17915, .T. ) ;
#17106 = CARTESIAN_POINT ( 'NONE',  ( 0.09278199725800895248, -0.7971562777438269132, 0.2877230682800478445 ) ) ;
#17107 = CARTESIAN_POINT ( 'NONE',  ( 0.1188169051961329437, -1.413502985213658247, 0.5800534899519873555 ) ) ;
#17108 = CARTESIAN_POINT ( 'NONE',  ( 0.06935100149987896700, -0.5417505261625371604, 0.1708526567523814543 ) ) ;
#17109 = CARTESIAN_POINT ( 'NONE',  ( 0.5540999761718204963, -1.510283947878215516, 0.6075923333766917178 ) ) ;
#17110 = CARTESIAN_POINT ( 'NONE',  ( 0.3300460303897821968, -1.638469719739709118, -0.3391576931604809997 ) ) ;
#17111 = DIRECTION ( 'NONE',  ( 2.157041537713702240E-32, -0.8709776783778059306, 0.4913225862583635584 ) ) ;
#17112 = CARTESIAN_POINT ( 'NONE',  ( 0.7007246779392307667, -1.487338553264568208, 0.4637699275333992954 ) ) ;
#17113 = VECTOR ( 'NONE', #15771, 39.37007874015748143 ) ;
#17114 = CARTESIAN_POINT ( 'NONE',  ( 0.4880253864272864894, -1.700462583248872894, 0.5182417262812423209 ) ) ;
#17115 = CARTESIAN_POINT ( 'NONE',  ( 0.6654360144368460794, -1.561514405424819119, 0.5611086426770289792 ) ) ;
#17116 = CARTESIAN_POINT ( 'NONE',  ( 0.06463019578131175280, -1.332095939219700487, 0.5196073683862424408 ) ) ;
#17117 = CARTESIAN_POINT ( 'NONE',  ( 0.07885325192267222949, -1.319783927197341944, 0.4754891053729509154 ) ) ;
#17118 = AXIS2_PLACEMENT_3D ( 'NONE', #38883, #7200, #894 ) ;
#17119 = CARTESIAN_POINT ( 'NONE',  ( 0.3336325236675090067, -1.050835064020409160, 0.7593003920438236021 ) ) ;
#17120 = CARTESIAN_POINT ( 'NONE',  ( 0.01166930780816748982, -0.7552342480465903396, -0.1042461971847544744 ) ) ;
#17121 = FACE_OUTER_BOUND ( 'NONE', #40169, .T. ) ;
#17122 = CARTESIAN_POINT ( 'NONE',  ( 0.4909801108973092520, -1.199306193601649362, -0.5155029497116575543 ) ) ;
#17123 = DIRECTION ( 'NONE',  ( 1.188678714063518227E-15, -1.000000000000000000, -3.263080277421930985E-16 ) ) ;
#17124 = CARTESIAN_POINT ( 'NONE',  ( 0.1861033513463754285, -1.549633035783825497, 0.5860151309145639198 ) ) ;
#17125 = CARTESIAN_POINT ( 'NONE',  ( 0.4929465528686921005, -1.082715557938388029, 0.5682417262808779901 ) ) ;
#17126 = PRODUCT_CONTEXT ( 'NONE', #5310, 'mechanical' ) ;
#17127 = CARTESIAN_POINT ( 'NONE',  ( 0.7185399166019250661, -1.465950542831855330, 0.7545741816404391011 ) ) ;
#17128 = EDGE_CURVE ( 'NONE', #37277, #30555, #9385, .T. ) ;
#17129 = FACE_OUTER_BOUND ( 'NONE', #26170, .T. ) ;
#17130 = DIRECTION ( 'NONE',  ( -3.543711097672506306E-32, 0.6954292836768432018, 0.7185945389471819489 ) ) ;
#17131 = ORIENTED_EDGE ( 'NONE', *, *, #2937, .T. ) ;
#17132 = LINE ( 'NONE', #30093, #27019 ) ;
#17133 = CARTESIAN_POINT ( 'NONE',  ( 0.01055999354154114368, -0.5296565605740094496, 0.1394354128953858296 ) ) ;
#17134 = AXIS2_PLACEMENT_3D ( 'NONE', #17563, #36481, #30106 ) ;
#17135 = CARTESIAN_POINT ( 'NONE',  ( 0.1947076744186670427, -1.243108242024598242, 0.4512817965407442955 ) ) ;
#17137 = ORIENTED_EDGE ( 'NONE', *, *, #2383, .F. ) ;
#17136 = FACE_OUTER_BOUND ( 'NONE', #33793, .T. ) ;
#17138 = CARTESIAN_POINT ( 'NONE',  ( 0.3267680042207918301, -1.758262944587549503, 0.4789874961554916322 ) ) ;
#17139 = CARTESIAN_POINT ( 'NONE',  ( 0.5691520580847880817, -1.222151117369431939, 0.8040585553043922973 ) ) ;
#17141 = ORIENTED_EDGE ( 'NONE', *, *, #32786, .T. ) ;
#17140 = ORIENTED_EDGE ( 'NONE', *, *, #13262, .F. ) ;
#17142 = CARTESIAN_POINT ( 'NONE',  ( 0.01265409468558189275, -1.700310348714810349, -0.6650692675765490502 ) ) ;
#17143 = AXIS2_PLACEMENT_3D ( 'NONE', #22636, #26128, #32253 ) ;
#17144 = EDGE_LOOP ( 'NONE', ( #38774, #3359, #5952, #7481, #2637 ) ) ;
#17145 = CARTESIAN_POINT ( 'NONE',  ( 0.1637488714925408873, -0.5994898440788770655, 0.1932149833450298726 ) ) ;
#17146 = AXIS2_PLACEMENT_3D ( 'NONE', #17242, #38079, #6402 ) ;
#17147 = FACE_OUTER_BOUND ( 'NONE', #27950, .T. ) ;
#17148 = AXIS2_PLACEMENT_3D ( 'NONE', #12260, #34053, #27490 ) ;
#17149 = CARTESIAN_POINT ( 'NONE',  ( -0.04140212552917778288, 0.4420250499596291571, -0.1614397576335124540 ) ) ;
#17150 = VERTEX_POINT ( 'NONE', #7009 ) ;
#17151 = DIRECTION ( 'NONE',  ( 0.8660512985181132439, 0.4999551463232376758, 0.000000000000000000 ) ) ;
#17152 = CARTESIAN_POINT ( 'NONE',  ( 0.1058028591704159582, -0.7174348744888263685, 0.3722218170207774457 ) ) ;
#17153 = CARTESIAN_POINT ( 'NONE',  ( 0.2539806336202973247, -1.480393849963148600, 1.018971347781354231 ) ) ;
#17154 = CARTESIAN_POINT ( 'NONE',  ( 0.2457936252450182157, -1.026797302826530034, 0.7978041782991802666 ) ) ;
#17156 = CARTESIAN_POINT ( 'NONE',  ( -0.1151895542371739328, -0.5267561842548686979, 0.1296992319623857803 ) ) ;
#17155 = CARTESIAN_POINT ( 'NONE',  ( 0.2681791922883234869, -1.687400927718340826, 0.6168360553784030254 ) ) ;
#17157 = CARTESIAN_POINT ( 'NONE',  ( 0.1811302593339075007, -1.059783243163161970, 0.6264505142422892581 ) ) ;
#17158 = EDGE_LOOP ( 'NONE', ( #35969, #37037, #28642, #39867 ) ) ;
#17159 = DIRECTION ( 'NONE',  ( 0.000000000000000000, -2.731847993664239947E-15, -1.000000000000000000 ) ) ;
#17160 = CARTESIAN_POINT ( 'NONE',  ( 0.1932692805625377541, -0.5636194602968859213, 0.2661166255916873058 ) ) ;
#17161 = DIRECTION ( 'NONE',  ( 1.000000000000000000, -0.000000000000000000, -0.000000000000000000 ) ) ;
#17162 = CARTESIAN_POINT ( 'NONE',  ( -0.05137569054208215857, -0.4416101343670569834, -0.1670214652524110166 ) ) ;
#17163 = VECTOR ( 'NONE', #4626, 39.37007874015748143 ) ;
#17164 = CARTESIAN_POINT ( 'NONE',  ( -0.01548846960707477016, 0.5198120922912062847, -0.07362328916748482610 ) ) ;
#17165 = B_SPLINE_CURVE_WITH_KNOTS ( 'NONE', 3,
 ( #37465, #17939, #9283, #21863, #28218, #33561, #24147, #18970, #6805, #22682 ),
 .UNSPECIFIED., .F., .F.,
 ( 4, 2, 2, 2, 4 ),
 ( 0.000000000000000000, 0.0003219901686702020174, 0.0006439803373404040347, 0.0009659705060106060521, 0.001287960674680808069 ),
 .UNSPECIFIED. ) ;
#17166 = AXIS2_PLACEMENT_3D ( 'NONE', #8814, #14793, #18079 ) ;
#17167 = FACE_OUTER_BOUND ( 'NONE', #39108, .T. ) ;
#17168 = CARTESIAN_POINT ( 'NONE',  ( 0.5387674647098039671, -1.171534441891039169, 0.7413454372389880476 ) ) ;
#17169 = AXIS2_PLACEMENT_3D ( 'NONE', #32365, #16952, #16544 ) ;
#17170 =( BOUNDED_SURFACE ( )  B_SPLINE_SURFACE ( 3, 2, ( 
 ( #2009, #11468, #24031 ),
 ( #20935, #2213, #15357 ),
 ( #24421, #39633, #33657 ),
 ( #37359, #5871, #30786 ),
 ( #24836, #21551, #33457 ),
 ( #17822, #34070, #30592 ),
 ( #37166, #21734, #39844 ),
 ( #36747, #8558, #2415 ),
 ( #18431, #14953, #8771 ),
 ( #33884, #5687, #2606 ),
 ( #15143, #27704, #12073 ),
 ( #8980, #24636, #30985 ),
 ( #2808, #25224, #28115 ),
 ( #22558, #18864, #38365 ),
 ( #28723, #3206, #35089 ),
 ( #15751, #40646, #16182 ),
 ( #28905, #31404, #9587 ),
 ( #585, #13078, #15963 ),
 ( #13277, #6485, #386 ),
 ( #3811, #18646, #34480 ),
 ( #6291, #31591, #28301 ),
 ( #771, #31206, #37768 ),
 ( #169, #19054, #25633 ),
 ( #25017, #31804, #38164 ),
 ( #3023, #9988, #12659 ),
 ( #3408, #22166, #3618 ),
 ( #28510, #15568, #34680 ),
 ( #12884, #22770, #25845 ),
 ( #25443, #12463, #37974 ),
 ( #37549, #9784, #22354 ),
 ( #34875, #6686, #19261 ),
 ( #6893, #19467, #32000 ),
 ( #16367, #9371, #10203 ),
 ( #6076, #21953, #33363 ),
 ( #13676, #4004, #29112 ),
 ( #35693, #39944, #8270 ) ),
 .UNSPECIFIED., .F., .F., .F. ) 
 B_SPLINE_SURFACE_WITH_KNOTS ( ( 4, 2, 2, 2, 2, 2, 2, 2, 2, 2, 2, 2, 2, 2, 2, 2, 2, 4 ),
 ( 3, 3 ),
 ( 0.006158837752303239141, 0.008831284596174333867, 0.01150373144004543033, 0.01417617828391652506, 0.01551240170585207329, 0.01684862512778761978, 0.01818484854972316628, 0.01952107197165871277, 0.02018918368262648602, 0.02085729539359425927, 0.02152540710456203599, 0.02219351881552980923, 0.02352974223746535920, 0.02486596565940090570, 0.02553407737036867894, 0.02620218908133645219, 0.02687030079230422544, 0.02753841250327199869 ),
 ( 0.000000000000000000, 1.000000000000000000 ),
 .UNSPECIFIED. ) 
 GEOMETRIC_REPRESENTATION_ITEM ( )  RATIONAL_B_SPLINE_SURFACE ( (
 ( 1.000000000000000000, 0.6567084680803600971, 1.000000000000000000),
 ( 1.000000000000000000, 0.6566839907465437109, 1.000000000000000000),
 ( 1.000000000000000000, 0.6572021228041137197, 1.000000000000000000),
 ( 1.000000000000000000, 0.6579559531357345170, 1.000000000000000000),
 ( 1.000000000000000000, 0.6581132063349907080, 1.000000000000000000),
 ( 1.000000000000000000, 0.6570134697022161907, 1.000000000000000000),
 ( 1.000000000000000000, 0.6557949822498931880, 1.000000000000000000),
 ( 1.000000000000000000, 0.6519304267099326200, 1.000000000000000000),
 ( 1.000000000000000000, 0.6503122123076459093, 1.000000000000000000),
 ( 1.000000000000000000, 0.6462645446810073580, 1.000000000000000000),
 ( 1.000000000000000000, 0.6438349337072757361, 1.000000000000000000),
 ( 1.000000000000000000, 0.6382227172733763165, 1.000000000000000000),
 ( 1.000000000000000000, 0.6351102327385169666, 1.000000000000000000),
 ( 1.000000000000000000, 0.6287744411780002984, 1.000000000000000000),
 ( 1.000000000000000000, 0.6257180153651936694, 1.000000000000000000),
 ( 1.000000000000000000, 0.6223102534591248292, 1.000000000000000000),
 ( 1.000000000000000000, 0.6213451726380976314, 1.000000000000000000),
 ( 1.000000000000000000, 0.6201746544136139683, 1.000000000000000000),
 ( 1.000000000000000000, 0.6200976022680225741, 1.000000000000000000),
 ( 1.000000000000000000, 0.6203287173039150337, 1.000000000000000000),
 ( 1.000000000000000000, 0.6206481638358333219, 1.000000000000000000),
 ( 1.000000000000000000, 0.6220779520615170588, 1.000000000000000000),
 ( 1.000000000000000000, 0.6233032503211219932, 1.000000000000000000),
 ( 1.000000000000000000, 0.6274491077548256523, 1.000000000000000000),
 ( 1.000000000000000000, 0.6306542643529917669, 1.000000000000000000),
 ( 1.000000000000000000, 0.6389337287488969785, 1.000000000000000000),
 ( 1.000000000000000000, 0.6434217649977074238, 1.000000000000000000),
 ( 1.000000000000000000, 0.6522238611423898380, 1.000000000000000000),
 ( 1.000000000000000000, 0.6557613510651914002, 1.000000000000000000),
 ( 1.000000000000000000, 0.6639824573846913047, 1.000000000000000000),
 ( 1.000000000000000000, 0.6683217727600526681, 1.000000000000000000),
 ( 1.000000000000000000, 0.6790624151853396073, 1.000000000000000000),
 ( 1.000000000000000000, 0.6862971593358724309, 1.000000000000000000),
 ( 1.000000000000000000, 0.7000895111908658208, 1.000000000000000000),
 ( 1.000000000000000000, 0.7087223284753119135, 1.000000000000000000),
 ( 1.000000000000000000, 0.7109670133747438836, 1.000000000000000000) ) ) 
 REPRESENTATION_ITEM ( '' )  SURFACE ( )  );
#17171 = CARTESIAN_POINT ( 'NONE',  ( 0.08973038502581247300, -1.323151139955826450, 0.4733271373649473035 ) ) ;
#17172 = AXIS2_PLACEMENT_3D ( 'NONE', #30447, #30226, #11529 ) ;
#17173 = CARTESIAN_POINT ( 'NONE',  ( 0.02988725412889516389, -2.019627616784832380, -0.2840895204354123571 ) ) ;
#17174 = CARTESIAN_POINT ( 'NONE',  ( 0.3224586748600002384, -1.296590453040780799, 0.4182417262808783009 ) ) ;
#17175 = VERTEX_POINT ( 'NONE', #36002 ) ;
#17176 = EDGE_CURVE ( 'NONE', #21164, #13737, #10619, .T. ) ;
#17177 = CARTESIAN_POINT ( 'NONE',  ( 0.3121678834194830943, -1.028870205852967512, 0.7302106030273709525 ) ) ;
#17178 = CARTESIAN_POINT ( 'NONE',  ( -0.2746410161513782033, -1.962518963160043706, -0.3791801492432048115 ) ) ;
#17179 = FACE_OUTER_BOUND ( 'NONE', #11094, .T. ) ;
#17180 = EDGE_CURVE ( 'NONE', #25706, #15019, #26863, .T. ) ;
#17181 = VERTEX_POINT ( 'NONE', #19575 ) ;
#17182 = LINE ( 'NONE', #5230, #22693 ) ;
#17183 = CARTESIAN_POINT ( 'NONE',  ( -0.05283094505690071052, 0.03968992937477607008, -0.4666439588235273828 ) ) ;
#17184 = ADVANCED_FACE ( 'NONE', ( #39291 ), #37645, .T. ) ;
#17185 = CARTESIAN_POINT ( 'NONE',  ( 0.4292533899499677563, -1.122974568708051013, 0.5176300287282207258 ) ) ;
#17186 = ADVANCED_FACE ( 'NONE', ( #39900 ), #30044, .T. ) ;
#17187 = CARTESIAN_POINT ( 'NONE',  ( 0.04712643034123224772, -0.8746274208907861558, 0.4664299315230325815 ) ) ;
#17188 = ORIENTED_EDGE ( 'NONE', *, *, #5740, .F. ) ;
#17189 = CARTESIAN_POINT ( 'NONE',  ( -0.02235124290213137341, 0.3550643254722171127, 0.3695962758878529320 ) ) ;
#17190 = CARTESIAN_POINT ( 'NONE',  ( 0.01548846960707342575, 0.07651041855119247725, 0.5222379212568240003 ) ) ;
#17191 = CARTESIAN_POINT ( 'NONE',  ( 0.3712555767072253654, -1.761044764944616814, -0.4317137529336340096 ) ) ;
#17192 = CARTESIAN_POINT ( 'NONE',  ( -0.02000000000000000042, -1.646519645934556131, -0.1171471737359304072 ) ) ;
#17193 = CARTESIAN_POINT ( 'NONE',  ( 0.4773696427185842861, -1.254357306845002684, 0.6502240367204457083 ) ) ;
#17194 = VECTOR ( 'NONE', #11951, 39.37007874015748143 ) ;
#17196 = CARTESIAN_POINT ( 'NONE',  ( 0.1640786445897259860, -1.229311324678093786, 0.5182417262812423209 ) ) ;
#17195 = CARTESIAN_POINT ( 'NONE',  ( 0.3924513946351673721, -1.141110873382124913, 0.4807468720547258823 ) ) ;
#17197 = CARTESIAN_POINT ( 'NONE',  ( 0.5772941663360542375, -1.534806448867990003, -0.4703100941054121353 ) ) ;
#17198 = ORIENTED_EDGE ( 'NONE', *, *, #35147, .T. ) ;
#17199 = CARTESIAN_POINT ( 'NONE',  ( -0.08000000000000000167, -2.504411011601259673, -0.4441669705721119632 ) ) ;
#17200 = ORIENTED_EDGE ( 'NONE', *, *, #6408, .F. ) ;
#17201 = AXIS2_PLACEMENT_3D ( 'NONE', #9100, #21666, #4737 ) ;
#17202 = CARTESIAN_POINT ( 'NONE',  ( 0.1873046210896235908, -0.4547550531002670371, 0.1479976049341028554 ) ) ;
#17203 = AXIS2_PLACEMENT_3D ( 'NONE', #4915, #37001, #26753 ) ;
#17204 = CARTESIAN_POINT ( 'NONE',  ( 0.04867247092399697161, -0.5557472067246875813, 0.2394143140500440414 ) ) ;
#17205 = EDGE_CURVE ( 'NONE', #6967, #33790, #9295, .T. ) ;
#17207 = CARTESIAN_POINT ( 'NONE',  ( 0.08986174638071832421, -0.6039319072276565503, 0.1463024350879380542 ) ) ;
#17206 = CARTESIAN_POINT ( 'NONE',  ( 0.06920015087246249308, -0.5397947987972752104, 0.1394826760052076675 ) ) ;
#17208 = PLANE ( 'NONE',  #23115 ) ;
#17209 = APPLIED_PERSON_AND_ORGANIZATION_ASSIGNMENT ( #3162, #2364, ( #30575 ) ) ;
#17210 = VERTEX_POINT ( 'NONE', #2513 ) ;
#17211 = EDGE_LOOP ( 'NONE', ( #11211, #688, #33523, #6269 ) ) ;
#17212 = CARTESIAN_POINT ( 'NONE',  ( 0.5628430809287441328, -1.504124224925729170, 0.5331533104258753264 ) ) ;
#17213 = CARTESIAN_POINT ( 'NONE',  ( 0.5741976824997229167, -1.499288812830245954, 0.5782747764390164802 ) ) ;
#17214 = VERTEX_POINT ( 'NONE', #14852 ) ;
#17215 = CARTESIAN_POINT ( 'NONE',  ( 0.1399999999999994582, 0.000000000000000000, 0.000000000000000000 ) ) ;
#17216 = CARTESIAN_POINT ( 'NONE',  ( 0.05561375719525241818, -0.4316271021131540264, 0.1617018132803446362 ) ) ;
#17217 = CARTESIAN_POINT ( 'NONE',  ( 0.3818164125050786950, -1.758841887392954995, -0.4494967532450438452 ) ) ;
#17218 = CARTESIAN_POINT ( 'NONE',  ( 0.2336506187151118352, -1.232159623642217872, 0.5021138023866104083 ) ) ;
#17219 = CARTESIAN_POINT ( 'NONE',  ( 0.3991883495211515087, -1.748813394476138372, -0.5227867695449579521 ) ) ;
#17220 = CARTESIAN_POINT ( 'NONE',  ( -0.01548846960707524721, 0.000000000000000000, 0.000000000000000000 ) ) ;
#17221 = CARTESIAN_POINT ( 'NONE',  ( 0.6786648513340227673, -1.399193080605451334, 0.7803980693475389696 ) ) ;
#17222 = DIRECTION ( 'NONE',  ( 1.000000000000000000, -2.549619951388196240E-12, 4.473262954207672140E-13 ) ) ;
#17223 = VECTOR ( 'NONE', #35338, 39.37007874015748143 ) ;
#17224 = CARTESIAN_POINT ( 'NONE',  ( 0.5982289360768325848, -1.580768761966706348, -0.6063568540101081927 ) ) ;
#17225 = CARTESIAN_POINT ( 'NONE',  ( 0.4768848212686895849, -1.682051206446435243, -0.4156371400837835517 ) ) ;
#17226 = CARTESIAN_POINT ( 'NONE',  ( 0.1838283605672264565, -0.5363226265955328698, 0.04314883391416569208 ) ) ;
#17227 = CARTESIAN_POINT ( 'NONE',  ( 0.4343450670606688879, -1.232029114211916854, 0.4817113837480122007 ) ) ;
#17228 = CARTESIAN_POINT ( 'NONE',  ( -0.03309060444528683781, 0.5154120966056447983, -0.07470591001490199667 ) ) ;
#17229 = ADVANCED_FACE ( 'NONE', ( #8050 ), #34222, .F. ) ;
#17230 = CIRCLE ( 'NONE', #189, 0.08000000000000002942 ) ;
#17231 = VECTOR ( 'NONE', #31910, 39.37007874015748143 ) ;
#17232 = DIRECTION ( 'NONE',  ( 1.000000000000000000, 2.403560570595279103E-31, -1.725633230170969455E-31 ) ) ;
#17233 = CARTESIAN_POINT ( 'NONE',  ( 0.5872508345537166274, -1.538326194691165050, -0.6180035471177106610 ) ) ;
#17234 = AXIS2_PLACEMENT_3D ( 'NONE', #26025, #22934, #3789 ) ;
#17235 = ADVANCED_FACE ( 'NONE', ( #27417 ), #17534, .T. ) ;
#17236 = CARTESIAN_POINT ( 'NONE',  ( 0.03113248654051816583, -0.2940959072101921867, -0.05922497245433272495 ) ) ;
#17237 = DIRECTION ( 'NONE',  ( 0.01455087615875041117, 0.9998941303973198913, 0.000000000000000000 ) ) ;
#17238 = CARTESIAN_POINT ( 'NONE',  ( -0.04760454375021173912, -0.3171166672795114883, 0.3633054878239699303 ) ) ;
#17239 = ADVANCED_FACE ( 'NONE', ( #30484, #3724 ), #21642, .F. ) ;
#17240 = VERTEX_POINT ( 'NONE', #31697 ) ;
#17241 = ORIENTED_EDGE ( 'NONE', *, *, #5721, .F. ) ;
#17242 = CARTESIAN_POINT ( 'NONE',  ( 0.4763501221259694440, -1.554011115824661893, -0.5166151207188711680 ) ) ;
#17243 = CARTESIAN_POINT ( 'NONE',  ( 0.1434010736994648927, -1.283284918233685623, 0.5707417262808780478 ) ) ;
#17244 = ORIENTED_EDGE ( 'NONE', *, *, #28025, .F. ) ;
#17245 = FACE_OUTER_BOUND ( 'NONE', #17690, .T. ) ;
#17246 = CARTESIAN_POINT ( 'NONE',  ( 0.01548846960707370504, 0.2450655194479869625, -0.4674710490749294234 ) ) ;
#17247 = CARTESIAN_POINT ( 'NONE',  ( 0.5552441641573474529, -1.389167795574909547, 0.5900859616208992131 ) ) ;
#17249 = EDGE_LOOP ( 'NONE', ( #25565, #5707, #39158, #13344 ) ) ;
#17248 = DIRECTION ( 'NONE',  ( 0.000000000000000000, 0.000000000000000000, -1.000000000000000000 ) ) ;
#17250 = CARTESIAN_POINT ( 'NONE',  ( 0.5134194225791607336, -1.118797547403455273, 0.5580923141791981346 ) ) ;
#17251 = CARTESIAN_POINT ( 'NONE',  ( 0.03309057659885114577, 0.5154121718708729594, -0.07470590733143775419 ) ) ;
#17252 = ORIENTED_EDGE ( 'NONE', *, *, #31579, .T. ) ;
#17253 = CYLINDRICAL_SURFACE ( 'NONE', #10689, 0.01499999999999999424 ) ;
#17254 = CARTESIAN_POINT ( 'NONE',  ( 0.3224727725618313778, -1.601339809662290614, 0.7774851842373180499 ) ) ;
#17255 = EDGE_CURVE ( 'NONE', #2786, #27821, #3516, .T. ) ;
#17257 = CARTESIAN_POINT ( 'NONE',  ( 0.1875666489605907761, -0.5533060011614776563, 0.04426231146092830110 ) ) ;
#17256 = CARTESIAN_POINT ( 'NONE',  ( 0.6910102488910387919, -1.503481276490886254, 0.4663957319702505822 ) ) ;
#17258 = DIRECTION ( 'NONE',  ( 0.000000000000000000, 0.000000000000000000, 1.000000000000000000 ) ) ;
#17259 = AXIS2_PLACEMENT_3D ( 'NONE', #21225, #33763, #30260 ) ;
#17260 = CYLINDRICAL_SURFACE ( 'NONE', #826, 0.1033070866141734129 ) ;
#17261 = ORIENTED_EDGE ( 'NONE', *, *, #488, .F. ) ;
#17262 = DIRECTION ( 'NONE',  ( -1.000000000000000000, 0.000000000000000000, 0.000000000000000000 ) ) ;
#17263 = DIRECTION ( 'NONE',  ( 0.000000000000000000, 0.000000000000000000, 1.000000000000000000 ) ) ;
#17264 = CARTESIAN_POINT ( 'NONE',  ( -0.3000000000000000999, -2.853330612949663170, -0.6088139570729240724 ) ) ;
#17265 = AXIS2_PLACEMENT_3D ( 'NONE', #36403, #8008, #8416 ) ;
#17266 = CIRCLE ( 'NONE', #40243, 0.01500000000000004108 ) ;
#17267 = CARTESIAN_POINT ( 'NONE',  ( 0.4388835414683293634, -1.230108148053269179, 0.5682417262808738823 ) ) ;
#17268 = CARTESIAN_POINT ( 'NONE',  ( 0.1617959581636433664, -1.277479963088032244, -0.3330842537329358199 ) ) ;
#17269 = AXIS2_PLACEMENT_3D ( 'NONE', #40528, #5758, #12348 ) ;
#17270 = CARTESIAN_POINT ( 'NONE',  ( -0.1680316146028532909, 0.5219773800263015628, 0.3170215181389818837 ) ) ;
#17271 = CARTESIAN_POINT ( 'NONE',  ( -0.1684323897529161340, 0.5231977509870414655, 0.3108929459560476061 ) ) ;
#17272 = DIRECTION ( 'NONE',  ( 1.000000000000000000, 0.000000000000000000, 0.000000000000000000 ) ) ;
#17273 = CARTESIAN_POINT ( 'NONE',  ( 0.3558973088851713484, -1.163486677007739667, 0.4185315289370134528 ) ) ;
#17274 = AXIS2_PLACEMENT_3D ( 'NONE', #38017, #32228, #35138 ) ;
#17275 = DIRECTION ( 'NONE',  ( -1.000000000000000000, 0.000000000000000000, 0.000000000000000000 ) ) ;
#17276 = CARTESIAN_POINT ( 'NONE',  ( 0.2196639771989866430, -1.182743154750227843, -0.5155029497116575543 ) ) ;
#17277 = CARTESIAN_POINT ( 'NONE',  ( 0.3974763075531499990, -1.145280806970993659, 0.4306062601161479431 ) ) ;
#17278 = CARTESIAN_POINT ( 'NONE',  ( 0.1837824601350801224, -1.244685677561853554, -0.4092841885321224504 ) ) ;
#17279 = DIRECTION ( 'NONE',  ( 1.188678714063518227E-15, -1.000000000000000000, -3.263080277421930985E-16 ) ) ;
#17280 = EDGE_CURVE ( 'NONE', #23808, #27248, #14549, .T. ) ;
#17281 = CARTESIAN_POINT ( 'NONE',  ( 0.01182178933247767828, -0.6030406541726748282, -0.09969815838237815198 ) ) ;
#17282 = DIRECTION ( 'NONE',  ( -1.000000000000000000, -0.000000000000000000, -0.000000000000000000 ) ) ;
#17283 = CIRCLE ( 'NONE', #14634, 0.2500000000000000000 ) ;
#17284 = EDGE_CURVE ( 'NONE', #4940, #25265, #30787, .T. ) ;
#17285 = DIRECTION ( 'NONE',  ( 5.551115123125956498E-17, 0.000000000000000000, -1.000000000000000000 ) ) ;
#17286 = DIRECTION ( 'NONE',  ( 1.000000000000000000, -0.000000000000000000, -0.000000000000000000 ) ) ;
#17287 = ORIENTED_EDGE ( 'NONE', *, *, #7884, .T. ) ;
#17288 = ORIENTED_EDGE ( 'NONE', *, *, #34609, .T. ) ;
#17289 = AXIS2_PLACEMENT_3D ( 'NONE', #23228, #4068, #19714 ) ;
#17290 = DIRECTION ( 'NONE',  ( 0.000000000000000000, 3.330669073875470114E-16, 1.000000000000000000 ) ) ;
#17291 = EDGE_LOOP ( 'NONE', ( #12499, #20206, #10367, #6440 ) ) ;
#17292 = EDGE_CURVE ( 'NONE', #38276, #9616, #37541, .T. ) ;
#17293 = LINE ( 'NONE', #36418, #35483 ) ;
#17295 = ORIENTED_EDGE ( 'NONE', *, *, #1420, .F. ) ;
#17294 = CARTESIAN_POINT ( 'NONE',  ( 0.2008624261879642658, -0.7759890251660743754, 0.5855711181173813840 ) ) ;
#17297 = ORIENTED_EDGE ( 'NONE', *, *, #36503, .F. ) ;
#17296 = CARTESIAN_POINT ( 'NONE',  ( -0.001637768206801153191, -0.8343066215553702758, 0.06341441842760701941 ) ) ;
#17298 = VERTEX_POINT ( 'NONE', #5974 ) ;
#17299 = CARTESIAN_POINT ( 'NONE',  ( 0.5253935478925986224, -1.258261529843748727, 0.9008978830525721238 ) ) ;
#17300 = ORIENTED_EDGE ( 'NONE', *, *, #28811, .F. ) ;
#17301 = EDGE_CURVE ( 'NONE', #37987, #15898, #34771, .T. ) ;
#17302 = CARTESIAN_POINT ( 'NONE',  ( 0.2479547223653777166, -1.576436051040469355, 0.8688751265680482172 ) ) ;
#17304 = CARTESIAN_POINT ( 'NONE',  ( 0.4497590084914004360, -1.610781099968991992, -0.3722728953286537634 ) ) ;
#17303 = DIRECTION ( 'NONE',  ( -1.000000000000000000, -2.280301054154495132E-31, 1.664003471950577689E-31 ) ) ;
#17305 = CARTESIAN_POINT ( 'NONE',  ( 0.6303272460286932777, -1.599106815577767904, -0.4488814048484467967 ) ) ;
#17306 = EDGE_CURVE ( 'NONE', #22862, #21137, #37877, .T. ) ;
#17307 = CARTESIAN_POINT ( 'NONE',  ( -0.0001922331839921582748, -0.4210325180397646583, 0.1483282180229311964 ) ) ;
#17309 = VERTEX_POINT ( 'NONE', #28621 ) ;
#17308 = VERTEX_POINT ( 'NONE', #40341 ) ;
#17310 = ADVANCED_FACE ( 'NONE', ( #9877 ), #31073, .T. ) ;
#17311 = CARTESIAN_POINT ( 'NONE',  ( 0.2187263053623307030, -0.9276774108102062710, 0.6425196885543180692 ) ) ;
#17312 = DIRECTION ( 'NONE',  ( 0.4999551463232373427, -0.8660512985181134660, 0.000000000000000000 ) ) ;
#17313 = CARTESIAN_POINT ( 'NONE',  ( 0.1125434483652356515, -0.6674345388938710544, 0.4183932267472516564 ) ) ;
#17314 = CARTESIAN_POINT ( 'NONE',  ( 0.5507456769299096111, -1.501809185380300393, 0.6702287185426054616 ) ) ;
#17315 = EDGE_CURVE ( 'NONE', #31663, #2486, #16090, .T. ) ;
#17316 = CARTESIAN_POINT ( 'NONE',  ( 0.1972041951826758455, -0.5769445034669802297, 0.3142228439387118599 ) ) ;
#17317 = CARTESIAN_POINT ( 'NONE',  ( 4.780733988912460139E-16, 0.2949999999999991518, -7.512581982576723358E-16 ) ) ;
#17318 = CARTESIAN_POINT ( 'NONE',  ( 0.3211332658540719254, -1.297355586764235236, 0.4182417297899396202 ) ) ;
#17319 = CIRCLE ( 'NONE', #16672, 0.01499999999999995781 ) ;
#17320 = CARTESIAN_POINT ( 'NONE',  ( 0.4084093395596710141, -1.687879686225770781, -0.4185105672228304208 ) ) ;
#17321 = DIRECTION ( 'NONE',  ( -0.1871397384865028379, -0.9823333030490229989, -6.060229385358974537E-17 ) ) ;
#17322 = FACE_OUTER_BOUND ( 'NONE', #18621, .T. ) ;
#17323 = CONICAL_SURFACE ( 'NONE', #311, 0.1400000000000009570, 1.047197551196600962 ) ;
#17324 = DIRECTION ( 'NONE',  ( -9.860761315262614725E-32, -0.9849933812516262766, 0.1725921171157263345 ) ) ;
#17325 = AXIS2_PLACEMENT_3D ( 'NONE', #4077, #3696, #22849 ) ;
#17326 = CARTESIAN_POINT ( 'NONE',  ( 0.01138001396866243804, -0.9310208032443704207, 0.05798820300846099784 ) ) ;
#17327 = CARTESIAN_POINT ( 'NONE',  ( 0.4351293263873937667, -1.231514889939106849, 0.5832342842089121016 ) ) ;
#17328 = CARTESIAN_POINT ( 'NONE',  ( -0.02000000000000000042, -2.545097362529205487, -0.2282911599260125379 ) ) ;
#17329 = DIRECTION ( 'NONE',  ( 5.551115123125703816E-17, -5.306893166658304503E-16, -1.000000000000000000 ) ) ;
#17330 = CARTESIAN_POINT ( 'NONE',  ( 0.1209218709639075517, -1.413449759333152755, 0.6688053819537839173 ) ) ;
#17331 = CARTESIAN_POINT ( 'NONE',  ( 0.4679067357895266843, -1.070896998011005019, 0.6479521087143890190 ) ) ;
#17332 = DATE_AND_TIME ( #23928, #3639 ) ;
#17333 = CARTESIAN_POINT ( 'NONE',  ( 0.1907823988372855106, -0.4944553380418882926, 0.2959634315342150046 ) ) ;
#17334 = AXIS2_PLACEMENT_3D ( 'NONE', #13627, #38716, #10748 ) ;
#17335 = EDGE_CURVE ( 'NONE', #30976, #12637, #9321, .T. ) ;
#17336 = DIRECTION ( 'NONE',  ( -0.4999551463232372317, 0.8660512985181135770, -0.000000000000000000 ) ) ;
#17337 = EDGE_CURVE ( 'NONE', #39958, #35001, #19182, .T. ) ;
#17338 = CARTESIAN_POINT ( 'NONE',  ( -0.07216878364870325802, 0.05141091571461162829, -0.1249999999999999029 ) ) ;
#17339 = ORIENTED_EDGE ( 'NONE', *, *, #32105, .T. ) ;
#17340 = CARTESIAN_POINT ( 'NONE',  ( 0.3424206644552083567, -1.681860750042348807, -0.5668114887320723216 ) ) ;
#17341 = CARTESIAN_POINT ( 'NONE',  ( 0.04683743026951789346, -0.8297330588939687557, 0.7132132020604889933 ) ) ;
#17342 = B_SPLINE_CURVE_WITH_KNOTS ( 'NONE', 3,
 ( #38177, #29127, #988, #37780, #31605, #32011, #3420, #28733, #9795, #19870 ),
 .UNSPECIFIED., .F., .F.,
 ( 4, 2, 2, 2, 4 ),
 ( 0.000000000000000000, 0.0007746574062662862307, 0.001549314812532572461, 0.002323972218798858909, 0.003098629625065144923 ),
 .UNSPECIFIED. ) ;
#17343 = AXIS2_PLACEMENT_3D ( 'NONE', #18665, #31228, #9395 ) ;
#17344 = CARTESIAN_POINT ( 'NONE',  ( 0.08271545042603034581, -1.307985630826135059, 0.4687282396759575587 ) ) ;
#17346 = ORIENTED_EDGE ( 'NONE', *, *, #12395, .T. ) ;
#17345 = CARTESIAN_POINT ( 'NONE',  ( 0.2421510470436483708, -1.227192766047864758, 0.5682417262808779901 ) ) ;
#17347 = CYLINDRICAL_SURFACE ( 'NONE', #26516, 0.06250000000000001388 ) ;
#17348 = CARTESIAN_POINT ( 'NONE',  ( 0.2318926187578342901, -0.6847811903715324000, 0.4821206442548801596 ) ) ;
#17350 = VERTEX_POINT ( 'NONE', #31491 ) ;
#17349 = ORIENTED_EDGE ( 'NONE', *, *, #7196, .T. ) ;
#17351 = CARTESIAN_POINT ( 'NONE',  ( 0.0005182934561807130700, -1.951317934876418914, -0.6895229178506784296 ) ) ;
#17352 = VECTOR ( 'NONE', #30553, 39.37007874015748143 ) ;
#17353 = AXIS2_PLACEMENT_3D ( 'NONE', #38041, #22232, #16435 ) ;
#17354 = CARTESIAN_POINT ( 'NONE',  ( 0.05634304521267768928, -2.731847993664263218E-15, -0.4588823192046729837 ) ) ;
#17355 = PRODUCT_DEFINITION_SHAPE ( 'NONE', 'NONE',  #11166 ) ;
#17356 = CARTESIAN_POINT ( 'NONE',  ( -0.2399999999999999079, -3.216935334666387813, -0.6321346234654038332 ) ) ;
#17357 = PERSON_AND_ORGANIZATION ( #28500, #32463 ) ;
#17358 = CARTESIAN_POINT ( 'NONE',  ( -0.04760454375021105911, 0.4700983808485347248, -0.1075238135162311093 ) ) ;
#17359 = ORIENTED_EDGE ( 'NONE', *, *, #14316, .T. ) ;
#17360 = CARTESIAN_POINT ( 'NONE',  ( 0.08670746357302318297, -1.302632728992202837, 0.5759743761708646659 ) ) ;
#17361 = CARTESIAN_POINT ( 'NONE',  ( 0.1293136892229509449, -0.7528337723472907639, 0.4737154814036002026 ) ) ;
#17362 = AXIS2_PLACEMENT_3D ( 'NONE', #23584, #22965, #7509 ) ;
#17363 = CARTESIAN_POINT ( 'NONE',  ( 0.2758292747667600575, -1.561373478687104743, 0.9870382891917031110 ) ) ;
#17364 = CARTESIAN_POINT ( 'NONE',  ( 0.09869151381832386161, -0.5631343475376648922, 0.2335645800241998582 ) ) ;
#17365 = AXIS2_PLACEMENT_3D ( 'NONE', #39280, #30032, #4317 ) ;
#17367 = CARTESIAN_POINT ( 'NONE',  ( 0.3181856309082868317, -1.645723040471628762, 0.6029037648573117858 ) ) ;
#17366 = CARTESIAN_POINT ( 'NONE',  ( 0.1132205867452878156, -0.6714125266378772050, -0.09528610095238206068 ) ) ;
#17368 = CARTESIAN_POINT ( 'NONE',  ( 0.09699292618303559377, -0.9356975710665345058, 0.2689778393378690069 ) ) ;
#17369 = ORIENTED_EDGE ( 'NONE', *, *, #19356, .T. ) ;
#17370 = VERTEX_POINT ( 'NONE', #15859 ) ;
#17371 = DIRECTION ( 'NONE',  ( 0.5741533254374902029, 0.3983735212876081122, -0.7152946920158034239 ) ) ;
#17372 = CARTESIAN_POINT ( 'NONE',  ( 0.1177181460812074948, -0.4737793742729833890, 0.2761546688069523858 ) ) ;
#17373 = DIRECTION ( 'NONE',  ( 1.000000000000000000, 0.000000000000000000, 0.000000000000000000 ) ) ;
#17374 = CARTESIAN_POINT ( 'NONE',  ( -0.02953079040095612021, -0.5250338024619279897, -0.07436286310882828099 ) ) ;
#17375 = CONICAL_SURFACE ( 'NONE', #25247, 0.1600000000000006417, 1.047197551196599408 ) ;
#17376 = CARTESIAN_POINT ( 'NONE',  ( 0.07069647374262323647, -1.314947515254170307, 0.5019162079743227922 ) ) ;
#17377 = VECTOR ( 'NONE', #1072, 39.37007874015748143 ) ;
#17378 = CARTESIAN_POINT ( 'NONE',  ( 0.4058326211045913401, -1.732063036044662274, -0.4894232243292900852 ) ) ;
#17379 = DIRECTION ( 'NONE',  ( -8.881784197001245421E-16, 2.361472542561082612E-16, -1.000000000000000000 ) ) ;
#17380 = CARTESIAN_POINT ( 'NONE',  ( 0.6183701179687098870, -1.298963174629117479, 0.5817474467243960445 ) ) ;
#17381 = CIRCLE ( 'NONE', #39047, 0.01500000000000003934 ) ;
#17382 = DIRECTION ( 'NONE',  ( 1.000000000000000000, 2.465190328815662439E-32, 0.000000000000000000 ) ) ;
#17383 = DIRECTION ( 'NONE',  ( -0.4413459890218811021, 0.8973370147131440877, 0.000000000000000000 ) ) ;
#17384 = LINE ( 'NONE', #36095, #23894 ) ;
#17385 = CARTESIAN_POINT ( 'NONE',  ( -0.05464101615137786222, -2.332630956013932888, -0.5701767140373721343 ) ) ;
#17386 = CARTESIAN_POINT ( 'NONE',  ( -0.08000000000000000167, -2.313818782766725146, -0.3979462133327477114 ) ) ;
#17387 = CIRCLE ( 'NONE', #2276, 0.9237847906030128842 ) ;
#17388 = CARTESIAN_POINT ( 'NONE',  ( -0.04229883635637923800, -0.2719170545448721388, -0.3816769773555965806 ) ) ;
#17389 = ORIENTED_EDGE ( 'NONE', *, *, #40139, .T. ) ;
#17390 = CARTESIAN_POINT ( 'NONE',  ( 0.4040203406124813212, -0.9939942186036138105, 0.7028486825154387496 ) ) ;
#17391 = CARTESIAN_POINT ( 'NONE',  ( 0.5207218691171461300, -1.171053392212251021, 0.4666017006239680520 ) ) ;
#17392 = DIRECTION ( 'NONE',  ( 7.771561172376107616E-16, -7.170354002788761615E-17, 1.000000000000000000 ) ) ;
#17393 = CARTESIAN_POINT ( 'NONE',  ( 0.05122501923433656068, -0.8846498927777804999, 0.5029692314556662991 ) ) ;
#17394 = VERTEX_POINT ( 'NONE', #28409 ) ;
#17395 = CARTESIAN_POINT ( 'NONE',  ( 0.04293317454820616552, 0.2295413494973359003, 0.4381202835071925650 ) ) ;
#17396 = CARTESIAN_POINT ( 'NONE',  ( 0.02881408050861127002, 0.06014027758172069138, 0.4945500181289073649 ) ) ;
#17397 = DIRECTION ( 'NONE',  ( -1.000000000000000000, 0.000000000000000000, 0.000000000000000000 ) ) ;
#17398 = SPHERICAL_SURFACE ( 'NONE', #10150, 0.01499999999999999944 ) ;
#17399 = CIRCLE ( 'NONE', #12152, 0.2000000000000000389 ) ;
#17400 = CARTESIAN_POINT ( 'NONE',  ( 0.4023727053442279766, -1.150481506616649607, 0.6972092212261085109 ) ) ;
#17402 = CARTESIAN_POINT ( 'NONE',  ( 0.4828795985232906540, -1.118743695481591915, 0.5686671663553843903 ) ) ;
#17401 = DIRECTION ( 'NONE',  ( 1.188678714063518227E-15, -1.000000000000000000, -3.263080277421930985E-16 ) ) ;
#17403 = CARTESIAN_POINT ( 'NONE',  ( -0.04293701532779585495, -0.2295363440003029276, -0.4381116105132951688 ) ) ;
#17404 = EDGE_LOOP ( 'NONE', ( #30847, #4934, #8199, #32366 ) ) ;
#17405 = AXIS2_PLACEMENT_3D ( 'NONE', #24358, #17582, #21279 ) ;
#17406 = CARTESIAN_POINT ( 'NONE',  ( 7.512581982576723358E-16, -0.2981948553318921613, -3.414809992080329023E-16 ) ) ;
#17407 = ORIENTED_EDGE ( 'NONE', *, *, #23002, .F. ) ;
#17408 = CIRCLE ( 'NONE', #19395, 0.5543128707267515054 ) ;
#17409 = CARTESIAN_POINT ( 'NONE',  ( 0.4159916692016358830, -1.069406866067976081, -0.5155029497116575543 ) ) ;
#17410 = CARTESIAN_POINT ( 'NONE',  ( 0.06359643539015311098, -0.5791250426409843000, 0.2975846012595457779 ) ) ;
#17412 = CARTESIAN_POINT ( 'NONE',  ( 0.1937362933224030803, -0.7983156727584820311, 0.2891542942581120657 ) ) ;
#17411 = CARTESIAN_POINT ( 'NONE',  ( 0.06671632896744131291, -0.6969372051195925621, -0.001946471286827283678 ) ) ;
#17413 = CARTESIAN_POINT ( 'NONE',  ( 0.1637585665034339832, -0.5994899851647166322, 0.1022936816274461203 ) ) ;
#17414 = SECURITY_CLASSIFICATION ( '', '', #15408 ) ;
#17415 = EDGE_LOOP ( 'NONE', ( #10058, #17680, #132, #9289 ) ) ;
#17416 = ORIENTED_EDGE ( 'NONE', *, *, #36565, .T. ) ;
#17417 = DIRECTION ( 'NONE',  ( -0.4999551463232373427, 0.8660512985181134660, -0.000000000000000000 ) ) ;
#17418 = CARTESIAN_POINT ( 'NONE',  ( 0.5739118490517725046, -1.499259023535516988, 0.5731568487034417458 ) ) ;
#17419 = APPLICATION_CONTEXT ( 'configuration controlled 3d designs of mechanical parts and assemblies' ) ;
#17420 = ORIENTED_EDGE ( 'NONE', *, *, #3161, .T. ) ;
#17421 = AXIS2_PLACEMENT_3D ( 'NONE', #36339, #33453, #11248 ) ;
#17422 = CARTESIAN_POINT ( 'NONE',  ( 0.6017231405399463551, -1.610171036770066122, 0.5941483199617545452 ) ) ;
#17423 = CARTESIAN_POINT ( 'NONE',  ( 0.04308558661660559508, -0.4494156853470195334, 0.2058346122080974006 ) ) ;
#17424 =( BOUNDED_SURFACE ( )  B_SPLINE_SURFACE ( 3, 2, ( 
 ( #27278, #39810, #33620 ),
 ( #8944, #12035, #2774 ),
 ( #28268, #27880, #18205 ),
 ( #2573, #31553, #24805 ) ),
 .UNSPECIFIED., .F., .F., .F. ) 
 B_SPLINE_SURFACE_WITH_KNOTS ( ( 4, 4 ),
 ( 3, 3 ),
 ( 0.0007843053012490898077, 0.001168341556843950548 ),
 ( 0.000000000000000000, 1.000000000000000000 ),
 .UNSPECIFIED. ) 
 GEOMETRIC_REPRESENTATION_ITEM ( )  RATIONAL_B_SPLINE_SURFACE ( (
 ( 1.000000000000000000, 0.9117915798263158678, 1.000000000000000000),
 ( 1.000000000000000000, 0.9032018617293362528, 1.000000000000000000),
 ( 1.000000000000000000, 0.8990088477696482894, 1.000000000000000000),
 ( 1.000000000000000000, 0.8989970956542941982, 1.000000000000000000) ) ) 
 REPRESENTATION_ITEM ( '' )  SURFACE ( )  );
#17425 = CARTESIAN_POINT ( 'NONE',  ( 0.6335034394193310714, -1.559158136216843404, 0.4182417262808776903 ) ) ;
#17426 = CARTESIAN_POINT ( 'NONE',  ( 0.1524794451307193710, -1.279078254004480053, 0.4205905341015664378 ) ) ;
#17427 = CARTESIAN_POINT ( 'NONE',  ( 0.4003286058064897679, -1.748155145941718169, -0.5147095092643340086 ) ) ;
#17428 = EDGE_CURVE ( 'NONE', #22034, #20195, #32962, .T. ) ;
#17429 = CARTESIAN_POINT ( 'NONE',  ( 0.08845320025402096664, -0.5635964745544715937, 0.02268293738053128727 ) ) ;
#17430 = EDGE_CURVE ( 'NONE', #35502, #29923, #31688, .T. ) ;
#17431 = CARTESIAN_POINT ( 'NONE',  ( 0.1875104876115774588, -0.4605130342159906021, 0.1706505080850997946 ) ) ;
#17432 = DIRECTION ( 'NONE',  ( -1.000000000000000000, 0.000000000000000000, -7.515112548955566195E-16 ) ) ;
#17433 = CARTESIAN_POINT ( 'NONE',  ( 0.6010916754805513129, -1.596410883951256965, -0.5227362160200681451 ) ) ;
#17434 = AXIS2_PLACEMENT_3D ( 'NONE', #4856, #8157, #1217 ) ;
#17435 = CARTESIAN_POINT ( 'NONE',  ( 0.03672447062657503702, 0.3146083306767443188, 0.3636032511890208707 ) ) ;
#17436 = CARTESIAN_POINT ( 'NONE',  ( 0.6475056143351221039, -1.571742384113670621, 0.6112107622448768041 ) ) ;
#17437 = CARTESIAN_POINT ( 'NONE',  ( -0.2746410161513782033, -1.739646749720735741, -0.3661865639197241507 ) ) ;
#17438 = DIRECTION ( 'NONE',  ( -1.000000000000000000, -0.000000000000000000, -0.000000000000000000 ) ) ;
#17439 = EDGE_CURVE ( 'NONE', #9666, #18610, #29681, .T. ) ;
#17440 = APPLIED_APPROVAL_ASSIGNMENT ( #20757, ( #1014 ) ) ;
#17441 = APPLIED_PERSON_AND_ORGANIZATION_ASSIGNMENT ( #7450, #8271, ( #40563 ) ) ;
#17442 = CARTESIAN_POINT ( 'NONE',  ( 0.3137727395043992673, -1.722325404801505089, 0.8203598276066251804 ) ) ;
#17443 = CARTESIAN_POINT ( 'NONE',  ( 0.6050257157783865969, -1.526910860915171364, -0.5980336084688177012 ) ) ;
#17444 = CARTESIAN_POINT ( 'NONE',  ( 0.1131241454731939100, -0.6872203660140440151, -0.09530310615070609892 ) ) ;
#17445 = CARTESIAN_POINT ( 'NONE',  ( 0.4718448929443245232, -1.683416021769955861, 0.5701492720201403186 ) ) ;
#17446 = CARTESIAN_POINT ( 'NONE',  ( -0.05269191099235827347, -0.2718205810683996804, 0.3817379850160088073 ) ) ;
#17447 = B_SPLINE_CURVE_WITH_KNOTS ( 'NONE', 3,
 ( #3547, #16500, #13618, #32136 ),
 .UNSPECIFIED., .F., .F.,
 ( 4, 4 ),
 ( 1.081944681729554441E-16, 0.0007979876146421405712 ),
 .UNSPECIFIED. ) ;
#17448 = AXIS2_PLACEMENT_3D ( 'NONE', #21643, #30884, #34166 ) ;
#17449 = ORIENTED_EDGE ( 'NONE', *, *, #5936, .T. ) ;
#17450 = ORIENTED_EDGE ( 'NONE', *, *, #32637, .T. ) ;
#17451 = CARTESIAN_POINT ( 'NONE',  ( -0.2746410161513782033, -2.183180860297908144, -0.4937760292030871079 ) ) ;
#17452 = CARTESIAN_POINT ( 'NONE',  ( 0.3644961020528623141, -1.765334207956099632, -0.5888949161622180073 ) ) ;
#17453 = VERTEX_POINT ( 'NONE', #7800 ) ;
#17454 = CARTESIAN_POINT ( 'NONE',  ( -0.1167294259372888832, -0.5331983348239500708, 0.1528658435937002014 ) ) ;
#17455 = CARTESIAN_POINT ( 'NONE',  ( -0.04582889109739289590, 0.2312034125369032966, -0.4285435303321075695 ) ) ;
#17456 = CARTESIAN_POINT ( 'NONE',  ( 0.5337193422410454469, -1.352074988199290617, 0.5876441216552129587 ) ) ;
#17458 = ORIENTED_EDGE ( 'NONE', *, *, #35406, .F. ) ;
#17457 = CARTESIAN_POINT ( 'NONE',  ( -0.1613941803225978633, 0.5013693709968672918, 0.1260513636289611328 ) ) ;
#17459 = CARTESIAN_POINT ( 'NONE',  ( 0.2706875035899702353, -0.8747201880513900685, 0.5443116846754595395 ) ) ;
#17460 = DIRECTION ( 'NONE',  ( 0.4999999999999988343, 0.000000000000000000, -0.8660254037844393737 ) ) ;
#17461 = ORIENTED_EDGE ( 'NONE', *, *, #13715, .F. ) ;
#17462 = SPHERICAL_SURFACE ( 'NONE', #33669, 0.01499999999999999944 ) ;
#17463 = CARTESIAN_POINT ( 'NONE',  ( 0.02497539211394332256, -0.5654553311636884017, 0.2802127003532230431 ) ) ;
#17465 = CARTESIAN_POINT ( 'NONE',  ( 0.1770450918743750601, -0.4681907750250927647, 0.07469303172640867627 ) ) ;
#17464 = CARTESIAN_POINT ( 'NONE',  ( 0.6781574892493564821, -1.522851489271323189, 0.4444256985947928063 ) ) ;
#17466 = CARTESIAN_POINT ( 'NONE',  ( 0.4093611158985690501, -1.131941421409890403, 0.5197417262808780025 ) ) ;
#17467 = DIRECTION ( 'NONE',  ( -0.3779644730092284188, 0.9258200997725509751, 0.000000000000000000 ) ) ;
#17468 = ORIENTED_EDGE ( 'NONE', *, *, #14962, .T. ) ;
#17469 = AXIS2_PLACEMENT_3D ( 'NONE', #34452, #24200, #24389 ) ;
#17470 = CIRCLE ( 'NONE', #31281, 0.08249999999977555842 ) ;
#17471 = FACE_OUTER_BOUND ( 'NONE', #29356, .T. ) ;
#17472 = EDGE_CURVE ( 'NONE', #26954, #36862, #4508, .T. ) ;
#17473 = LINE ( 'NONE', #33097, #15472 ) ;
#17474 = CARTESIAN_POINT ( 'NONE',  ( 0.08825382088300037786, -0.8443243380302292156, 0.3515346555839444220 ) ) ;
#17475 = PRODUCT_DEFINITION_FORMATION_WITH_SPECIFIED_SOURCE ( 'ANY', '', #35397, .NOT_KNOWN. ) ;
#17476 = CARTESIAN_POINT ( 'NONE',  ( 0.3323178337258445580, -1.749637176862759880, 0.4593294054832028350 ) ) ;
#17477 = ADVANCED_FACE ( 'NONE', ( #29617 ), #40183, .F. ) ;
#17478 = CARTESIAN_POINT ( 'NONE',  ( 0.4159916692016358830, -1.069406866067976081, -0.5155029497116575543 ) ) ;
#17479 = EDGE_CURVE ( 'NONE', #26954, #19390, #2759, .T. ) ;
#17480 = ADVANCED_FACE ( 'NONE', ( #38673 ), #4105, .T. ) ;
#17481 = AXIS2_PLACEMENT_3D ( 'NONE', #2212, #8557, #29567 ) ;
#17482 = CARTESIAN_POINT ( 'NONE',  ( -0.02587796518899032269, 2.459870571432321995E-16, 0.5399999999999999245 ) ) ;
#17483 = CARTESIAN_POINT ( 'NONE',  ( -0.1126900943766889623, -0.5191528597923187327, 0.1491007326289494894 ) ) ;
#17484 = CARTESIAN_POINT ( 'NONE',  ( 0.03113248654051816583, 0.000000000000000000, 0.000000000000000000 ) ) ;
#17485 = CARTESIAN_POINT ( 'NONE',  ( 0.2511799810870077310, -1.337738304023724512, -0.3144976166544468099 ) ) ;
#17486 = CARTESIAN_POINT ( 'NONE',  ( -0.02000000000000000042, -2.281505296119629378, -0.5332679964655872018 ) ) ;
#17487 = PERSON_AND_ORGANIZATION_ROLE ( 'design_owner' ) ;
#17488 = CARTESIAN_POINT ( 'NONE',  ( 0.4168500870363872068, -1.141030447601083742, 0.4330279073753918739 ) ) ;
#17489 = CARTESIAN_POINT ( 'NONE',  ( 0.04229956186878531393, -0.4483852441756314144, 0.1364680347311799102 ) ) ;
#17490 = CARTESIAN_POINT ( 'NONE',  ( 0.7083987901907250473, -1.516814183290504214, 0.5551003832434545648 ) ) ;
#17491 = EDGE_CURVE ( 'NONE', #11991, #2287, #17868, .T. ) ;
#17492 = APPLIED_PERSON_AND_ORGANIZATION_ASSIGNMENT ( #5117, #33940, ( #22018 ) ) ;
#17493 = CARTESIAN_POINT ( 'NONE',  ( 0.01221484228109331709, -0.4284514069139452874, 0.1505827212209437382 ) ) ;
#17494 = CARTESIAN_POINT ( 'NONE',  ( 0.4246513848252074785, -1.105208224189071942, 0.5933906341394227235 ) ) ;
#17495 = CARTESIAN_POINT ( 'NONE',  ( -0.1196588179077709702, -0.4996288669916955083, 0.3264677846082026380 ) ) ;
#17496 = VECTOR ( 'NONE', #27540, 39.37007874015748143 ) ;
#17497 = CARTESIAN_POINT ( 'NONE',  ( -0.02000000000000000042, -1.518907846805490403, -0.1889969338327479598 ) ) ;
#17498 = VERTEX_POINT ( 'NONE', #32891 ) ;
#17499 = VERTEX_POINT ( 'NONE', #20175 ) ;
#17500 = CARTESIAN_POINT ( 'NONE',  ( 0.4226000438817392180, -1.709616762427842218, 0.4282184315516496809 ) ) ;
#17501 = VERTEX_POINT ( 'NONE', #38480 ) ;
#17502 = EDGE_CURVE ( 'NONE', #37027, #33332, #40288, .T. ) ;
#17503 = FACE_OUTER_BOUND ( 'NONE', #7860, .T. ) ;
#17504 = CARTESIAN_POINT ( 'NONE',  ( 0.5512873130268265420, -1.413716574473140142, 0.7672181155003892083 ) ) ;
#17506 = EDGE_LOOP ( 'NONE', ( #21979, #17510, #8500, #32988 ) ) ;
#17505 = CARTESIAN_POINT ( 'NONE',  ( 0.0002045689356396978231, -0.6663330284319074481, -0.01264868658114923390 ) ) ;
#17507 = AXIS2_PLACEMENT_3D ( 'NONE', #932, #10147, #28456 ) ;
#17508 = ORIENTED_EDGE ( 'NONE', *, *, #36044, .F. ) ;
#17509 = CYLINDRICAL_SURFACE ( 'NONE', #25798, 0.1946589359789743512 ) ;
#17510 = ORIENTED_EDGE ( 'NONE', *, *, #39902, .T. ) ;
#17511 = CARTESIAN_POINT ( 'NONE',  ( 0.2700346912201526672, -1.656539685250784766, 0.7399851559723034100 ) ) ;
#17513 = CARTESIAN_POINT ( 'NONE',  ( 0.1995953702521893469, -1.242370031073753323, 0.5988181646041325079 ) ) ;
#17512 = DIRECTION ( 'NONE',  ( -1.000000000000000000, -7.857794173099924470E-32, -8.628166150854818811E-32 ) ) ;
#17514 = CARTESIAN_POINT ( 'NONE',  ( 0.6348907386704650824, -1.612746832763798155, -0.4546890026736098434 ) ) ;
#17515 = DATE_TIME_ROLE ( 'classification_date' ) ;
#17516 = CARTESIAN_POINT ( 'NONE',  ( 0.03113248654051816583, -0.3767386922704979990, -0.2665524483967541269 ) ) ;
#17518 = ORIENTED_EDGE ( 'NONE', *, *, #2725, .T. ) ;
#17517 = ORIENTED_EDGE ( 'NONE', *, *, #17547, .T. ) ;
#17519 = CARTESIAN_POINT ( 'NONE',  ( 0.01137586991659313325, -0.9325856198352224791, 0.06247312220023811674 ) ) ;
#17520 = CARTESIAN_POINT ( 'NONE',  ( 0.1182319155106198311, -1.406289766173004052, 0.6146117128210031311 ) ) ;
#17521 = ADVANCED_FACE ( 'NONE', ( #19751 ), #22876, .T. ) ;
#17522 = CARTESIAN_POINT ( 'NONE',  ( 0.1708199212777183340, -0.7760174123164113036, 0.5959575580650713356 ) ) ;
#17523 = CARTESIAN_POINT ( 'NONE',  ( 0.06843411546424661707, -1.327640554429453168, 0.5682417262808774350 ) ) ;
#17524 = PLANE ( 'NONE',  #11326 ) ;
#17525 = CARTESIAN_POINT ( 'NONE',  ( 0.1999999903896442222, -2.079563169082558893, -0.2654453414298869052 ) ) ;
#17526 = ADVANCED_FACE ( 'NONE', ( #32701 ), #35391, .F. ) ;
#17527 = DIRECTION ( 'NONE',  ( 0.000000000000000000, 0.9246857012436752177, -0.3807313408632029827 ) ) ;
#17528 = FACE_OUTER_BOUND ( 'NONE', #24056, .T. ) ;
#17529 = AXIS2_PLACEMENT_3D ( 'NONE', #12282, #175, #24839 ) ;
#17530 = ADVANCED_FACE ( 'NONE', ( #32494 ), #19851, .T. ) ;
#17531 = CARTESIAN_POINT ( 'NONE',  ( 0.3568477411066238725, -1.622997595545246918, -0.6071924687824667988 ) ) ;
#17532 = DIRECTION ( 'NONE',  ( 0.8660512985181142431, 0.4999551463232357884, 0.000000000000000000 ) ) ;
#17533 = LINE ( 'NONE', #35844, #5479 ) ;
#17534 = CYLINDRICAL_SURFACE ( 'NONE', #33605, 0.5400000000000004796 ) ;
#17535 = CARTESIAN_POINT ( 'NONE',  ( 0.3850224864643204126, -1.658839704013842065, -0.4046842732936995479 ) ) ;
#17536 = ORGANIZATION ( 'NAUO-ORG13', 'UNSPECIFIED', 'UNSPECIFIED' ) ;
#17537 = SPHERICAL_SURFACE ( 'NONE', #36998, 0.01499999999999999944 ) ;
#17538 = AXIS2_PLACEMENT_3D ( 'NONE', #9468, #30872, #267 ) ;
#17539 = CARTESIAN_POINT ( 'NONE',  ( 0.03132541776874769868, -0.7585458590990268313, 0.6287131927338691639 ) ) ;
#17540 = CARTESIAN_POINT ( 'NONE',  ( 0.4756538103953397711, -1.077424610118791648, 0.6442006390088441670 ) ) ;
#17541 = CALENDAR_DATE ( 2026, 13, 10 ) ;
#17542 = SHAPE_REPRESENTATION ( 'Parallelogram front_REAR', ( #27819 ), #32382 ) ;
#17543 = CARTESIAN_POINT ( 'NONE',  ( 0.1883801994403443147, -0.4771412664261568959, 0.2456734866192890887 ) ) ;
#17544 = EDGE_CURVE ( 'NONE', #2251, #8719, #17090, .T. ) ;
#17545 = EDGE_LOOP ( 'NONE', ( #26877, #38201, #1994, #35809, #35876 ) ) ;
#17546 = EDGE_CURVE ( 'NONE', #34948, #36123, #10910, .T. ) ;
#17547 = EDGE_CURVE ( 'NONE', #31970, #30050, #34723, .T. ) ;
#17548 = CARTESIAN_POINT ( 'NONE',  ( 0.4069111126224479458, -1.648375263996657347, -0.6326914302627749676 ) ) ;
#17549 = LINE ( 'NONE', #9494, #28507 ) ;
#17550 = ORIENTED_EDGE ( 'NONE', *, *, #13270, .T. ) ;
#17551 = CARTESIAN_POINT ( 'NONE',  ( 5.499415574654559131E-16, -0.2899999999999994249, -0.06434668806854157430 ) ) ;
#17552 = CARTESIAN_POINT ( 'NONE',  ( 0.06682382353313973122, -0.8940662392066401898, 0.7548868145630993620 ) ) ;
#17553 = DIRECTION ( 'NONE',  ( 0.000000000000000000, 0.000000000000000000, -1.000000000000000000 ) ) ;
#17555 = ORIENTED_EDGE ( 'NONE', *, *, #8249, .F. ) ;
#17554 = DIRECTION ( 'NONE',  ( 0.000000000000000000, -0.9343694307158671997, 0.3563057211773426602 ) ) ;
#17556 = CIRCLE ( 'NONE', #31997, 0.4614999999999880864 ) ;
#17557 = LINE ( 'NONE', #32570, #14664 ) ;
#17558 = CARTESIAN_POINT ( 'NONE',  ( 0.1912376716460947867, -0.5867422834582064484, 0.1926850933134615362 ) ) ;
#17560 = VERTEX_POINT ( 'NONE', #11902 ) ;
#17559 = ORIENTED_EDGE ( 'NONE', *, *, #26108, .T. ) ;
#17561 = CARTESIAN_POINT ( 'NONE',  ( 0.02678764122032725042, -1.589661793665505307, -0.6397169502282477049 ) ) ;
#17562 = EDGE_LOOP ( 'NONE', ( #30228, #21698, #18122, #5429, #25250 ) ) ;
#17563 = CARTESIAN_POINT ( 'NONE',  ( -0.08000000000000000167, -2.183180860297908144, -0.4937760292030871079 ) ) ;
#17564 = FACE_OUTER_BOUND ( 'NONE', #5129, .T. ) ;
#17565 = ITEM_DEFINED_TRANSFORMATION ( 'NONE', 'NONE', #7497,  #31163 ) ;
#17566 = DIRECTION ( 'NONE',  ( -1.000000000000000000, -2.280301054154495132E-31, 1.664003471950577689E-31 ) ) ;
#17567 = VERTEX_POINT ( 'NONE', #18089 ) ;
#17568 = CARTESIAN_POINT ( 'NONE',  ( 0.09322317613841625550, -1.292681667036668536, 0.5862519905939423959 ) ) ;
#17569 = CARTESIAN_POINT ( 'NONE',  ( 0.08630836114928054636, -0.7249243428820488777, 0.1580372468105708250 ) ) ;
#17570 = B_SPLINE_CURVE_WITH_KNOTS ( 'NONE', 3,
 ( #19958, #29221, #19750, #17068, #4104, #26940, #32492, #23264, #32700, #1458 ),
 .UNSPECIFIED., .F., .F.,
 ( 4, 2, 2, 2, 4 ),
 ( 0.002191118811101763590, 0.002741761465162498475, 0.003292404119223232926, 0.003843046773283967377, 0.004393689427344702261 ),
 .UNSPECIFIED. ) ;
#17571 = CARTESIAN_POINT ( 'NONE',  ( 0.2459797859955291377, -1.413075159975130557, 1.027285411072242027 ) ) ;
#17572 = CARTESIAN_POINT ( 'NONE',  ( 0.1330595972864711818, -0.7019348493605459538, 0.5085182576753194406 ) ) ;
#17574 = CARTESIAN_POINT ( 'NONE',  ( -0.1157923916715208196, -0.5295015842444287246, 0.1380392329925462791 ) ) ;
#17573 = CARTESIAN_POINT ( 'NONE',  ( 0.1148637460941117766, -0.4678991626007031890, 0.04620028533150236788 ) ) ;
#17575 = CARTESIAN_POINT ( 'NONE',  ( 0.3724417182818310357, -1.137927301686664894, 0.6120655133956764971 ) ) ;
#17576 = ORIENTED_EDGE ( 'NONE', *, *, #26983, .F. ) ;
#17577 = EDGE_LOOP ( 'NONE', ( #367, #2120, #24203, #18830, #22321, #33287 ) ) ;
#17578 = EDGE_CURVE ( 'NONE', #30050, #28751, #27718, .T. ) ;
#17579 = CARTESIAN_POINT ( 'NONE',  ( -0.1604632851855414266, 0.4983239941852535271, 0.1050370266831579524 ) ) ;
#17580 = CARTESIAN_POINT ( 'NONE',  ( 0.1960084681062461975, -0.5083467667687623370, 0.3310205429436359204 ) ) ;
#17581 = ADVANCED_FACE ( 'NONE', ( #8821 ), #39765, .T. ) ;
#17582 = DIRECTION ( 'NONE',  ( -2.526820087036053001E-31, -0.1402348365095093807, 0.9901182710308659152 ) ) ;
#17583 = CARTESIAN_POINT ( 'NONE',  ( 0.05283102792148602206, -0.4315398646667508165, 0.1819478359276331114 ) ) ;
#17584 = CARTESIAN_POINT ( 'NONE',  ( -0.02242905165738937404, -0.5043144057283245330, -0.09034433801567860745 ) ) ;
#17585 = DIRECTION ( 'NONE',  ( 0.9591734532964043547, 0.2828184691484104119, 0.000000000000000000 ) ) ;
#17586 = CARTESIAN_POINT ( 'NONE',  ( 0.3948342593773176423, -1.754451107475622162, -0.7138391223717516221 ) ) ;
#17587 = DIRECTION ( 'NONE',  ( 0.000000000000000000, 0.000000000000000000, -1.000000000000000000 ) ) ;
#17588 = CARTESIAN_POINT ( 'NONE',  ( 0.5081268369560435483, -1.127385812641128693, 0.7490048996577514107 ) ) ;
#17589 = B_SPLINE_SURFACE_WITH_KNOTS ( 'NONE', 5, 5, ( 
 ( #5920, #30640, #34118, #2046, #2261, #2653 ),
 ( #8820, #14579, #40286, #21398, #24684, #33494 ),
 ( #37214, #40501, #11901, #17667, #33937, #15404 ),
 ( #24466, #27150, #9034, #21593, #40077, #15194 ),
 ( #18088, #37000, #18482, #11516, #36393, #5112 ),
 ( #14999, #30832, #31038, #2464, #21175, #2856 ) ),
 .UNSPECIFIED., .F., .F., .F.,
 ( 6, 6 ),
 ( 6, 6 ),
 ( -6.477000000001651436, 6.477000000001640778 ),
 ( -2.080605796196440593, 4.396394203803596135 ),
 .UNSPECIFIED. ) ;
#17590 = CARTESIAN_POINT ( 'NONE',  ( 0.3699999999999786793, -2.097675824466503691, -0.5196396315034578217 ) ) ;
#17591 = CARTESIAN_POINT ( 'NONE',  ( 0.1174979645898149572, -1.377733081079238753, -0.3274860884505732539 ) ) ;
#17592 = DIRECTION ( 'NONE',  ( -6.162975822039152677E-33, 0.000000000000000000, -1.000000000000000000 ) ) ;
#17593 = ORIENTED_EDGE ( 'NONE', *, *, #26350, .F. ) ;
#17594 = EDGE_CURVE ( 'NONE', #22691, #38078, #27076, .T. ) ;
#17595 = CARTESIAN_POINT ( 'NONE',  ( 0.4352891435086604921, -1.230633402764584217, 0.5979772237276071989 ) ) ;
#17596 = CARTESIAN_POINT ( 'NONE',  ( -0.05279185365593280777, -0.2420570131477388365, -0.4010466975930389033 ) ) ;
#17597 = VERTEX_POINT ( 'NONE', #15000 ) ;
#17598 = CARTESIAN_POINT ( 'NONE',  ( -0.08000000000000000167, -2.545097362529205487, -0.2282911599260125379 ) ) ;
#17599 = FACE_OUTER_BOUND ( 'NONE', #16714, .T. ) ;
#17600 = CARTESIAN_POINT ( 'NONE',  ( 0.05369492612522367564, -0.8909568881529167372, 0.5212784798856601176 ) ) ;
#17601 = ORIENTED_EDGE ( 'NONE', *, *, #18841, .T. ) ;
#17602 = CARTESIAN_POINT ( 'NONE',  ( 0.05561176441985762192, 0.2871508736821606345, 0.3605511861568527765 ) ) ;
#17603 = CARTESIAN_POINT ( 'NONE',  ( 0.04157143636675603160, 0.01703379379375214581, 0.4699528923077435083 ) ) ;
#17604 = CARTESIAN_POINT ( 'NONE',  ( 0.3695052819757340123, -1.758428263776099287, -0.4278193900811940176 ) ) ;
#17605 = CARTESIAN_POINT ( 'NONE',  ( 0.5129602329048122966, -1.030748725941331267, -0.5155029497116575543 ) ) ;
#17606 = CARTESIAN_POINT ( 'NONE',  ( 0.4658302039846137221, -1.234123384229465437, 0.6126497851603042166 ) ) ;
#17608 = CARTESIAN_POINT ( 'NONE',  ( 0.5205119442373250527, -1.138897204853200229, 0.5683089796893805445 ) ) ;
#17607 = DIRECTION ( 'NONE',  ( 0.8660512985181135770, 0.4999551463232370652, -6.610988856618918076E-16 ) ) ;
#17609 = CYLINDRICAL_SURFACE ( 'NONE', #10588, 0.06000000000000021289 ) ;
#17610 = ORIENTED_EDGE ( 'NONE', *, *, #8921, .T. ) ;
#17611 = CARTESIAN_POINT ( 'NONE',  ( 0.05999999999999990757, -0.3829990175980249600, -0.3390339253215535198 ) ) ;
#17612 = EDGE_LOOP ( 'NONE', ( #34516, #36426, #3032, #5028 ) ) ;
#17613 = CARTESIAN_POINT ( 'NONE',  ( 0.03113248654051816583, -0.03575622569115821658, -0.2978615321325044363 ) ) ;
#17614 = CARTESIAN_POINT ( 'NONE',  ( 0.1000474123420599382, -0.7296998566091608129, 0.5617000639417457641 ) ) ;
#17616 = CARTESIAN_POINT ( 'NONE',  ( 0.000000000000000000, 0.000000000000000000, 0.000000000000000000 ) ) ;
#17615 = CARTESIAN_POINT ( 'NONE',  ( 0.08936724799475873060, -0.5571496410808217670, 0.08395718622765509231 ) ) ;
#17617 = CARTESIAN_POINT ( 'NONE',  ( -0.2300000000000000100, 0.5182417262804744906, 0.3749999999999995559 ) ) ;
#17618 = ORIENTED_EDGE ( 'NONE', *, *, #32662, .F. ) ;
#17619 = ADVANCED_FACE ( 'NONE', ( #40078 ), #30215, .T. ) ;
#17620 = CARTESIAN_POINT ( 'NONE',  ( 0.2615233978049238406, -1.678084768816710648, 0.5373352594323992371 ) ) ;
#17621 = CARTESIAN_POINT ( 'NONE',  ( 0.4497016209966545053, -1.290036543533680913, 0.8253355315714806517 ) ) ;
#17622 = AXIS2_PLACEMENT_3D ( 'NONE', #12445, #21934, #33639 ) ;
#17623 = EDGE_LOOP ( 'NONE', ( #11480, #35226, #29099, #10784 ) ) ;
#17624 = CARTESIAN_POINT ( 'NONE',  ( 0.6522658206810004744, -1.579593865398426722, 0.6111888698553425980 ) ) ;
#17625 = CARTESIAN_POINT ( 'NONE',  ( 0.05269111014005897070, -0.4484844745756915718, 0.1361491033660628125 ) ) ;
#17626 = CARTESIAN_POINT ( 'NONE',  ( 0.6486139156353442070, -1.547557828783085121, 0.4182417262808776903 ) ) ;
#17627 = CARTESIAN_POINT ( 'NONE',  ( 0.1136150038498828785, -1.301558380274246751, 0.4408081706944013689 ) ) ;
#17628 = DIRECTION ( 'NONE',  ( -1.000000000000000000, 0.000000000000000000, 0.000000000000000000 ) ) ;
#17629 = CARTESIAN_POINT ( 'NONE',  ( 0.04582897286455959313, -0.06484386734940368602, 0.4825967645925794414 ) ) ;
#17630 = CARTESIAN_POINT ( 'NONE',  ( 0.3508337187165347926, -0.8535322721259723799, 0.7608596062780633718 ) ) ;
#17631 = DIRECTION ( 'NONE',  ( -1.000000000000000000, -2.280301054154495132E-31, 1.664003471950577689E-31 ) ) ;
#17632 = CARTESIAN_POINT ( 'NONE',  ( -0.1696273608102604469, 0.4941101834779037527, 0.3212105875170810365 ) ) ;
#17633 = CARTESIAN_POINT ( 'NONE',  ( 0.6182805410152977243, -1.621742373187212261, -0.5380257021149844610 ) ) ;
#17634 = LINE ( 'NONE', #33459, #290 ) ;
#17635 = CARTESIAN_POINT ( 'NONE',  ( 0.02999778723028691946, -2.087755359801442445, -0.2623954751430958021 ) ) ;
#17636 = CARTESIAN_POINT ( 'NONE',  ( 0.03664605387828118871, 0.3149102792626792269, -0.3635688186731551585 ) ) ;
#17637 = CARTESIAN_POINT ( 'NONE',  ( 0.1282168942194763239, -1.302307715041175928, 0.4238844456335508215 ) ) ;
#17638 = CARTESIAN_POINT ( 'NONE',  ( 0.03506116283237684095, -0.6633195576212149724, 0.6677130251333698308 ) ) ;
#17639 = CARTESIAN_POINT ( 'NONE',  ( 0.5776621282381364519, -1.563796264554554227, -0.5899727365385690758 ) ) ;
#17640 = CARTESIAN_POINT ( 'NONE',  ( 0.4192378292399245865, -1.648733790552149081, -0.6219568095148814146 ) ) ;
#17641 = EDGE_CURVE ( 'NONE', #17394, #36928, #14580, .T. ) ;
#17642 = FACE_OUTER_BOUND ( 'NONE', #22632, .T. ) ;
#17643 = ORIENTED_EDGE ( 'NONE', *, *, #25566, .F. ) ;
#17644 = DIRECTION ( 'NONE',  ( 6.779273404243062539E-32, -0.5237184928541297468, 0.8518913899333639961 ) ) ;
#17645 = CARTESIAN_POINT ( 'NONE',  ( 0.3734578206545139389, -1.768187696252267571, -0.5721167227818628742 ) ) ;
#17646 = DIRECTION ( 'NONE',  ( 0.000000000000000000, -0.8159412518334726583, -0.5781348229923756188 ) ) ;
#17647 = CARTESIAN_POINT ( 'NONE',  ( 0.6194230288292433828, -1.535705225211028147, -0.4012506026892472821 ) ) ;
#17648 = CARTESIAN_POINT ( 'NONE',  ( 0.5200485381878245938, -1.326553309810435399, 0.6274662840736040526 ) ) ;
#17650 = ORIENTED_EDGE ( 'NONE', *, *, #9368, .T. ) ;
#17649 = CARTESIAN_POINT ( 'NONE',  ( -0.05082303569918694003, 0.4330427793496118838, 0.1918498709088739262 ) ) ;
#17651 = CARTESIAN_POINT ( 'NONE',  ( 0.5138550893713603740, -1.118750960246259307, 0.5715134594416469982 ) ) ;
#17652 = CARTESIAN_POINT ( 'NONE',  ( 0.01044944019094518409, -1.729937559987831275, -0.3655757404049914672 ) ) ;
#17653 = ORIENTED_EDGE ( 'NONE', *, *, #38860, .F. ) ;
#17654 = CARTESIAN_POINT ( 'NONE',  ( 0.3590286451914425081, -1.755833398155118186, -0.5341343048503752744 ) ) ;
#17655 = ORIENTED_EDGE ( 'NONE', *, *, #23252, .F. ) ;
#17656 = CARTESIAN_POINT ( 'NONE',  ( 0.3570248845998820197, -1.622585014455490304, 0.5866312166437432918 ) ) ;
#17657 = CARTESIAN_POINT ( 'NONE',  ( 0.7071432900848956260, -1.497117398935195354, 0.5333719091693975844 ) ) ;
#17658 = CARTESIAN_POINT ( 'NONE',  ( 0.1437340355044557927, -1.283861693981850349, 0.4177417262808780229 ) ) ;
#17659 = VERTEX_POINT ( 'NONE', #27554 ) ;
#17660 = ORIENTED_EDGE ( 'NONE', *, *, #11671, .T. ) ;
#17661 = DIRECTION ( 'NONE',  ( -0.4999551463232373427, 0.8660512985181134660, -0.000000000000000000 ) ) ;
#17662 = CARTESIAN_POINT ( 'NONE',  ( 0.3679555284477226129, -2.044013266926633765, -0.5096248211185702148 ) ) ;
#17663 = CARTESIAN_POINT ( 'NONE',  ( 0.3183040104215587029, -1.268443597496760056, 0.6598424690337639786 ) ) ;
#17664 = DIRECTION ( 'NONE',  ( 0.4999999999999978351, 0.7980870686147867321, 0.3362395439413078391 ) ) ;
#17665 = CARTESIAN_POINT ( 'NONE',  ( 0.5450221724342032559, -1.653079607787938166, -0.5489131283297039587 ) ) ;
#17666 = DIRECTION ( 'NONE',  ( -5.551115123125856658E-17, 5.007578356027541926E-16, 1.000000000000000000 ) ) ;
#17667 = CARTESIAN_POINT ( 'NONE',  ( 0.4793488899164102257, -1.661214906270700453, 0.4177417262808786336 ) ) ;
#17668 = CARTESIAN_POINT ( 'NONE',  ( 0.3613793631777935111, -1.160337313064966347, 0.4225651295761964632 ) ) ;
#17669 = DIRECTION ( 'NONE',  ( 0.000000000000000000, 0.000000000000000000, -1.000000000000000000 ) ) ;
#17670 = CARTESIAN_POINT ( 'NONE',  ( 0.02999999999997886302, -2.183180860297921466, -0.4937760292030871079 ) ) ;
#17671 = APPROVAL_DATE_TIME ( #11906, #13213 ) ;
#17672 = CARTESIAN_POINT ( 'NONE',  ( 0.3579638268247242183, -1.149302532586722103, 0.4372416223683186498 ) ) ;
#17673 = LINE ( 'NONE', #5309, #1486 ) ;
#17674 = DIRECTION ( 'NONE',  ( -1.000000000000000000, -0.000000000000000000, -0.000000000000000000 ) ) ;
#17675 = CARTESIAN_POINT ( 'NONE',  ( 0.4362865664533659982, -1.115424303768361325, -0.3894947692426334873 ) ) ;
#17676 = CARTESIAN_POINT ( 'NONE',  ( -0.2399999999999999079, -3.941790907013290823, 0.1405840032208834911 ) ) ;
#17677 = CARTESIAN_POINT ( 'NONE',  ( -0.01548846960707490547, 0.5346638663566677385, -0.07572681171513587217 ) ) ;
#17678 = CARTESIAN_POINT ( 'NONE',  ( 0.04230188431063434257, -0.008729788072062542176, -0.4686063437799722342 ) ) ;
#17679 = ADVANCED_FACE ( 'NONE', ( #23663, #23870 ), #7999, .T. ) ;
#17680 = ORIENTED_EDGE ( 'NONE', *, *, #25847, .F. ) ;
#17681 = ADVANCED_FACE ( 'NONE', ( #36606 ), #190, .F. ) ;
#17682 = ORIENTED_EDGE ( 'NONE', *, *, #16543, .F. ) ;
#17683 = CARTESIAN_POINT ( 'NONE',  ( 0.1788859795914834461, -0.5039164411451052539, 0.2269575196228969527 ) ) ;
#17684 = ORIENTED_EDGE ( 'NONE', *, *, #15477, .F. ) ;
#17685 = CARTESIAN_POINT ( 'NONE',  ( 0.4114935271033751674, -1.686083435099646977, -0.4173439381843800922 ) ) ;
#17686 = EDGE_CURVE ( 'NONE', #16637, #37027, #37211, .T. ) ;
#17688 = ORIENTED_EDGE ( 'NONE', *, *, #3900, .F. ) ;
#17687 = CARTESIAN_POINT ( 'NONE',  ( -0.2746410161513779258, -2.511040369707300268, -0.4948468226404901804 ) ) ;
#17690 = EDGE_LOOP ( 'NONE', ( #17884, #10626, #36422, #25573 ) ) ;
#17689 = CARTESIAN_POINT ( 'NONE',  ( 0.006255712965108143654, -0.8411565454896892113, 0.1072706165909301929 ) ) ;
#17691 = EDGE_CURVE ( 'NONE', #13011, #38249, #25765, .T. ) ;
#17692 = ORIENTED_EDGE ( 'NONE', *, *, #19987, .T. ) ;
#17693 = CARTESIAN_POINT ( 'NONE',  ( 0.1499999999999990508, -0.4730347584886803736, -0.2341461249029834490 ) ) ;
#17694 = VERTEX_POINT ( 'NONE', #24883 ) ;
#17695 = CARTESIAN_POINT ( 'NONE',  ( 0.2666826698441861487, -1.675428791908667892, 0.5775416952914532720 ) ) ;
#17697 = CARTESIAN_POINT ( 'NONE',  ( 0.1475177807054492418, -1.270527447976652180, 0.6057499628053283347 ) ) ;
#17696 = CARTESIAN_POINT ( 'NONE',  ( 0.4584717390208090659, -1.703043547193806573, -0.5155029497116575543 ) ) ;
#17698 = DIRECTION ( 'NONE',  ( 0.4999551463232372317, -0.8660512985181135770, 0.000000000000000000 ) ) ;
#17699 = PERSON_AND_ORGANIZATION ( #3421, #7008 ) ;
#17700 = CARTESIAN_POINT ( 'NONE',  ( -0.1667650433730277770, 0.4848728453260193749, 0.3315300532330285321 ) ) ;
#17702 = VERTEX_POINT ( 'NONE', #6341 ) ;
#17701 = ORIENTED_EDGE ( 'NONE', *, *, #18023, .F. ) ;
#17703 = CARTESIAN_POINT ( 'NONE',  ( 0.3866205031219385191, -1.115072307344278535, 0.6234536249022221144 ) ) ;
#17704 = B_SPLINE_CURVE_WITH_KNOTS ( 'NONE', 3,
 ( #3447, #16604, #22198, #615, #425, #19093 ),
 .UNSPECIFIED., .F., .F.,
 ( 4, 2, 4 ),
 ( 0.0002303018524726760570, 0.0008163183685728757919, 0.001402334884673075554 ),
 .UNSPECIFIED. ) ;
#17705 = CARTESIAN_POINT ( 'NONE',  ( 0.2101951102887192890, -1.233953443661628846, 0.5631135429232324574 ) ) ;
#17706 = CARTESIAN_POINT ( 'NONE',  ( 0.1724982287072397702, -0.8035217669752177105, 0.5910157953457164659 ) ) ;
#17707 = CARTESIAN_POINT ( 'NONE',  ( 0.1852881512505511474, -0.8378655682486129130, 0.1409330132775444278 ) ) ;
#17708 = EDGE_CURVE ( 'NONE', #19134, #34885, #6533, .T. ) ;
#17709 = DIRECTION ( 'NONE',  ( 0.9848077530122080203, -0.1736481776669303589, -3.189865274363657256E-17 ) ) ;
#17710 = DIRECTION ( 'NONE',  ( 0.000000000000000000, 3.885780586188049371E-16, 1.000000000000000000 ) ) ;
#17711 = PRODUCT_DEFINITION ( 'UNKNOWN', '', #1014, #13779 ) ;
#17712 = CARTESIAN_POINT ( 'NONE',  ( -1.019575837292303166, -0.04310840302197994911, 0.08499999999999990896 ) ) ;
#17713 = FACE_OUTER_BOUND ( 'NONE', #26125, .T. ) ;
#17714 = CARTESIAN_POINT ( 'NONE',  ( 0.3360297777558891585, -1.646801663888270317, -0.6479318779998786137 ) ) ;
#17715 = CARTESIAN_POINT ( 'NONE',  ( 0.1998231473750205767, -2.070638627232769480, -0.2997811547186691739 ) ) ;
#17716 = CARTESIAN_POINT ( 'NONE',  ( -1.133455804397020025E-05, -0.9470593448225452793, 0.1159768874212486062 ) ) ;
#17717 = FACE_OUTER_BOUND ( 'NONE', #35362, .T. ) ;
#17718 = CARTESIAN_POINT ( 'NONE',  ( 0.000000000000000000, 0.000000000000000000, 0.000000000000000000 ) ) ;
#17719 = CARTESIAN_POINT ( 'NONE',  ( 0.6129340932688779331, -1.613573864442072292, -0.5426322817999900128 ) ) ;
#17720 = EDGE_CURVE ( 'NONE', #5090, #40153, #31316, .T. ) ;
#17721 = CARTESIAN_POINT ( 'NONE',  ( 0.2322327485446251394, -1.539891620887370749, 0.8667544471685157959 ) ) ;
#17722 = CARTESIAN_POINT ( 'NONE',  ( 0.2530466182501821537, -0.9510907114987208200, 0.4863111693326979679 ) ) ;
#17723 = CARTESIAN_POINT ( 'NONE',  ( 0.02653710545434064677, -0.9701798883197163548, 0.6461398643848382806 ) ) ;
#17724 = DATE_TIME_ROLE ( 'classification_date' ) ;
#17725 = CARTESIAN_POINT ( 'NONE',  ( 0.1875104876115774588, -0.4605130342159906021, 0.1706505080850997946 ) ) ;
#17726 = CARTESIAN_POINT ( 'NONE',  ( 0.3745565332565439221, -1.612774642522065704, -0.6154719560940745682 ) ) ;
#17727 = CARTESIAN_POINT ( 'NONE',  ( 0.02953079040094795660, 0.09152108205202806601, -0.5223162075576639474 ) ) ;
#17728 = EDGE_CURVE ( 'NONE', #15674, #13990, #9831, .T. ) ;
#17729 = CARTESIAN_POINT ( 'NONE',  ( 0.02999999999976839596, -2.097673604718639062, -0.7286983764821324261 ) ) ;
#17730 = ORIENTED_EDGE ( 'NONE', *, *, #33508, .F. ) ;
#17731 = DIRECTION ( 'NONE',  ( 0.8150167559926634331, 0.5794373887239202547, 1.138269997360109576E-15 ) ) ;
#17732 = CARTESIAN_POINT ( 'NONE',  ( 0.02323507894693532111, -0.7204624892072191145, 0.5750910600171844633 ) ) ;
#17733 = ADVANCED_FACE ( 'NONE', ( #3464 ), #441, .T. ) ;
#17734 = CARTESIAN_POINT ( 'NONE',  ( 0.5879123204753100573, -1.491226093260655583, 0.5729944458046030142 ) ) ;
#17735 = CARTESIAN_POINT ( 'NONE',  ( 0.3717145517045183922, -1.760210800595612080, -0.4321619518649676972 ) ) ;
#17737 = EDGE_LOOP ( 'NONE', ( #23608, #16746 ) ) ;
#17736 = CARTESIAN_POINT ( 'NONE',  ( 0.3868278802867940458, -1.884152038337740143, -0.4995641518168190687 ) ) ;
#17738 = CARTESIAN_POINT ( 'NONE',  ( 0.02231181081520650783, 0.3551561381230151637, 0.3696296485972545010 ) ) ;
#17739 = ADVANCED_FACE ( 'NONE', ( #12325 ), #3425, .T. ) ;
#17740 = CARTESIAN_POINT ( 'NONE',  ( 0.2790103250938448243, -0.7681568326658522183, 0.6036499921438334137 ) ) ;
#17742 = ORIENTED_EDGE ( 'NONE', *, *, #5018, .T. ) ;
#17741 = VERTEX_POINT ( 'NONE', #27752 ) ;
#17743 = CARTESIAN_POINT ( 'NONE',  ( 0.003249118729953440199, -1.844392804249546103, -0.6741495493879861023 ) ) ;
#17744 = ORIENTED_EDGE ( 'NONE', *, *, #22058, .F. ) ;
#17745 = DIRECTION ( 'NONE',  ( -0.9378410757839561462, -0.1072489841977624786, 0.3300784330442383396 ) ) ;
#17746 = CARTESIAN_POINT ( 'NONE',  ( 0.4549080897931743750, -1.227294277471189465, 0.6004711738143356792 ) ) ;
#17747 = APPROVAL_DATE_TIME ( #8490, #40039 ) ;
#17748 = TOROIDAL_SURFACE ( 'NONE', #31546, 0.5250000000000000222, 0.01499999999999999944 ) ;
#17749 = CARTESIAN_POINT ( 'NONE',  ( -0.2399999999999999079, -2.375007723916885194, -0.5268601001523036675 ) ) ;
#17750 = ORIENTED_EDGE ( 'NONE', *, *, #16449, .F. ) ;
#17751 = CARTESIAN_POINT ( 'NONE',  ( 0.1734973056165641514, -1.209394307038482497, -0.5155029497116575543 ) ) ;
#17752 = CIRCLE ( 'NONE', #8070, 0.1000000000000000194 ) ;
#17753 = CARTESIAN_POINT ( 'NONE',  ( 0.1550089719294916735, -0.8025920081343739243, 0.5453556522365147208 ) ) ;
#17754 = CARTESIAN_POINT ( 'NONE',  ( 0.2518910028716056515, -1.434241493328622941, 1.024070326526868469 ) ) ;
#17755 = VECTOR ( 'NONE', #29071, 39.37007874015748143 ) ;
#17756 = CARTESIAN_POINT ( 'NONE',  ( 0.2083161643468393331, -0.8974363671813946342, 0.7129651506473948519 ) ) ;
#17758 = DIRECTION ( 'NONE',  ( 0.9378410757839513723, -0.2807814858886641396, 0.2039996905746546685 ) ) ;
#17757 = DIRECTION ( 'NONE',  ( -0.8062136690494358104, -0.4849338684320062542, 0.3389080451765882351 ) ) ;
#17759 = EDGE_CURVE ( 'NONE', #2621, #22034, #24685, .T. ) ;
#17760 = CARTESIAN_POINT ( 'NONE',  ( 0.01684860433265163854, -0.9502109314606926871, 0.2753421542032672975 ) ) ;
#17761 = ORIENTED_EDGE ( 'NONE', *, *, #32098, .T. ) ;
#17762 = ORIENTED_EDGE ( 'NONE', *, *, #38938, .T. ) ;
#17763 = CARTESIAN_POINT ( 'NONE',  ( 0.03309057659885086822, -0.4608882367397868496, -0.2425133248663977337 ) ) ;
#17764 = CARTESIAN_POINT ( 'NONE',  ( 0.4470003202926319807, -1.034455986214164902, 0.7862651520392351934 ) ) ;
#17765 = LINE ( 'NONE', #27252, #32518 ) ;
#17766 = DIRECTION ( 'NONE',  ( 0.000000000000000000, 0.6595282642760673664, 0.7516797646744242112 ) ) ;
#17767 = DIRECTION ( 'NONE',  ( 0.08797602414327373999, 0.6303231869445276025, 0.7713318994933610062 ) ) ;
#17768 = CARTESIAN_POINT ( 'NONE',  ( 0.2285553773980233683, -1.596574492821664526, -0.6995327739724715999 ) ) ;
#17769 = CARTESIAN_POINT ( 'NONE',  ( 0.3206377073886440554, -1.170977842177069350, 0.5588165336952308770 ) ) ;
#17770 = CARTESIAN_POINT ( 'NONE',  ( 0.5761226916817485666, -1.227707429964641328, 0.7155794456320599961 ) ) ;
#17771 = APPROVAL_DATE_TIME ( #25903, #22763 ) ;
#17772 = CARTESIAN_POINT ( 'NONE',  ( 0.05999999999999990757, 0.7171888913565960255, -0.2950238883388468514 ) ) ;
#17773 = CIRCLE ( 'NONE', #28938, 0.01500000000000002894 ) ;
#17774 = PLANE ( 'NONE',  #5463 ) ;
#17775 = CARTESIAN_POINT ( 'NONE',  ( 0.4136942338497008320, -1.674605337725208143, -0.3991494578240276647 ) ) ;
#17776 = DIRECTION ( 'NONE',  ( -1.000000000000000000, -2.280301054154495132E-31, 1.664003471950577689E-31 ) ) ;
#17777 = DIRECTION ( 'NONE',  ( -0.000000000000000000, 0.3090169943749569437, 0.9510565162951504226 ) ) ;
#17778 = CARTESIAN_POINT ( 'NONE',  ( -0.03301200226531783577, -0.3732424419978427887, -0.3635087277994391575 ) ) ;
#17779 = AXIS2_PLACEMENT_3D ( 'NONE', #8789, #2625, #6310 ) ;
#17780 = VERTEX_POINT ( 'NONE', #15405 ) ;
#17781 = CARTESIAN_POINT ( 'NONE',  ( -0.02953079040095652960, 0.5250338024619264354, 0.07436286310882474215 ) ) ;
#17782 = AXIS2_PLACEMENT_3D ( 'NONE', #103, #15896, #13021 ) ;
#17783 = EDGE_CURVE ( 'NONE', #1249, #9409, #21837, .T. ) ;
#17784 = DIRECTION ( 'NONE',  ( 0.000000000000000000, 0.000000000000000000, -1.000000000000000000 ) ) ;
#17785 = CARTESIAN_POINT ( 'NONE',  ( 0.2203738904872941939, -1.339329718032100880, 0.6315676663001210667 ) ) ;
#17786 = VERTEX_POINT ( 'NONE', #9217 ) ;
#17787 = CARTESIAN_POINT ( 'NONE',  ( -0.04229956186878665314, 0.2825373843407192331, 0.3739591931584692608 ) ) ;
#17788 = DIRECTION ( 'NONE',  ( -0.8660512985181130219, -0.4999551463232380644, 0.000000000000000000 ) ) ;
#17789 = CARTESIAN_POINT ( 'NONE',  ( 0.04946288932099927871, -0.4635771722446667686, -0.1136559182874704588 ) ) ;
#17790 = ADVANCED_FACE ( 'NONE', ( #21788, #20273 ), #32793, .F. ) ;
#17791 = DIRECTION ( 'NONE',  ( -1.000000000000000000, -1.448788479720436272E-15, 8.229804381843897223E-16 ) ) ;
#17792 = CARTESIAN_POINT ( 'NONE',  ( 0.4069238378739554185, -1.154943970571837175, 0.6833052645732561325 ) ) ;
#17794 = CYLINDRICAL_SURFACE ( 'NONE', #34555, 0.07999999999999996003 ) ;
#17793 = CARTESIAN_POINT ( 'NONE',  ( 0.1399999999999994582, 0.000000000000000000, 0.000000000000000000 ) ) ;
#17795 = CARTESIAN_POINT ( 'NONE',  ( -1.502516396515344672E-15, -0.3899999999999999578, 5.463695987328526437E-16 ) ) ;
#17796 = VERTEX_POINT ( 'NONE', #27045 ) ;
#17797 = ORIENTED_EDGE ( 'NONE', *, *, #19114, .T. ) ;
#17798 = CARTESIAN_POINT ( 'NONE',  ( 0.06653396568654543208, -1.328888091817681749, 0.5069507058184855586 ) ) ;
#17799 = ORIENTED_EDGE ( 'NONE', *, *, #29129, .F. ) ;
#17800 = DIRECTION ( 'NONE',  ( 0.000000000000000000, 0.000000000000000000, -1.000000000000000000 ) ) ;
#17801 = CARTESIAN_POINT ( 'NONE',  ( 0.4426374324197126509, -1.573834870353632898, 0.5890683219565086004 ) ) ;
#17803 = CARTESIAN_POINT ( 'NONE',  ( 0.4581930876178143541, -1.105887789949125510, -0.6551259416095572830 ) ) ;
#17802 = CARTESIAN_POINT ( 'NONE',  ( 0.08771197480159868831, -0.6713012847033815733, 0.02348685380516160603 ) ) ;
#17804 = CARTESIAN_POINT ( 'NONE',  ( -0.01548846960721238578, 0.2450655194478933985, -0.4674710490746305513 ) ) ;
#17805 = EDGE_CURVE ( 'NONE', #12532, #34047, #19207, .T. ) ;
#17806 = ORIENTED_EDGE ( 'NONE', *, *, #13417, .T. ) ;
#17807 = CIRCLE ( 'NONE', #117, 0.1000000000000000194 ) ;
#17808 = EDGE_CURVE ( 'NONE', #7716, #34573, #31001, .T. ) ;
#17809 = CARTESIAN_POINT ( 'NONE',  ( 0.1837600765269550573, -1.884334881598526579, -0.3110488970864131453 ) ) ;
#17810 = AXIS2_PLACEMENT_3D ( 'NONE', #39671, #21588, #40495 ) ;
#17811 = CARTESIAN_POINT ( 'NONE',  ( 0.5779626767790062569, -1.486117140961969563, 0.6660763835963422475 ) ) ;
#17812 = CARTESIAN_POINT ( 'NONE',  ( -0.08000000000000000167, -1.538828486247671101, 0.2167077994389899898 ) ) ;
#17813 = AXIS2_PLACEMENT_3D ( 'NONE', #10828, #4616, #17397 ) ;
#17814 = CARTESIAN_POINT ( 'NONE',  ( 2.172611109905790102E-15, -0.2899999999999994249, 0.06434668806854020040 ) ) ;
#17815 = AXIS2_PLACEMENT_3D ( 'NONE', #34996, #28832, #7016 ) ;
#17816 = CARTESIAN_POINT ( 'NONE',  ( 0.1743562189534910989, -1.266421578639647327, 0.4246093132792315150 ) ) ;
#17817 = AXIS2_PLACEMENT_3D ( 'NONE', #24752, #37274, #9091 ) ;
#17818 = LINE ( 'NONE', #13912, #11495 ) ;
#17819 = CARTESIAN_POINT ( 'NONE',  ( -0.2746410161513779258, -3.941790907013290823, -0.4709369376873030477 ) ) ;
#17820 = CARTESIAN_POINT ( 'NONE',  ( 0.7220926616001757115, -1.479655736425856682, 0.5682417262808782121 ) ) ;
#17821 = CARTESIAN_POINT ( 'NONE',  ( 0.07497864282572903882, -1.322056043867073427, 0.4862695133534064018 ) ) ;
#17822 = CARTESIAN_POINT ( 'NONE',  ( 0.01423347799720674905, -0.9652063955883527502, 0.3874744253929337523 ) ) ;
#17823 = B_SPLINE_CURVE_WITH_KNOTS ( 'NONE', 3,
 ( #23147, #29705, #26425, #29505, #23748, #17156, #14275, #17574 ),
 .UNSPECIFIED., .F., .F.,
 ( 4, 2, 2, 4 ),
 ( 0.0005881714484888313221, 0.001255587419990858997, 0.001589295405741874461, 0.001923003391492890141 ),
 .UNSPECIFIED. ) ;
#17824 = B_SPLINE_CURVE_WITH_KNOTS ( 'NONE', 3,
 ( #40619, #21101, #33854, #2781, #6050, #18618, #15330, #5239 ),
 .UNSPECIFIED., .F., .F.,
 ( 4, 2, 2, 4 ),
 ( 2.350980519355055435E-07, 0.001838925622864751681, 0.002758270885271160797, 0.003677616147677569697 ),
 .UNSPECIFIED. ) ;
#17825 = CARTESIAN_POINT ( 'NONE',  ( 0.5857764079363468879, -1.600142216809019802, -0.5816357325289774893 ) ) ;
#17826 = CARTESIAN_POINT ( 'NONE',  ( 0.02977875364827006072, -2.019445173720740616, -0.7044873537940673502 ) ) ;
#17827 = CARTESIAN_POINT ( 'NONE',  ( 0.5881428029937501023, -1.617990245335324984, 0.5794342689744652608 ) ) ;
#17828 = CARTESIAN_POINT ( 'NONE',  ( 0.6973771390368941336, -1.438889517336061408, 0.5421659396764333394 ) ) ;
#17829 = CARTESIAN_POINT ( 'NONE',  ( 0.000000000000000000, 0.000000000000000000, 0.000000000000000000 ) ) ;
#17830 = CARTESIAN_POINT ( 'NONE',  ( 0.1835961851041346959, -0.5126270562563732813, 0.08826789480522242992 ) ) ;
#17831 = CARTESIAN_POINT ( 'NONE',  ( 0.4102222551943826567, -1.708906198810314248, -0.6086602454107996607 ) ) ;
#17832 = CARTESIAN_POINT ( 'NONE',  ( 0.1664437047740607023, -1.270578109106206277, 0.5509909136888835324 ) ) ;
#17833 = VECTOR ( 'NONE', #8256, 39.37007874015748854 ) ;
#17834 = ADVANCED_FACE ( 'NONE', ( #32389 ), #38443, .T. ) ;
#17835 = DIRECTION ( 'NONE',  ( 0.8660254037844409281, -0.3758398823372091635, 0.3297641321380309631 ) ) ;
#17836 = ORIENTED_EDGE ( 'NONE', *, *, #35512, .F. ) ;
#17837 = CARTESIAN_POINT ( 'NONE',  ( 0.4789169902643273247, -1.099522405089615962, -0.6159558956687188891 ) ) ;
#17838 = AXIS2_PLACEMENT_3D ( 'NONE', #17901, #39926, #11743 ) ;
#17839 = AXIS2_PLACEMENT_3D ( 'NONE', #22142, #5501, #24247 ) ;
#17840 = CARTESIAN_POINT ( 'NONE',  ( 0.3870156086493387604, -1.114928226039928028, 0.6233982234651463950 ) ) ;
#17841 = FACE_OUTER_BOUND ( 'NONE', #26024, .T. ) ;
#17842 = CARTESIAN_POINT ( 'NONE',  ( -0.03309057659885162456, 0.2303206601891044092, -0.4671007096900172684 ) ) ;
#17843 = AXIS2_PLACEMENT_3D ( 'NONE', #15063, #12186, #34177 ) ;
#17844 = CARTESIAN_POINT ( 'NONE',  ( 0.5323400999026242086, -1.348064161999662280, 0.6174472662931688172 ) ) ;
#17846 = ORIENTED_EDGE ( 'NONE', *, *, #21883, .F. ) ;
#17845 = FACE_OUTER_BOUND ( 'NONE', #31246, .T. ) ;
#17847 = CARTESIAN_POINT ( 'NONE',  ( 0.4955945803445692133, -1.095919195860131534, 0.6270439991606266972 ) ) ;
#17848 = ORIENTED_EDGE ( 'NONE', *, *, #15020, .F. ) ;
#17849 = LINE ( 'NONE', #24863, #39476 ) ;
#17850 = ORIENTED_EDGE ( 'NONE', *, *, #37441, .T. ) ;
#17851 = CARTESIAN_POINT ( 'NONE',  ( 0.3690965330173307524, -1.099411688709415413, 0.5182417262812423209 ) ) ;
#17852 = CARTESIAN_POINT ( 'NONE',  ( 0.1349261257125279889, -0.9884281589464994910, 0.8058857660061659045 ) ) ;
#17854 = CARTESIAN_POINT ( 'NONE',  ( -0.02869942827333544708, -0.3396431753871640424, 0.3648167270360663794 ) ) ;
#17853 = CARTESIAN_POINT ( 'NONE',  ( 0.7014158978116333820, -1.493052833726295381, 0.5008243877641355146 ) ) ;
#17855 = CARTESIAN_POINT ( 'NONE',  ( 0.1637488714925408873, -0.5994898440788770655, 0.1932149833450298726 ) ) ;
#17856 = ORIENTED_EDGE ( 'NONE', *, *, #30348, .F. ) ;
#17857 = ORIENTED_EDGE ( 'NONE', *, *, #297, .T. ) ;
#17858 = CARTESIAN_POINT ( 'NONE',  ( 0.3743249978302641279, -1.006520688755567106, 0.6168196747304992567 ) ) ;
#17859 = EDGE_LOOP ( 'NONE', ( #37581, #16486, #31418, #38949 ) ) ;
#17860 = CARTESIAN_POINT ( 'NONE',  ( 0.4265829747943327699, -1.610301022689196060, -0.3658488903366757805 ) ) ;
#17861 = DIRECTION ( 'NONE',  ( -0.4999999999999976685, 0.7693667687702180347, -0.3975861857661508458 ) ) ;
#17862 = CARTESIAN_POINT ( 'NONE',  ( 0.08497705572000407992, -0.8399793145007137252, 0.3168515346811236477 ) ) ;
#17863 = CARTESIAN_POINT ( 'NONE',  ( 0.1758314180332314625, -1.266529637424046006, -0.3265915900978382247 ) ) ;
#17864 = ADVANCED_FACE ( 'NONE', ( #17167 ), #29327, .F. ) ;
#17865 = CARTESIAN_POINT ( 'NONE',  ( 0.000000000000000000, -0.6872203660140440151, 0.1457185332388702681 ) ) ;
#17866 = CARTESIAN_POINT ( 'NONE',  ( -0.1684323895664698867, 0.5231977504175417959, 0.3032895567580831675 ) ) ;
#17867 = AXIS2_PLACEMENT_3D ( 'NONE', #36442, #30074, #18329 ) ;
#17868 = CIRCLE ( 'NONE', #30363, 0.01500000000000002200 ) ;
#17869 = CARTESIAN_POINT ( 'NONE',  ( 0.03650581953630534227, 0.2290855126858382385, -0.4575806651622376653 ) ) ;
#17870 = CARTESIAN_POINT ( 'NONE',  ( -0.08000000000000000167, -2.183180860297908144, -0.4312760292030870524 ) ) ;
#17871 = FACE_OUTER_BOUND ( 'NONE', #30948, .T. ) ;
#17872 = SHAPE_DEFINITION_REPRESENTATION ( #33343, #27514 ) ;
#17873 = VECTOR ( 'NONE', #16539, 39.37007874015748143 ) ;
#17874 = CARTESIAN_POINT ( 'NONE',  ( 0.4471907055705798273, -1.138637937364841646, 0.4406841123770021684 ) ) ;
#17875 = CARTESIAN_POINT ( 'NONE',  ( 0.4033617574584467680, -1.135069255774922015, 0.5545239497365388459 ) ) ;
#17876 = CARTESIAN_POINT ( 'NONE',  ( 0.06980746140711582837, -4.527947890665460015E-17, -0.2150000000000000244 ) ) ;
#17877 = CARTESIAN_POINT ( 'NONE',  ( 4.197799705714884069E-05, -0.4263059253886176680, 0.1506519890000039552 ) ) ;
#17878 = LINE ( 'NONE', #30445, #24570 ) ;
#17879 = DIRECTION ( 'NONE',  ( 0.000000000000000000, 0.000000000000000000, -1.000000000000000000 ) ) ;
#17880 = DIRECTION ( 'NONE',  ( -0.2067069058495574485, -0.1193280138680813535, -0.9710989033977958096 ) ) ;
#17881 = ORIENTED_EDGE ( 'NONE', *, *, #23575, .T. ) ;
#17882 = ORIENTED_EDGE ( 'NONE', *, *, #2147, .F. ) ;
#17883 = CARTESIAN_POINT ( 'NONE',  ( 0.3324871086615504012, -1.659137217475707304, -0.6399689536651966826 ) ) ;
#17884 = ORIENTED_EDGE ( 'NONE', *, *, #39553, .T. ) ;
#17885 = LINE ( 'NONE', #39491, #12508 ) ;
#17886 = AXIS2_PLACEMENT_3D ( 'NONE', #9581, #38715, #28292 ) ;
#17887 = DIRECTION ( 'NONE',  ( 1.000000000000000000, 2.341930812374887555E-31, -1.664003471950578127E-31 ) ) ;
#17889 = ORIENTED_EDGE ( 'NONE', *, *, #3735, .T. ) ;
#17888 = CARTESIAN_POINT ( 'NONE',  ( -0.0007351284806403281420, -0.7588986013227282390, 0.002782588056763008258 ) ) ;
#17890 = ORIENTED_EDGE ( 'NONE', *, *, #12267, .T. ) ;
#17891 = CARTESIAN_POINT ( 'NONE',  ( 0.01548846960721238578, 0.5203207976464816475, -0.08861466064783077301 ) ) ;
#17892 = CIRCLE ( 'NONE', #31707, 0.08830708661417341343 ) ;
#17893 = EDGE_LOOP ( 'NONE', ( #8075, #7771, #28734 ) ) ;
#17894 = AXIS2_PLACEMENT_3D ( 'NONE', #16083, #12569, #18761 ) ;
#17895 = CARTESIAN_POINT ( 'NONE',  ( 0.2052211579314608680, -1.341797434425455515, 0.9341812257356882920 ) ) ;
#17897 = CARTESIAN_POINT ( 'NONE',  ( 0.5462348416196848300, -1.594646255991501560, -0.4868944820179722521 ) ) ;
#17896 = DIRECTION ( 'NONE',  ( 0.000000000000000000, 0.000000000000000000, -1.000000000000000000 ) ) ;
#17898 = CARTESIAN_POINT ( 'NONE',  ( -0.05464101615137769569, -1.758704040287260018, -0.8825853814972600686 ) ) ;
#17899 = SECURITY_CLASSIFICATION_LEVEL ( 'unclassified' ) ;
#17900 = TOROIDAL_SURFACE ( 'NONE', #14614, 0.5250000000000000222, 0.01499999999999999944 ) ;
#17901 = CARTESIAN_POINT ( 'NONE',  ( 0.01548846960707524721, 0.000000000000000000, 0.000000000000000000 ) ) ;
#17903 = ORIENTED_EDGE ( 'NONE', *, *, #21244, .T. ) ;
#17902 = VERTEX_POINT ( 'NONE', #7704 ) ;
#17904 = B_SPLINE_CURVE_WITH_KNOTS ( 'NONE', 3,
 ( #40620, #34044, #31380, #8532, #21102, #18003 ),
 .UNSPECIFIED., .F., .F.,
 ( 4, 2, 4 ),
 ( 0.000000000000000000, 0.5000000000000000000, 1.000000000000000000 ),
 .UNSPECIFIED. ) ;
#17905 = CARTESIAN_POINT ( 'NONE',  ( 0.08509544147734073027, -0.8123111742434827587, 0.1597949892228995861 ) ) ;
#17906 = CARTESIAN_POINT ( 'NONE',  ( 0.1146236400730676064, -1.385147693593549389, 0.6565552975533486268 ) ) ;
#17907 = B_SPLINE_SURFACE_WITH_KNOTS ( 'NONE', 3, 3, ( 
 ( #35028, #9537, #28863, #37924, #3957, #3348, #12832, #723, #22717, #25173, #28452, #22114, #19421, #31955, #22304, #113, #7047, #25395, #34819, #13222, #12414, #24964, #3772, #16327, #34635, #25791, #6240, #3159, #539, #10144, #35249 ),
 ( #6628, #16519, #37495, #38316, #13034, #6432, #28249, #19204, #18813, #19004, #31746, #31536, #15703, #3564, #16133, #28670, #19616, #32151, #9317, #25586, #38113, #21898, #23328, #4555, #36048, #928, #8054, #13436, #19804, #20419, #7447 ),
 ( #38527, #20231, #7664, #35641, #1130, #17330, #10543, #22920, #35435, #32342, #7235, #26005, #20632, #4163, #35851, #10972, #26609, #13632, #38925, #16730, #13824, #29473, #32751, #26198, #29281, #20021, #38722, #32953, #32554, #23118, #7847 ),
 ( #1317, #17124, #33168, #4374, #4757, #29674, #16929, #4973, #29888, #26394, #29059, #10357, #1516, #10755, #23529, #14034, #39145, #1728, #14244, #26807, #39334, #11156, #23713, #36240, #39524, #8661, #5169, #34170, #12173, #30086, #8464 ),
 ( #14636, #30487, #37057, #30269, #30696, #21234, #21455, #17721, #2099, #9080, #11356, #36848, #27206, #33361, #2316, #23925, #30887, #17539, #40344, #2517, #15056, #2708, #36658, #26996, #36456, #37264, #17926, #21646, #27606, #8268, #24136 ),
 ( #14857, #11963, #24737, #14427, #39740, #33980, #27420, #5785, #20841, #11574, #21028, #40135, #33552, #1914, #5361, #33772, #18342, #39943, #11763, #24320, #24528, #5582, #18141, #8879, #15252, #27810, #22263, #28019, #15865, #21849, #9696 ),
 ( #6394, #37881, #10097, #22065, #9884, #34776, #12372, #22671, #6792, #34590, #38266, #31095, #6581, #28413, #496, #75, #18960, #40552, #25541, #25739, #31309, #19163, #2915, #25128, #24928, #31701, #34376, #37456, #28821, #5978, #28625 ) ),
 .UNSPECIFIED., .F., .F., .F.,
 ( 4, 1, 1, 1, 4 ),
 ( 4, 1, 1, 1, 1, 1, 1, 1, 1, 1, 1, 1, 1, 1, 1, 1, 1, 1, 1, 1, 1, 1, 1, 1, 1, 3, 4 ),
 ( 0.000000000000000000, 0.2500000000000000000, 0.5000000000000000000, 0.7500000000000000000, 1.000000000000000000 ),
 ( 0.000000000000000000, 0.03051875000000000074, 0.04577812500000000978, 0.06103750000000000148, 0.09155625000000001956, 0.1220750000000000030, 0.1525937500000000002, 0.1831125000000000391, 0.2136312499999999948, 0.2441500000000000059, 0.2993062499999999959, 0.3544624999999999027, 0.4096187500000000314, 0.4647750000000000492, 0.5199312500000002890, 0.5750875000000000847, 0.6302437499999999915, 0.6854000000000000092, 0.7247249999999998415, 0.7640500000000001180, 0.8033749999999999503, 0.8427000000000000046, 0.8820249999999999480, 0.9213500000000000023, 0.9606749999999998346, 1.000000000000000000, 1.037727370758942724 ),
 .UNSPECIFIED. ) ;
#17908 = CARTESIAN_POINT ( 'NONE',  ( 0.2242084987759379311, -0.9108783394681766454, 0.7161520956205715827 ) ) ;
#17909 = CARTESIAN_POINT ( 'NONE',  ( 0.1874345095996926280, -0.6910927985529788931, 0.04286511273904547448 ) ) ;
#17910 = VECTOR ( 'NONE', #16178, 39.37007874015748854 ) ;
#17911 = DIRECTION ( 'NONE',  ( 0.000000000000000000, 0.8159412518334721032, 0.5781348229923763959 ) ) ;
#17912 = DIRECTION ( 'NONE',  ( 0.1611076279721909144, -0.2660824569950847041, 0.9503917393836255334 ) ) ;
#17913 = CARTESIAN_POINT ( 'NONE',  ( 0.01221471773871474209, -0.4297850025901314708, 0.1735288129617342245 ) ) ;
#17914 = CARTESIAN_POINT ( 'NONE',  ( 0.4131462650696018368, -1.740755752022009606, -0.5824989720263729076 ) ) ;
#17915 = EDGE_CURVE ( 'NONE', #7075, #34890, #36903, .T. ) ;
#17916 = DIRECTION ( 'NONE',  ( 0.8660512985181135770, 0.4999551463232371762, 0.000000000000000000 ) ) ;
#17917 = DIRECTION ( 'NONE',  ( 0.4999551463232373427, -0.8660512985181134660, 0.000000000000000000 ) ) ;
#17918 = CARTESIAN_POINT ( 'NONE',  ( 0.3060205578877235877, -1.769002121529782423, 0.4687417262808789009 ) ) ;
#17919 = CARTESIAN_POINT ( 'NONE',  ( 0.4548090296651450259, -1.115736959625045932, 0.5760494755837164416 ) ) ;
#17920 = CARTESIAN_POINT ( 'NONE',  ( 0.3929308436716468234, -1.654878899976784501, -0.4107462969407084108 ) ) ;
#17921 = CARTESIAN_POINT ( 'NONE',  ( -0.2349999999999999312, 0.000000000000000000, 0.000000000000000000 ) ) ;
#17922 = EDGE_CURVE ( 'NONE', #13839, #12748, #1460, .T. ) ;
#17923 = CIRCLE ( 'NONE', #30418, 0.08749999999977552123 ) ;
#17924 = CARTESIAN_POINT ( 'NONE',  ( 0.01548846960707524721, 0.000000000000000000, 0.000000000000000000 ) ) ;
#17925 = EDGE_CURVE ( 'NONE', #40377, #14064, #15239, .T. ) ;
#17926 = CARTESIAN_POINT ( 'NONE',  ( 0.003124719664520334353, -0.5686731593868922241, 0.1635439462316863046 ) ) ;
#17927 = DIRECTION ( 'NONE',  ( 1.000000000000000000, -1.609192080949047896E-13, 1.762723797404871399E-11 ) ) ;
#17928 = PERSON_AND_ORGANIZATION ( #28500, #32463 ) ;
#17929 = CIRCLE ( 'NONE', #4760, 0.01500000000000004628 ) ;
#17930 = CARTESIAN_POINT ( 'NONE',  ( 0.6419406851146725046, -1.339736372716090917, 0.8215813590131169075 ) ) ;
#17931 = AXIS2_PLACEMENT_3D ( 'NONE', #6198, #36200, #20379 ) ;
#17932 = CARTESIAN_POINT ( 'NONE',  ( 0.4043366342594306162, -1.595583149648728272, -0.6186662175067518810 ) ) ;
#17933 = CARTESIAN_POINT ( 'NONE',  ( 0.05201840200954339216, -0.01807554437688853669, -0.4701299851801460372 ) ) ;
#17934 = B_SPLINE_CURVE_WITH_KNOTS ( 'NONE', 3,
 ( #16177, #13073, #34671, #6478, #28499, #577, #28291, #25624, #10194, #28715, #3199, #3398, #19253, #12455, #18854, #374, #25835, #9775 ),
 .UNSPECIFIED., .F., .F.,
 ( 4, 2, 2, 2, 2, 2, 2, 2, 4 ),
 ( 0.000000000000000000, 0.0007746617437634299155, 0.001549323487526859397, 0.002323985231290289204, 0.003098646975053718795, 0.003873308718817148385, 0.004647970462580578409, 0.005422632206344008866, 0.006197293950107437589 ),
 .UNSPECIFIED. ) ;
#17935 = VECTOR ( 'NONE', #14033, 39.37007874015748143 ) ;
#17936 = EDGE_CURVE ( 'NONE', #35047, #38442, #24437, .T. ) ;
#17937 = CARTESIAN_POINT ( 'NONE',  ( -0.08000000000000000167, -2.698373762442814350, -0.2370085142459261163 ) ) ;
#17938 = VERTEX_POINT ( 'NONE', #7491 ) ;
#17939 = CARTESIAN_POINT ( 'NONE',  ( 0.4730652175054185782, -1.158518077264399260, -0.6186948529734398461 ) ) ;
#17940 = APPLIED_PERSON_AND_ORGANIZATION_ASSIGNMENT ( #1730, #1132, ( #13386 ) ) ;
#17941 = CARTESIAN_POINT ( 'NONE',  ( 0.1793448322649782434, -1.306301048382400465, 0.9356552813208593999 ) ) ;
#17942 = CARTESIAN_POINT ( 'NONE',  ( 0.1287628997187199309, -0.5693032371059245644, 0.2349318639996405556 ) ) ;
#17943 = CARTESIAN_POINT ( 'NONE',  ( 0.3778411022549617582, -1.761430872877596698, -0.4448008592944453499 ) ) ;
#17945 = ORIENTED_EDGE ( 'NONE', *, *, #1372, .F. ) ;
#17944 = DIRECTION ( 'NONE',  ( 0.000000000000000000, 0.000000000000000000, -1.000000000000000000 ) ) ;
#17946 = CARTESIAN_POINT ( 'NONE',  ( 0.6170741104697204937, -1.294989041298300947, 0.6128831306409553425 ) ) ;
#17948 = VERTEX_POINT ( 'NONE', #1560 ) ;
#17947 = EDGE_LOOP ( 'NONE', ( #29033, #37625, #2289, #15371 ) ) ;
#17949 = CARTESIAN_POINT ( 'NONE',  ( 0.06635375273718516209, -1.430634853383571770, -0.6831062175902198330 ) ) ;
#17950 = CARTESIAN_POINT ( 'NONE',  ( 0.3580990748662325474, -1.735866295672110038, -0.5196385737601301180 ) ) ;
#17951 = CYLINDRICAL_SURFACE ( 'NONE', #38385, 0.2500000000000000000 ) ;
#17952 = DATE_AND_TIME ( #12202, #16190 ) ;
#17953 = VECTOR ( 'NONE', #26630, 39.37007874015748143 ) ;
#17954 = DIRECTION ( 'NONE',  ( -0.8660512985181133550, -0.4999551463232372317, 0.000000000000000000 ) ) ;
#17955 = VERTEX_POINT ( 'NONE', #32600 ) ;
#17956 = CARTESIAN_POINT ( 'NONE',  ( 0.2374407952065339944, -0.9329004813706425203, 0.6724982063807530830 ) ) ;
#17957 = CIRCLE ( 'NONE', #4184, 0.9087847906030154244 ) ;
#17958 = CARTESIAN_POINT ( 'NONE',  ( 0.2243373955775073425, -1.373658029840927997, 1.035783466587031132 ) ) ;
#17959 = CIRCLE ( 'NONE', #24560, 0.9237847906030128842 ) ;
#17960 = CARTESIAN_POINT ( 'NONE',  ( 0.1177320669826718569, -0.6536998228781175646, 0.4362173610713035443 ) ) ;
#17962 = CARTESIAN_POINT ( 'NONE',  ( -0.001619896210524758443, -0.8333112946399738874, 0.06168507148062359058 ) ) ;
#17961 = CARTESIAN_POINT ( 'NONE',  ( -0.2399999999999999079, -3.985676108854518507, -0.7623095129438225426 ) ) ;
#17963 = CARTESIAN_POINT ( 'NONE',  ( 0.01081354071025426335, -1.017577864057874315, 0.5450223083628769061 ) ) ;
#17964 = ORIENTED_EDGE ( 'NONE', *, *, #13267, .T. ) ;
#17965 = ORIENTED_EDGE ( 'NONE', *, *, #22888, .T. ) ;
#17966 = CARTESIAN_POINT ( 'NONE',  ( -2.359223927328458141E-16, -0.02999999999999984276, -0.1699999999999995404 ) ) ;
#17967 = CARTESIAN_POINT ( 'NONE',  ( 0.6157026484039241909, -1.296264186265224438, 0.8027992624428816892 ) ) ;
#17968 = EDGE_CURVE ( 'NONE', #38602, #39658, #29037, .T. ) ;
#17969 = VECTOR ( 'NONE', #15966, 39.37007874015748854 ) ;
#17970 = DIRECTION ( 'NONE',  ( -6.162975822039154730E-33, 0.000000000000000000, -1.000000000000000000 ) ) ;
#17971 = ADVANCED_FACE ( 'NONE', ( #14082 ), #39191, .T. ) ;
#17972 = CARTESIAN_POINT ( 'NONE',  ( 0.03113248654051816583, 0.6410130462957083219, -0.4300623794142587886 ) ) ;
#17973 = EDGE_CURVE ( 'NONE', #35865, #11425, #32997, .T. ) ;
#17974 = DIRECTION ( 'NONE',  ( 0.4747798520620616913, 0.000000000000000000, -0.8801045915548485477 ) ) ;
#17975 = EDGE_CURVE ( 'NONE', #6091, #8779, #10005, .T. ) ;
#17976 = CARTESIAN_POINT ( 'NONE',  ( 0.1852394899523307770, -1.940955445487499098, -0.6926550664574201432 ) ) ;
#17977 = EDGE_CURVE ( 'NONE', #15024, #8017, #1883, .T. ) ;
#17978 = CARTESIAN_POINT ( 'NONE',  ( 0.3172427931101068910, -1.184417370245142376, 0.5253393887875316137 ) ) ;
#17979 = CARTESIAN_POINT ( 'NONE',  ( 0.1937691639527174270, -0.6993326081247003279, 0.2764035553309984738 ) ) ;
#17980 = COORDINATED_UNIVERSAL_TIME_OFFSET ( 0, 0, .AHEAD. ) ;
#17981 = CARTESIAN_POINT ( 'NONE',  ( -0.1102510911460846676, -0.5035121463812856080, 0.3528822442262287695 ) ) ;
#17982 = CIRCLE ( 'NONE', #35082, 0.05000000000000000971 ) ;
#17983 = DIRECTION ( 'NONE',  ( 0.4999551463232372317, -0.8660512985181133550, 0.000000000000000000 ) ) ;
#17984 = DIRECTION ( 'NONE',  ( 1.000000000000000000, 0.000000000000000000, 0.000000000000000000 ) ) ;
#17985 = DIRECTION ( 'NONE',  ( -0.3468893892380646160, -0.9373665302208734618, -0.03180785525185502588 ) ) ;
#17986 = B_SPLINE_CURVE_WITH_KNOTS ( 'NONE', 3,
 ( #6896, #12465, #9172, #6079, #6295, #25227, #19058, #37976, #31595, #18867 ),
 .UNSPECIFIED., .F., .F.,
 ( 4, 2, 2, 2, 4 ),
 ( 0.007788013979030915246, 0.009512064120430865563, 0.01037408919113082945, 0.01080510172648081225, 0.01123611426183079333 ),
 .UNSPECIFIED. ) ;
#17987 = CIRCLE ( 'NONE', #23276, 0.1000000000000000194 ) ;
#17988 = ADVANCED_FACE ( 'NONE', ( #33601 ), #7427, .F. ) ;
#17989 = ORIENTED_EDGE ( 'NONE', *, *, #35078, .F. ) ;
#17990 = CARTESIAN_POINT ( 'NONE',  ( 0.7303750569129517922, -1.407367292694915895, -0.5155029497116575543 ) ) ;
#17991 = CARTESIAN_POINT ( 'NONE',  ( 0.2012009467146754493, -0.8934095266790128553, 0.6235197419108591266 ) ) ;
#17992 = CARTESIAN_POINT ( 'NONE',  ( -0.03170752374382680705, 0.05433200130547150702, -0.4888275802721897545 ) ) ;
#17993 = VECTOR ( 'NONE', #28496, 39.37007874015748854 ) ;
#17994 = CARTESIAN_POINT ( 'NONE',  ( 0.01696032325262748774, -0.8707704970672307532, 0.4345434047485409179 ) ) ;
#17995 = ORIENTED_EDGE ( 'NONE', *, *, #500, .T. ) ;
#17996 = CARTESIAN_POINT ( 'NONE',  ( 0.01548846960707528191, -0.4770632572900429524, 0.2530032579707506835 ) ) ;
#17997 = VECTOR ( 'NONE', #20785, 39.37007874015748854 ) ;
#17998 = CARTESIAN_POINT ( 'NONE',  ( 0.05201840200954539056, 0.01807554437689167307, 0.4701299851801462593 ) ) ;
#17999 = CARTESIAN_POINT ( 'NONE',  ( 0.05201782277452800252, -0.4415348900197206272, -0.1624722611720488818 ) ) ;
#18000 = CARTESIAN_POINT ( 'NONE',  ( 0.3579113904514451550, -1.818604591836422868, -0.5224471374048138550 ) ) ;
#18001 = CARTESIAN_POINT ( 'NONE',  ( 0.4262369507677812308, -1.179622181167630179, 0.6860357087046927704 ) ) ;
#18003 = CARTESIAN_POINT ( 'NONE',  ( 0.0004750592482352814579, -0.4386115460793976739, 0.1457185332388683252 ) ) ;
#18002 = CARTESIAN_POINT ( 'NONE',  ( 0.04574984450155244325, 0.4792536329485966862, 0.08732079948164367389 ) ) ;
#18004 = CARTESIAN_POINT ( 'NONE',  ( -0.05634301242525835418, -0.2780425975185365495, -0.3652000572937718070 ) ) ;
#18005 = ORIENTED_EDGE ( 'NONE', *, *, #24480, .T. ) ;
#18006 = FACE_OUTER_BOUND ( 'NONE', #33965, .T. ) ;
#18007 = ORIENTED_EDGE ( 'NONE', *, *, #31371, .F. ) ;
#18008 =( BOUNDED_SURFACE ( )  B_SPLINE_SURFACE ( 3, 2, ( 
 ( #28763, #10034, #13116 ),
 ( #19513, #2002, #13911 ),
 ( #36550, #14332, #29561 ),
 ( #29981, #17627, #36130 ),
 ( #26284, #5066, #14527 ),
 ( #30174, #26483, #1608 ),
 ( #27090, #23209, #20930 ),
 ( #17426, #33452, #5257 ),
 ( #4456, #7752, #39236 ),
 ( #38805, #24026, #14133 ),
 ( #17816, #30376, #7546 ),
 ( #4854, #17020, #29763 ),
 ( #26703, #10855, #11058 ),
 ( #13718, #23816, #36337 ),
 ( #8155, #39624, #1816 ),
 ( #11461, #8361, #26895 ),
 ( #20317, #10635, #23616 ),
 ( #20729, #35735, #32837 ),
 ( #23428, #35946, #33048 ),
 ( #20121, #32651, #33256 ),
 ( #1403, #39021, #4645 ),
 ( #17218, #7940, #20516 ),
 ( #11245, #39423, #34259 ),
 ( #12065, #18639, #8551 ),
 ( #34474, #37543, #15136 ),
 ( #40639, #31200, #6071 ),
 ( #8763, #11660, #40025 ),
 ( #3017, #24630, #21124 ) ),
 .UNSPECIFIED., .F., .F., .F. ) 
 B_SPLINE_SURFACE_WITH_KNOTS ( ( 4, 2, 2, 2, 2, 2, 2, 2, 2, 2, 2, 2, 2, 4 ),
 ( 3, 3 ),
 ( 0.002672765802653568300, 0.003643729169957819151, 0.004614692537262070002, 0.005100174220914195644, 0.005585655904566321286, 0.006071137588218446929, 0.006556619271870572571, 0.007042100955522698214, 0.007527582639174823856, 0.008013064322826949498, 0.008498546006479075141, 0.008984027690131200783, 0.009469509373783326425, 0.01044047274108757771 ),
 ( 0.000000000000000000, 1.000000000000000000 ),
 .UNSPECIFIED. ) 
 GEOMETRIC_REPRESENTATION_ITEM ( )  RATIONAL_B_SPLINE_SURFACE ( (
 ( 1.000000000000000000, 0.7094119666599625340, 1.000000000000000000),
 ( 1.000000000000000000, 0.7091975995508440489, 1.000000000000000000),
 ( 1.000000000000000000, 0.7089641823995880276, 1.000000000000000000),
 ( 1.000000000000000000, 0.7085568111716973316, 1.000000000000000000),
 ( 1.000000000000000000, 0.7083776127384138199, 1.000000000000000000),
 ( 1.000000000000000000, 0.7081748109123476853, 1.000000000000000000),
 ( 1.000000000000000000, 0.7081166372635343542, 1.000000000000000000),
 ( 1.000000000000000000, 0.7080222590712177411, 1.000000000000000000),
 ( 1.000000000000000000, 0.7079861540317865520, 1.000000000000000000),
 ( 1.000000000000000000, 0.7079344075164385464, 1.000000000000000000),
 ( 1.000000000000000000, 0.7079189101953833330, 1.000000000000000000),
 ( 1.000000000000000000, 0.7079093227531754184, 1.000000000000000000),
 ( 1.000000000000000000, 0.7079148671191604070, 1.000000000000000000),
 ( 1.000000000000000000, 0.7079463893497752736, 1.000000000000000000),
 ( 1.000000000000000000, 0.7079724427870122128, 1.000000000000000000),
 ( 1.000000000000000000, 0.7080416038675461099, 1.000000000000000000),
 ( 1.000000000000000000, 0.7080851831062294766, 1.000000000000000000),
 ( 1.000000000000000000, 0.7081858060029823099, 1.000000000000000000),
 ( 1.000000000000000000, 0.7082416808879808956, 1.000000000000000000),
 ( 1.000000000000000000, 0.7083570905282395858, 1.000000000000000000),
 ( 1.000000000000000000, 0.7084173298865795720, 1.000000000000000000),
 ( 1.000000000000000000, 0.7085256194978258870, 1.000000000000000000),
 ( 1.000000000000000000, 0.7085739217061582940, 1.000000000000000000),
 ( 1.000000000000000000, 0.7086427899149944087, 1.000000000000000000),
 ( 1.000000000000000000, 0.7086627554150931596, 1.000000000000000000),
 ( 1.000000000000000000, 0.7086506118568940416, 1.000000000000000000),
 ( 1.000000000000000000, 0.7085441098889576628, 1.000000000000000000),
 ( 1.000000000000000000, 0.7082931127450711184, 1.000000000000000000) ) ) 
 REPRESENTATION_ITEM ( '' )  SURFACE ( )  );
#18009 = CARTESIAN_POINT ( 'NONE',  ( 0.7471327741883029283, -1.536404953935046391, -0.5155029497116575543 ) ) ;
#18010 = CARTESIAN_POINT ( 'NONE',  ( 0.4311562402287792972, -1.539438156933338631, 0.7516812456913292140 ) ) ;
#18012 = FACE_BOUND ( 'NONE', #26675, .T. ) ;
#18011 = FACE_OUTER_BOUND ( 'NONE', #13002, .T. ) ;
#18013 = DIRECTION ( 'NONE',  ( -1.000000000000000000, 0.000000000000000000, 0.000000000000000000 ) ) ;
#18014 = ORIENTED_EDGE ( 'NONE', *, *, #2858, .F. ) ;
#18015 = AXIS2_PLACEMENT_3D ( 'NONE', #19227, #16346, #35269 ) ;
#18016 = CARTESIAN_POINT ( 'NONE',  ( 0.4448603323116310793, -1.593566437326633833, -0.6098708555474791071 ) ) ;
#18017 = CARTESIAN_POINT ( 'NONE',  ( 0.3902240973675495384, -1.938317844694748882, -0.2990241803344498850 ) ) ;
#18018 = VECTOR ( 'NONE', #25529, 39.37007874015748143 ) ;
#18019 = CARTESIAN_POINT ( 'NONE',  ( 0.1222542343297059741, -0.5526425588814477541, 0.1793279953326599452 ) ) ;
#18020 = CARTESIAN_POINT ( 'NONE',  ( 0.4865950407719751292, -1.661532037359216840, 0.5397203252285756037 ) ) ;
#18021 = DIRECTION ( 'NONE',  ( 1.000000000000000000, 1.373428330785185865E-31, -7.771561172376106630E-16 ) ) ;
#18022 = VECTOR ( 'NONE', #16745, 39.37007874015748143 ) ;
#18023 = EDGE_CURVE ( 'NONE', #28184, #10938, #27859, .T. ) ;
#18024 = CIRCLE ( 'NONE', #336, 0.1000000000000000194 ) ;
#18025 = DIRECTION ( 'NONE',  ( 0.000000000000000000, -0.7071067811865474617, -0.7071067811865474617 ) ) ;
#18026 = AXIS2_PLACEMENT_3D ( 'NONE', #3301, #678, #19571 ) ;
#18027 = DIRECTION ( 'NONE',  ( 1.000000000000000000, 0.000000000000000000, 0.000000000000000000 ) ) ;
#18028 = ADVANCED_FACE ( 'NONE', ( #33410 ), #9351, .T. ) ;
#18029 = DIRECTION ( 'NONE',  ( 2.465190328815661892E-32, 1.000000000000000000, -5.978086547377980964E-31 ) ) ;
#18030 = CARTESIAN_POINT ( 'NONE',  ( -0.1455608194604310901, -0.5249067277714107860, 0.3749999999999998335 ) ) ;
#18031 = ADVANCED_FACE ( 'NONE', ( #9117 ), #21682, .F. ) ;
#18032 = AXIS2_PLACEMENT_3D ( 'NONE', #13475, #23152, #25833 ) ;
#18033 = CARTESIAN_POINT ( 'NONE',  ( 0.1914513227106267590, -0.5214848928147161056, 0.2513073325497693911 ) ) ;
#18034 = CIRCLE ( 'NONE', #2279, 1.991674066779348218 ) ;
#18035 = CARTESIAN_POINT ( 'NONE',  ( -0.03303708955568322031, 0.2303604322856135367, 0.4672397951413029826 ) ) ;
#18036 = CARTESIAN_POINT ( 'NONE',  ( -0.1630570426857087529, 0.4726602372414832054, 0.3374198529391165269 ) ) ;
#18037 = CARTESIAN_POINT ( 'NONE',  ( 0.6350421536969704794, -1.594263220348614007, -0.5890555079769790314 ) ) ;
#18038 = CARTESIAN_POINT ( 'NONE',  ( 0.2626070881998294193, -0.6796769646063650638, 0.05684369497733833543 ) ) ;
#18039 = CYLINDRICAL_SURFACE ( 'NONE', #11601, 0.1000000000000000194 ) ;
#18040 = CARTESIAN_POINT ( 'NONE',  ( 0.3940498717738633028, -1.740175311725885576, -0.4363121077653914215 ) ) ;
#18041 = DIRECTION ( 'NONE',  ( 1.060606950627616773E-16, 6.122684696619993730E-17, 1.000000000000000000 ) ) ;
#18042 = EDGE_CURVE ( 'NONE', #30547, #4481, #34319, .T. ) ;
#18043 = ORIENTED_EDGE ( 'NONE', *, *, #14478, .F. ) ;
#18044 = CARTESIAN_POINT ( 'NONE',  ( 0.003300039066125767893, -0.4845961630426517952, 0.3648084845760091732 ) ) ;
#18045 = CARTESIAN_POINT ( 'NONE',  ( -0.2746410161513782033, -1.835749455202394298, -0.3938319975228649072 ) ) ;
#18046 = EDGE_CURVE ( 'NONE', #30357, #25200, #9932, .T. ) ;
#18047 = AXIS2_PLACEMENT_3D ( 'NONE', #14509, #14728, #20714 ) ;
#18048 = CARTESIAN_POINT ( 'NONE',  ( 0.1760551381089313916, -1.265079013133070474, 0.5412798231591671172 ) ) ;
#18049 = CARTESIAN_POINT ( 'NONE',  ( 0.3740960844805631957, -1.108072201694596526, 0.5182417262812423209 ) ) ;
#18050 = EDGE_CURVE ( 'NONE', #24506, #27821, #31356, .T. ) ;
#18051 = CIRCLE ( 'NONE', #26617, 0.1000000000000000194 ) ;
#18052 = CIRCLE ( 'NONE', #39081, 0.01000000000000007827 ) ;
#18053 = ORIENTED_EDGE ( 'NONE', *, *, #15982, .F. ) ;
#18054 = DIRECTION ( 'NONE',  ( -0.3468893892380659483, 0.7770416411310542282, -0.5252371270030326000 ) ) ;
#18055 = ADVANCED_FACE ( 'NONE', ( #12610 ), #17907, .T. ) ;
#18056 = DIRECTION ( 'NONE',  ( 0.8660512985181124668, 0.4999551463232388415, 0.000000000000000000 ) ) ;
#18057 = LOCAL_TIME ( 0, 53, 7.000000000000000000, #8413 ) ;
#18058 = CARTESIAN_POINT ( 'NONE',  ( 0.3422943015738595385, -1.758122929102525989, 0.4605087972123807494 ) ) ;
#18059 = CARTESIAN_POINT ( 'NONE',  ( -0.1304423469995336093, -0.5262799683630398073, 0.3749999999999999445 ) ) ;
#18060 = CARTESIAN_POINT ( 'NONE',  ( 0.4290884103726456122, -1.188868616449923366, 0.7477856797621026397 ) ) ;
#18062 = ORIENTED_EDGE ( 'NONE', *, *, #2898, .F. ) ;
#18061 = CARTESIAN_POINT ( 'NONE',  ( -0.1710642718812839524, 0.4986889572247744096, 0.1528658435937167159 ) ) ;
#18063 = CARTESIAN_POINT ( 'NONE',  ( 0.3318484986314376162, -0.9704704429389122700, 0.6048456486855374736 ) ) ;
#18064 = EDGE_LOOP ( 'NONE', ( #18945, #4522, #9292, #20991 ) ) ;
#18065 = CARTESIAN_POINT ( 'NONE',  ( -0.01548846960707517956, -0.09061086148575756005, -0.5171215251571035232 ) ) ;
#18066 = EDGE_LOOP ( 'NONE', ( #3381, #27520, #36594, #3326 ) ) ;
#18067 = CARTESIAN_POINT ( 'NONE',  ( 0.1499999999999993561, 0.000000000000000000, 0.000000000000000000 ) ) ;
#18068 = EDGE_LOOP ( 'NONE', ( #39822, #25161, #15429 ) ) ;
#18069 = CARTESIAN_POINT ( 'NONE',  ( 0.2040651102238323633, -1.191688104741121856, 0.8916119944643040585 ) ) ;
#18071 = CARTESIAN_POINT ( 'NONE',  ( 0.1771057343352051561, -0.4639829428808278089, 0.08932164138973593126 ) ) ;
#18070 = DIRECTION ( 'NONE',  ( 0.000000000000000000, 0.9510565162951502005, -0.3090169943749580539 ) ) ;
#18072 = DIRECTION ( 'NONE',  ( 0.4999551463232372317, -0.8660512985181135770, 0.000000000000000000 ) ) ;
#18073 = ORIENTED_EDGE ( 'NONE', *, *, #25547, .T. ) ;
#18074 = VERTEX_POINT ( 'NONE', #15468 ) ;
#18075 = CARTESIAN_POINT ( 'NONE',  ( 0.4041790769229076097, -0.9940227595139969896, 0.7031909273260571469 ) ) ;
#18076 = CARTESIAN_POINT ( 'NONE',  ( 0.1162211104444988985, -0.5562432141033685218, 0.1993352053206045305 ) ) ;
#18077 = ORIENTED_EDGE ( 'NONE', *, *, #5471, .F. ) ;
#18078 = CARTESIAN_POINT ( 'NONE',  ( 0.2047952255614176320, -1.936887964834772102, -0.3318900947218276776 ) ) ;
#18079 = DIRECTION ( 'NONE',  ( 0.000000000000000000, -1.610603102373135995E-15, -1.000000000000000000 ) ) ;
#18080 = CARTESIAN_POINT ( 'NONE',  ( 0.1224489045975470647, -0.8957878257233655717, 0.5611759970749146120 ) ) ;
#18081 = CARTESIAN_POINT ( 'NONE',  ( 0.005374783099221854855, -1.803624522921790652, -0.3583957701598275980 ) ) ;
#18082 = CIRCLE ( 'NONE', #4936, 0.03000000000000007175 ) ;
#18083 = ADVANCED_FACE ( 'NONE', ( #25345 ), #3520, .T. ) ;
#18084 = CARTESIAN_POINT ( 'NONE',  ( -0.1499999999999996336, -7.971802777789936683E-17, -0.1750000000000000167 ) ) ;
#18085 = CIRCLE ( 'NONE', #29242, 0.1000000000000000194 ) ;
#18086 = EDGE_CURVE ( 'NONE', #35323, #23884, #34974, .T. ) ;
#18087 = CARTESIAN_POINT ( 'NONE',  ( 0.1822807072488307478, -0.9686607882321045526, 0.5003333243558089061 ) ) ;
#18088 = CARTESIAN_POINT ( 'NONE',  ( 0.6601361389616772213, -1.566348459635070522, 0.5707417262808793801 ) ) ;
#18089 = CARTESIAN_POINT ( 'NONE',  ( -0.2746410161513779258, -4.250025578259899461, -0.8852376261118949374 ) ) ;
#18090 = DIRECTION ( 'NONE',  ( 0.000000000000000000, 0.000000000000000000, -1.000000000000000000 ) ) ;
#18091 = CARTESIAN_POINT ( 'NONE',  ( 0.04965997019300262549, -1.266850117287420696, 0.6475152895583352608 ) ) ;
#18092 = APPROVAL_ROLE ( '' ) ;
#18093 = LOCAL_TIME ( 0, 53, 7.000000000000000000, #17980 ) ;
#18094 = CARTESIAN_POINT ( 'NONE',  ( 0.4842989215684344595, -1.127184663968222589, 0.5007281051682350714 ) ) ;
#18095 = CARTESIAN_POINT ( 'NONE',  ( 0.03868264068766501251, -0.4417248602032650684, 0.1788646266443654487 ) ) ;
#18096 = AXIS2_PLACEMENT_3D ( 'NONE', #8000, #29828, #27555 ) ;
#18097 = DIRECTION ( 'NONE',  ( 0.000000000000000000, 0.9901182710308955581, -0.1402348365092997984 ) ) ;
#18098 = CARTESIAN_POINT ( 'NONE',  ( 1.621299365906332885E-05, -0.4335896441111527500, 0.08190102398457659028 ) ) ;
#18099 = DIRECTION ( 'NONE',  ( 0.000000000000000000, 3.330669073875470114E-16, 1.000000000000000000 ) ) ;
#18100 = CARTESIAN_POINT ( 'NONE',  ( 0.3204139389452037023, -1.755336229099433654, 0.4849083929475442867 ) ) ;
#18101 = DIRECTION ( 'NONE',  ( -1.000000000000000000, -0.000000000000000000, -0.000000000000000000 ) ) ;
#18102 = ORIENTED_EDGE ( 'NONE', *, *, #15062, .T. ) ;
#18103 = ORIENTED_EDGE ( 'NONE', *, *, #31535, .T. ) ;
#18104 = DIRECTION ( 'NONE',  ( 1.000000000000000000, 6.779273404243070203E-32, 4.314083075427408311E-32 ) ) ;
#18105 = ORIENTED_EDGE ( 'NONE', *, *, #12296, .T. ) ;
#18106 = DIRECTION ( 'NONE',  ( 1.000000000000000000, 1.450080480853946466E-15, -8.881784197001242463E-16 ) ) ;
#18108 = ORIENTED_EDGE ( 'NONE', *, *, #28166, .F. ) ;
#18107 = CARTESIAN_POINT ( 'NONE',  ( -0.1092363788443093259, -0.4985689912534735369, 0.1005717796975812012 ) ) ;
#18110 = VERTEX_POINT ( 'NONE', #9273 ) ;
#18109 = FACE_BOUND ( 'NONE', #16310, .T. ) ;
#18111 = AXIS2_PLACEMENT_3D ( 'NONE', #10833, #20492, #23409 ) ;
#18112 = CIRCLE ( 'NONE', #6906, 0.5400000000000018119 ) ;
#18113 = EDGE_LOOP ( 'NONE', ( #6821, #14304 ) ) ;
#18114 = CARTESIAN_POINT ( 'NONE',  ( 0.02953079040095728247, 0.000000000000000000, 0.000000000000000000 ) ) ;
#18115 = EDGE_LOOP ( 'NONE', ( #9846, #34345, #4846, #7316 ) ) ;
#18116 = CARTESIAN_POINT ( 'NONE',  ( 0.2685697523530611308, -1.675616378658084438, 0.6036540740780101943 ) ) ;
#18118 = CARTESIAN_POINT ( 'NONE',  ( 0.2112634585974465518, -1.245876612383048032, 0.5715387936656939338 ) ) ;
#18117 = CYLINDRICAL_SURFACE ( 'NONE', #376, 0.08000000000000000167 ) ;
#18119 = LOCAL_TIME ( 0, 53, 7.000000000000000000, #15779 ) ;
#18120 = CARTESIAN_POINT ( 'NONE',  ( 0.2547684209294985291, -1.595179263533379910, -0.3507741123912141989 ) ) ;
#18121 = CARTESIAN_POINT ( 'NONE',  ( 0.4953328006973022335, -1.658154532889615895, 0.5682417262808785452 ) ) ;
#18123 = ORIENTED_EDGE ( 'NONE', *, *, #31579, .F. ) ;
#18122 = ORIENTED_EDGE ( 'NONE', *, *, #24794, .T. ) ;
#18124 = CARTESIAN_POINT ( 'NONE',  ( 0.01138352277355129775, -0.9296896336311132325, 0.05438588250771710098 ) ) ;
#18125 = CIRCLE ( 'NONE', #4315, 0.01500000000000004281 ) ;
#18126 = CARTESIAN_POINT ( 'NONE',  ( 0.3405242896115940887, -1.744906522954217110, 0.4484829386635745263 ) ) ;
#18127 = CARTESIAN_POINT ( 'NONE',  ( -0.04945776359514589965, -0.4635931069071527189, 0.1136454792236764738 ) ) ;
#18128 = CARTESIAN_POINT ( 'NONE',  ( 0.4280571948436235341, -1.214389859197892108, 0.8188955122002271603 ) ) ;
#18129 = CARTESIAN_POINT ( 'NONE',  ( 0.1868462052469743451, -0.7315845167432759588, 0.03397798300244578296 ) ) ;
#18130 = DIRECTION ( 'NONE',  ( 0.000000000000000000, 0.3882559824134196313, -0.9215515678030125057 ) ) ;
#18131 = DIRECTION ( 'NONE',  ( -1.000000000000000000, -2.403560570595279103E-31, 1.725633230170969455E-31 ) ) ;
#18132 = LINE ( 'NONE', #36232, #20692 ) ;
#18133 = CARTESIAN_POINT ( 'NONE',  ( 0.4034340626290945364, -1.711742532993089982, 0.4219718062392947555 ) ) ;
#18134 = CARTESIAN_POINT ( 'NONE',  ( 0.3324871086615415194, -1.659137217475705306, -0.6399689536651991251 ) ) ;
#18135 = CARTESIAN_POINT ( 'NONE',  ( 0.1999999999999786671, -2.166079853131637645, -0.4467913981637915977 ) ) ;
#18136 = DIRECTION ( 'NONE',  ( 0.3779644730092246441, 0.000000000000000000, 0.9258200997725524184 ) ) ;
#18137 = CARTESIAN_POINT ( 'NONE',  ( 0.4370114410068630106, -1.106456163932805881, 0.5863244257242559154 ) ) ;
#18138 = CARTESIAN_POINT ( 'NONE',  ( 0.3999999999999787059, -2.166079853131637645, -0.4467913981637915422 ) ) ;
#18139 = AXIS2_PLACEMENT_3D ( 'NONE', #29471, #1724, #10753 ) ;
#18140 = CARTESIAN_POINT ( 'NONE',  ( 0.07216878364870311924, 0.08000000000000023759, 0.1249999999999999029 ) ) ;
#18141 = CARTESIAN_POINT ( 'NONE',  ( 0.005216780649377962716, -0.5315740328921342295, 0.3610413699792206499 ) ) ;
#18142 = CARTESIAN_POINT ( 'NONE',  ( 0.08354342017514641838, -1.252940714712708958, 0.7526680972150427973 ) ) ;
#18143 = PERSON_AND_ORGANIZATION_ROLE ( 'classification_officer' ) ;
#18144 = CARTESIAN_POINT ( 'NONE',  ( 0.5633425123490871655, -1.213831759034801561, 0.8533915188341715252 ) ) ;
#18145 = SECURITY_CLASSIFICATION ( '', '', #3754 ) ;
#18146 = CARTESIAN_POINT ( 'NONE',  ( -0.05464101615137795936, -1.598492537578166672, -0.2771380022280826028 ) ) ;
#18147 = AXIS2_PLACEMENT_3D ( 'NONE', #20685, #29940, #11624 ) ;
#18148 = CARTESIAN_POINT ( 'NONE',  ( 0.04308611741967211667, 0.05688666786373643147, -0.4910246251072729051 ) ) ;
#18149 = LINE ( 'NONE', #11974, #32292 ) ;
#18150 = ORIENTED_EDGE ( 'NONE', *, *, #31394, .T. ) ;
#18151 = CARTESIAN_POINT ( 'NONE',  ( 0.6568730927750874304, -1.460570608776338597, 0.4224083929475443977 ) ) ;
#18152 = CARTESIAN_POINT ( 'NONE',  ( 0.05418309106442487783, -0.8367704788373211411, 0.7042074783075930045 ) ) ;
#18153 = CARTESIAN_POINT ( 'NONE',  ( 0.5875422609861711276, -1.491128227361789182, 0.5657178549513129928 ) ) ;
#18155 = ORIENTED_EDGE ( 'NONE', *, *, #27330, .F. ) ;
#18154 = CARTESIAN_POINT ( 'NONE',  ( 0.3702892772755569384, -1.736523176964394732, 0.4320996613930846442 ) ) ;
#18156 = CARTESIAN_POINT ( 'NONE',  ( 0.1909052096321314784, -0.5854118129141068216, 0.1777712087850742972 ) ) ;
#18158 = VERTEX_POINT ( 'NONE', #31494 ) ;
#18157 = EDGE_LOOP ( 'NONE', ( #7266, #38703, #26912, #20196 ) ) ;
#18159 = CARTESIAN_POINT ( 'NONE',  ( 0.1817870711851117815, -1.296977422222274523, -0.7345968740143652420 ) ) ;
#18160 = DIRECTION ( 'NONE',  ( 1.000000000000000000, 2.341930812374887555E-31, -1.664003471950578127E-31 ) ) ;
#18161 = LINE ( 'NONE', #11988, #2266 ) ;
#18162 = COORDINATED_UNIVERSAL_TIME_OFFSET ( 0, 0, .AHEAD. ) ;
#18163 = CARTESIAN_POINT ( 'NONE',  ( -0.02953079040095628327, 0.4684706630666132243, -0.2484463060367378962 ) ) ;
#18164 = VERTEX_POINT ( 'NONE', #3304 ) ;
#18165 = CONICAL_SURFACE ( 'NONE', #10286, 0.5614999999999926716, 1.047197551196600296 ) ;
#18166 = CARTESIAN_POINT ( 'NONE',  ( 0.08829421125485691080, -0.7067105924166853237, 0.2075677057826203209 ) ) ;
#18167 = CARTESIAN_POINT ( 'NONE',  ( 0.3227739583020200476, -1.719409737019245155, 0.8075189798695981969 ) ) ;
#18168 = CARTESIAN_POINT ( 'NONE',  ( 0.4974589431443675047, -1.542506574375496209, 0.5734728255214222026 ) ) ;
#18170 = CARTESIAN_POINT ( 'NONE',  ( -0.0003951118247478632847, -0.7312479731468258803, -0.01669275631305656288 ) ) ;
#18169 = DIRECTION ( 'NONE',  ( 0.8660512985181130219, 0.4999551463232378978, 0.000000000000000000 ) ) ;
#18171 = CARTESIAN_POINT ( 'NONE',  ( 0.05992090360963508999, -1.332693131100006756, 0.5682417262808777680 ) ) ;
#18172 = APPROVAL_PERSON_ORGANIZATION ( #2293, #1494, #14407 ) ;
#18173 = ORIENTED_EDGE ( 'NONE', *, *, #19793, .T. ) ;
#18174 = ORIENTED_EDGE ( 'NONE', *, *, #2225, .T. ) ;
#18175 = CARTESIAN_POINT ( 'NONE',  ( -0.1589779575897145303, 0.4935643744415411649, 0.1021333108076148272 ) ) ;
#18176 = CARTESIAN_POINT ( 'NONE',  ( 0.3001519255637661865, -0.8839599682347554221, 0.8021632040787142204 ) ) ;
#18177 = CIRCLE ( 'NONE', #32620, 1.986674066779353875 ) ;
#18178 = CARTESIAN_POINT ( 'NONE',  ( 0.02953079040095704308, -0.3810518745593846068, 0.3687679460475796756 ) ) ;
#18179 = EDGE_CURVE ( 'NONE', #37196, #9415, #3118, .T. ) ;
#18180 = CARTESIAN_POINT ( 'NONE',  ( 0.3699999999999786793, -2.097675824466503691, -0.4685644896151254235 ) ) ;
#18181 = APPLIED_DATE_AND_TIME_ASSIGNMENT ( #12305, #200, ( #38779 ) ) ;
#18182 = DIRECTION ( 'NONE',  ( 1.000000000000000000, 1.169383359989551318E-31, -7.771561172376106630E-16 ) ) ;
#18183 = CARTESIAN_POINT ( 'NONE',  ( 0.4062230848227143531, -1.145582794160930895, 0.4248905050063966349 ) ) ;
#18184 = CARTESIAN_POINT ( 'NONE',  ( 0.2606473226204091831, -1.679216544086299612, 0.4886760040442115205 ) ) ;
#18185 = CARTESIAN_POINT ( 'NONE',  ( 0.3207953251618635981, -1.182327106099470448, 0.4907902897447509183 ) ) ;
#18186 = CARTESIAN_POINT ( 'NONE',  ( 0.5317104447742054818, -1.152447470094080328, 0.6575248185080280194 ) ) ;
#18187 = DATE_TIME_ROLE ( 'creation_date' ) ;
#18188 = CARTESIAN_POINT ( 'NONE',  ( 0.1901359855603551308, -0.5909830539303996266, 0.3021763630842474457 ) ) ;
#18189 = AXIS2_PLACEMENT_3D ( 'NONE', #23775, #36291, #37118 ) ;
#18190 = CARTESIAN_POINT ( 'NONE',  ( 0.3697217270809275425, -2.079157444975821001, -0.5163575626078683589 ) ) ;
#18191 = CARTESIAN_POINT ( 'NONE',  ( -0.01548846960707524721, 0.000000000000000000, 0.000000000000000000 ) ) ;
#18192 = CARTESIAN_POINT ( 'NONE',  ( 0.6059691746655119227, -1.480133143157562170, 0.5526975506195443977 ) ) ;
#18193 = EDGE_CURVE ( 'NONE', #9291, #33568, #4096, .T. ) ;
#18194 = ORIENTED_EDGE ( 'NONE', *, *, #9731, .F. ) ;
#18195 = CARTESIAN_POINT ( 'NONE',  ( 0.4841659176569872991, -1.131373688278120238, 0.4858252441513852826 ) ) ;
#18196 = CARTESIAN_POINT ( 'NONE',  ( -0.04085667396267390200, -0.2941474082995332862, 0.3688418229621477362 ) ) ;
#18197 = CARTESIAN_POINT ( 'NONE',  ( 0.2209338557910215939, -0.9109865339892553315, 0.6537527485991542209 ) ) ;
#18198 = EDGE_LOOP ( 'NONE', ( #32314, #25773, #4355, #13893 ) ) ;
#18199 = CARTESIAN_POINT ( 'NONE',  ( -0.04085667396267567836, 0.02117046819985016898, -0.4712948116111316255 ) ) ;
#18200 = EDGE_CURVE ( 'NONE', #32882, #34195, #19375, .T. ) ;
#18201 = CARTESIAN_POINT ( 'NONE',  ( 0.01310383523850323917, -0.8587138684673197853, 0.3611815158424811489 ) ) ;
#18203 = ORIENTED_EDGE ( 'NONE', *, *, #21550, .T. ) ;
#18202 = VERTEX_POINT ( 'NONE', #37666 ) ;
#18204 = EDGE_CURVE ( 'NONE', #7855, #31436, #9487, .T. ) ;
#18205 = CARTESIAN_POINT ( 'NONE',  ( -0.1167294258596054818, -0.5331983345538300334, 0.1478951491071729685 ) ) ;
#18206 = CARTESIAN_POINT ( 'NONE',  ( 0.05076679145662072595, 0.04886774829954446814, 0.4712599967968605363 ) ) ;
#18207 = CARTESIAN_POINT ( 'NONE',  ( 0.05078310099560560953, -0.4330765661303609404, -0.1920364777915913590 ) ) ;
#18208 = CARTESIAN_POINT ( 'NONE',  ( 0.1888132638007787578, -1.709137045139594857, -0.3586210806981278143 ) ) ;
#18209 = EDGE_CURVE ( 'NONE', #16210, #12748, #14607, .T. ) ;
#18210 = CARTESIAN_POINT ( 'NONE',  ( 0.4306335752601955780, -1.183459269765066102, 0.6683203921661764468 ) ) ;
#18212 = CARTESIAN_POINT ( 'NONE',  ( 0.1633160071118299750, -1.272099323608264276, 0.4248106349649071189 ) ) ;
#18211 = CARTESIAN_POINT ( 'NONE',  ( 0.03474824846560953945, 0.5087747035359670988, 0.08925086559848140200 ) ) ;
#18213 = EDGE_CURVE ( 'NONE', #25941, #26629, #26342, .T. ) ;
#18214 = CARTESIAN_POINT ( 'NONE',  ( 0.02238826743733619493, -0.3549908576167588592, -0.3695531484129501720 ) ) ;
#18215 = ORIENTED_EDGE ( 'NONE', *, *, #17708, .T. ) ;
#18216 = ORIENTED_EDGE ( 'NONE', *, *, #20268, .T. ) ;
#18217 = EDGE_CURVE ( 'NONE', #14778, #27248, #11328, .T. ) ;
#18218 = ORIENTED_EDGE ( 'NONE', *, *, #39336, .F. ) ;
#18219 = DIRECTION ( 'NONE',  ( -0.4887635750373022780, -0.8724162812079766516, -1.864855553833737887E-16 ) ) ;
#18220 = CARTESIAN_POINT ( 'NONE',  ( 0.4417812153713224221, -1.573793491951804402, 0.5750929000743407737 ) ) ;
#18222 = CARTESIAN_POINT ( 'NONE',  ( 0.5623656178733204003, -1.618086598301832435, 0.5064396494810395888 ) ) ;
#18221 = CARTESIAN_POINT ( 'NONE',  ( -0.1157923916715208196, -0.5295015842444287246, 0.1380392329925462791 ) ) ;
#18223 = CARTESIAN_POINT ( 'NONE',  ( 0.4737925448037723086, -1.158599824872910800, 0.4226906129777907029 ) ) ;
#18224 = CARTESIAN_POINT ( 'NONE',  ( 0.1262945646573275515, -1.315309522507558837, -0.3176315144292584103 ) ) ;
#18225 = ORIENTED_EDGE ( 'NONE', *, *, #29900, .T. ) ;
#18226 = PRODUCT_DEFINITION_CONTEXT ( 'detailed design', #40545, 'design' ) ;
#18227 = CARTESIAN_POINT ( 'NONE',  ( -0.2900000000000008127, 0.5182417262804733804, 0.3600000000000000422 ) ) ;
#18228 = CARTESIAN_POINT ( 'NONE',  ( 0.1818679406367339213, -1.742646577052884727, -0.3269862635956189978 ) ) ;
#18229 = CARTESIAN_POINT ( 'NONE',  ( 0.1226644528301022302, -0.5666400526987965813, 0.2303931865571023363 ) ) ;
#18230 = CARTESIAN_POINT ( 'NONE',  ( 0.4722973099718666412, -1.670488640416608606, 0.5579311128194459624 ) ) ;
#18231 = DIRECTION ( 'NONE',  ( 0.4999551463232373427, -0.8660512985181134660, 0.000000000000000000 ) ) ;
#18232 = EDGE_CURVE ( 'NONE', #19186, #3583, #29264, .T. ) ;
#18233 = ORIENTED_EDGE ( 'NONE', *, *, #9756, .F. ) ;
#18234 = CARTESIAN_POINT ( 'NONE',  ( -0.03158843595483497996, 0.4819971762524428716, 0.09920191295802914533 ) ) ;
#18235 = APPLIED_DATE_AND_TIME_ASSIGNMENT ( #8002, #35997, ( #7895 ) ) ;
#18236 = CARTESIAN_POINT ( 'NONE',  ( 0.2059273467974226113, -1.283046334493782803, -0.3194715457588298557 ) ) ;
#18237 = DIRECTION ( 'NONE',  ( 0.000000000000000000, 5.978086547377980964E-31, 1.000000000000000000 ) ) ;
#18238 = LINE ( 'NONE', #28112, #36498 ) ;
#18239 = AXIS2_PLACEMENT_3D ( 'NONE', #16908, #34655, #22328 ) ;
#18240 = CARTESIAN_POINT ( 'NONE',  ( 0.2033263846434442690, -0.5675993867538808857, 0.3776288918835234987 ) ) ;
#18241 = CARTESIAN_POINT ( 'NONE',  ( -0.02953079040095645327, 0.3810518745593871048, 0.3687679460475778437 ) ) ;
#18242 = CARTESIAN_POINT ( 'NONE',  ( -0.1707627412572631231, 0.4977336986496899707, 0.3126474374754099061 ) ) ;
#18243 = CARTESIAN_POINT ( 'NONE',  ( 0.6138443103785190536, -1.548954526385655672, -0.4055369609750524296 ) ) ;
#18244 = CARTESIAN_POINT ( 'NONE',  ( 0.1354314573857386406, -1.346930980521078736, -0.7110692366758478711 ) ) ;
#18245 = LINE ( 'NONE', #27707, #35901 ) ;
#18246 = CARTESIAN_POINT ( 'NONE',  ( 0.08411373178446444887, 0.05688556330967591695, 0.1043107429350861731 ) ) ;
#18247 = ADVANCED_FACE ( 'NONE', ( #29834 ), #1466, .F. ) ;
#18248 = FACE_OUTER_BOUND ( 'NONE', #40104, .T. ) ;
#18249 = ORIENTED_EDGE ( 'NONE', *, *, #1156, .F. ) ;
#18250 = DIRECTION ( 'NONE',  ( 0.000000000000000000, 0.000000000000000000, -1.000000000000000000 ) ) ;
#18251 = CARTESIAN_POINT ( 'NONE',  ( 0.5948637837280855711, -1.483193241468645507, -0.6457934574185902887 ) ) ;
#18252 = CARTESIAN_POINT ( 'NONE',  ( -0.05464101615137761936, -1.845925619402022155, -0.3444148183989317880 ) ) ;
#18253 = CARTESIAN_POINT ( 'NONE',  ( 0.3699999999999786793, -2.097675824466503691, -0.4688691127277797022 ) ) ;
#18255 = ORIENTED_EDGE ( 'NONE', *, *, #24649, .F. ) ;
#18254 = B_SPLINE_SURFACE_WITH_KNOTS ( 'NONE', 3, 3, ( 
 ( #27648, #2556, #21499, #18184 ),
 ( #24361, #18811, #6431, #19002 ),
 ( #31355, #12609, #3158, #2966 ),
 ( #40178, #8708, #21284, #15701 ) ),
 .UNSPECIFIED., .F., .F., .F.,
 ( 4, 4 ),
 ( 4, 4 ),
 ( -6.214954718652347943, -5.911709546377296398 ),
 ( -1.271269362639431799, -0.03735764515002289871 ),
 .UNSPECIFIED. ) ;
#18256 = EDGE_CURVE ( 'NONE', #1239, #5197, #16508, .T. ) ;
#18257 = CARTESIAN_POINT ( 'NONE',  ( 0.5014952879983503031, -1.689753520674470710, -0.5927250297527999479 ) ) ;
#18258 =( BOUNDED_SURFACE ( )  B_SPLINE_SURFACE ( 3, 2, ( 
 ( #40282, #25480, #10247 ),
 ( #25893, #12930, #6939 ),
 ( #810, #19512, #38015 ),
 ( #16609, #26100, #4261 ) ),
 .UNSPECIFIED., .F., .F., .T. ) 
 B_SPLINE_SURFACE_WITH_KNOTS ( ( 4, 4 ),
 ( 3, 3 ),
 ( -3.816391647148975608E-16, 0.002151548051257935051 ),
 ( 0.000000000000000000, 0.7423884024711013829 ),
 .UNSPECIFIED. ) 
 GEOMETRIC_REPRESENTATION_ITEM ( )  RATIONAL_B_SPLINE_SURFACE ( (
 ( 1.000000000000000000, 0.7823248912590446968, 0.8878487349899315539),
 ( 1.000000000000000000, 0.7825950437676943983, 0.8879879238285908194),
 ( 1.000000000000000000, 0.7825604363545956010, 0.8879700932866414487),
 ( 1.000000000000000000, 0.7825594711904613199, 0.8879695960116924525) ) ) 
 REPRESENTATION_ITEM ( '' )  SURFACE ( )  );
#18259 = CARTESIAN_POINT ( 'NONE',  ( 0.3672888026336380562, -1.149235926965803012, 0.6020051486042412581 ) ) ;
#18260 = DIRECTION ( 'NONE',  ( -1.000000000000000000, -0.000000000000000000, -0.000000000000000000 ) ) ;
#18261 = CARTESIAN_POINT ( 'NONE',  ( 0.02881195911414642305, 0.3393447726770189576, -0.3647551865608069654 ) ) ;
#18262 = EDGE_CURVE ( 'NONE', #31712, #9001, #23830, .T. ) ;
#18263 = CARTESIAN_POINT ( 'NONE',  ( 0.4508755845972571286, -1.219119228265584276, 0.7279328556006846584 ) ) ;
#18265 = ORIENTED_EDGE ( 'NONE', *, *, #37528, .F. ) ;
#18264 = CARTESIAN_POINT ( 'NONE',  ( -0.01548846960707538425, -0.4638115001430989648, 0.2459753896937853235 ) ) ;
#18266 = CARTESIAN_POINT ( 'NONE',  ( 0.2957689212018802527, -0.9454471935599602084, 0.5654756054326123271 ) ) ;
#18267 = ORIENTED_EDGE ( 'NONE', *, *, #21493, .F. ) ;
#18268 = APPROVAL_ROLE ( '' ) ;
#18269 = ADVANCED_FACE ( 'NONE', ( #17076 ), #2149, .T. ) ;
#18270 = VECTOR ( 'NONE', #34666, 39.37007874015748143 ) ;
#18271 = CARTESIAN_POINT ( 'NONE',  ( 0.1720329558925851321, -1.269480774308429982, -0.3269759641248038973 ) ) ;
#18272 = ORIENTED_EDGE ( 'NONE', *, *, #32808, .T. ) ;
#18273 = CARTESIAN_POINT ( 'NONE',  ( 0.3495654075459491694, -1.736963291591081759, -0.5687247700623858648 ) ) ;
#18274 = ORIENTED_EDGE ( 'NONE', *, *, #35292, .T. ) ;
#18275 = CARTESIAN_POINT ( 'NONE',  ( 0.03561864634767011872, -0.5348410626444256577, 0.1638778232741606444 ) ) ;
#18277 = CARTESIAN_POINT ( 'NONE',  ( 0.1760631799394591079, -0.6276024324974762703, -0.07686131200774137806 ) ) ;
#18276 = DIRECTION ( 'NONE',  ( 0.8660512985181130219, 0.4999551463232378978, -4.627692199633250344E-15 ) ) ;
#18278 = CARTESIAN_POINT ( 'NONE',  ( -0.01548846960707531660, -0.2306506793134055211, -0.4716198300880352634 ) ) ;
#18279 = ORIENTED_EDGE ( 'NONE', *, *, #24850, .T. ) ;
#18280 = CARTESIAN_POINT ( 'NONE',  ( 0.3979951050334158968, -1.018748020539158805, 0.6285197686894602453 ) ) ;
#18281 = CARTESIAN_POINT ( 'NONE',  ( 0.5529634792074666905, -1.511186030616493259, 0.5729129695539203482 ) ) ;
#18283 = ORIENTED_EDGE ( 'NONE', *, *, #36131, .F. ) ;
#18282 = B_SPLINE_CURVE_WITH_KNOTS ( 'NONE', 3,
 ( #14746, #23211, #11462, #20931, #14529, #26896 ),
 .UNSPECIFIED., .F., .F.,
 ( 4, 2, 4 ),
 ( 0.000000000000000000, 0.5000000000000000000, 1.000000000000000000 ),
 .UNSPECIFIED. ) ;
#18284 = FACE_OUTER_BOUND ( 'NONE', #19091, .T. ) ;
#18285 = DIRECTION ( 'NONE',  ( 0.000000000000000000, 0.000000000000000000, -1.000000000000000000 ) ) ;
#18286 = EDGE_CURVE ( 'NONE', #16916, #6325, #38575, .T. ) ;
#18287 = B_SPLINE_CURVE_WITH_KNOTS ( 'NONE', 3,
 ( #23536, #27213, #20423, #24327, #23718, #36245 ),
 .UNSPECIFIED., .F., .F.,
 ( 4, 2, 4 ),
 ( 0.005049958045009090429, 0.005976456838057345525, 0.006902955631105599753 ),
 .UNSPECIFIED. ) ;
#18288 = CARTESIAN_POINT ( 'NONE',  ( 0.05370873345334652160, -1.468804715554985707, -0.3745649705647907113 ) ) ;
#18289 = EDGE_CURVE ( 'NONE', #26169, #10778, #27105, .T. ) ;
#18290 = CARTESIAN_POINT ( 'NONE',  ( -0.1212602504878778492, -0.5073146173917499890, 0.3048175120576743780 ) ) ;
#18291 = EDGE_CURVE ( 'NONE', #2983, #26971, #16586, .T. ) ;
#18292 = CARTESIAN_POINT ( 'NONE',  ( -0.02000000000000000042, -2.691615088641019504, -0.5143267481657003426 ) ) ;
#18293 = LINE ( 'NONE', #27962, #17997 ) ;
#18294 = CARTESIAN_POINT ( 'NONE',  ( 0.6540709664215760277, -1.593060928864740156, 0.5182417262812423209 ) ) ;
#18295 = CARTESIAN_POINT ( 'NONE',  ( 0.03113248654051816583, 0.6304109427692223822, -0.1442409525262416947 ) ) ;
#18296 = CARTESIAN_POINT ( 'NONE',  ( 1.365923996832131609E-16, -0.9481888444201347355, 0.09803024984676507458 ) ) ;
#18297 = PERSON_AND_ORGANIZATION ( #28500, #32463 ) ;
#18298 = CARTESIAN_POINT ( 'NONE',  ( 0.4829265164743086758, -1.123232261319281333, 0.5052793004277540412 ) ) ;
#18299 = CARTESIAN_POINT ( 'NONE',  ( 0.03662792686184294239, -0.4431041838557951418, 0.1872093443778323762 ) ) ;
#18300 = VECTOR ( 'NONE', #33202, 39.37007874015748854 ) ;
#18301 = CARTESIAN_POINT ( 'NONE',  ( 0.5705655853683049283, -1.576197229824741974, -0.5665877336259347308 ) ) ;
#18302 = CARTESIAN_POINT ( 'NONE',  ( 0.001991602493628476505, -0.9268535620581923595, 0.4078208622452191290 ) ) ;
#18303 = CARTESIAN_POINT ( 'NONE',  ( -0.02000000000000000042, -2.183180860297908144, -0.4937760292030871079 ) ) ;
#18304 = CARTESIAN_POINT ( 'NONE',  ( 0.01645090811047977483, -0.5819932753755481247, 0.5292683286643183882 ) ) ;
#18305 = CARTESIAN_POINT ( 'NONE',  ( 0.1993697748527691604, -1.286830511351394923, -0.2901526353474664366 ) ) ;
#18306 = ORIENTED_EDGE ( 'NONE', *, *, #14430, .T. ) ;
#18307 = ORIENTED_EDGE ( 'NONE', *, *, #20572, .T. ) ;
#18308 = DIRECTION ( 'NONE',  ( 0.000000000000000000, 0.000000000000000000, -1.000000000000000000 ) ) ;
#18309 = EDGE_LOOP ( 'NONE', ( #28928, #26522, #13101, #38678 ) ) ;
#18310 = DIRECTION ( 'NONE',  ( 0.000000000000000000, 0.000000000000000000, 1.000000000000000000 ) ) ;
#18311 = EDGE_CURVE ( 'NONE', #24913, #27710, #1084, .T. ) ;
#18312 = CARTESIAN_POINT ( 'NONE',  ( -0.1127285386967662312, -0.5155187098906055532, 0.1369073159183774313 ) ) ;
#18314 = ORIENTED_EDGE ( 'NONE', *, *, #24981, .F. ) ;
#18313 = CARTESIAN_POINT ( 'NONE',  ( 0.2637382839637063547, -0.6009449316864781121, 0.1932256475537140750 ) ) ;
#18315 = ORIENTED_EDGE ( 'NONE', *, *, #21821, .T. ) ;
#18316 = CARTESIAN_POINT ( 'NONE',  ( -0.02000000000000000042, -2.183180860297908144, -0.4312760292030870524 ) ) ;
#18317 = ORIENTED_EDGE ( 'NONE', *, *, #28166, .T. ) ;
#18318 = CARTESIAN_POINT ( 'NONE',  ( 0.2667337750453726564, -1.675443482348580648, 0.5781907244941091317 ) ) ;
#18320 = CARTESIAN_POINT ( 'NONE',  ( 0.08995075563790964901, -1.315447267446937074, 0.5712668678535780531 ) ) ;
#18319 = CARTESIAN_POINT ( 'NONE',  ( 0.06443582815874832059, -0.8352844082028780814, 0.1887074755868990705 ) ) ;
#18321 = PLANE ( 'NONE',  #12796 ) ;
#18322 = DIRECTION ( 'NONE',  ( 1.000000000000000000, 2.341930812374887555E-31, -1.664003471950578127E-31 ) ) ;
#18324 = ORIENTED_EDGE ( 'NONE', *, *, #32560, .F. ) ;
#18323 = ORIENTED_EDGE ( 'NONE', *, *, #20318, .T. ) ;
#18325 = CARTESIAN_POINT ( 'NONE',  ( 0.3516693977051734143, -1.145166927642649046, 0.6147136096956975493 ) ) ;
#18326 = DIRECTION ( 'NONE',  ( 0.9998941247116546194, -0.01455087607601020239, 0.0001066420868422379362 ) ) ;
#18327 = CARTESIAN_POINT ( 'NONE',  ( -0.04574984450155034077, -0.4792536329486041247, 0.08732079948164171712 ) ) ;
#18328 = CARTESIAN_POINT ( 'NONE',  ( 0.3234613948553985430, -1.057064862004813088, 0.7871205450755927036 ) ) ;
#18329 = DIRECTION ( 'NONE',  ( 0.000000000000000000, 0.000000000000000000, -1.000000000000000000 ) ) ;
#18330 = DIRECTION ( 'NONE',  ( -7.771561172376107616E-16, 7.170354002788761615E-17, -1.000000000000000000 ) ) ;
#18331 = EDGE_CURVE ( 'NONE', #5340, #9944, #11972, .T. ) ;
#18332 = APPLIED_DATE_AND_TIME_ASSIGNMENT ( #40109, #17515, ( #30020 ) ) ;
#18333 = CARTESIAN_POINT ( 'NONE',  ( 0.2117376410295460365, -1.291494683274178268, 1.029451941043375562 ) ) ;
#18334 = CARTESIAN_POINT ( 'NONE',  ( 0.3804897312162703882, -1.724958420852153118, 0.4230015755326726468 ) ) ;
#18335 = EDGE_CURVE ( 'NONE', #24709, #14547, #9662, .T. ) ;
#18336 = CARTESIAN_POINT ( 'NONE',  ( 0.2616322387702281205, -1.678013124025769187, 0.5382687897764735219 ) ) ;
#18337 = CARTESIAN_POINT ( 'NONE',  ( 0.3922353094782703997, -1.714330012172307294, 0.4177417262808784115 ) ) ;
#18338 = CARTESIAN_POINT ( 'NONE',  ( 0.3998620935691268308, -1.132090473766685035, 0.6053150776564958369 ) ) ;
#18339 = DIRECTION ( 'NONE',  ( 0.000000000000000000, -0.8063205929144886541, 0.5914787413272157846 ) ) ;
#18340 =( LENGTH_UNIT ( ) NAMED_UNIT ( * ) SI_UNIT ( $, .METRE. ) );
#18341 = DIRECTION ( 'NONE',  ( 0.000000000000000000, 0.000000000000000000, -1.000000000000000000 ) ) ;
#18342 = CARTESIAN_POINT ( 'NONE',  ( 0.04961935711675592720, -0.7636540146707464505, 0.7296111229395446651 ) ) ;
#18343 = CARTESIAN_POINT ( 'NONE',  ( 0.06061003669112926401, -1.113841305498648904, 0.7547552038151051912 ) ) ;
#18344 = PRODUCT_CONTEXT ( 'NONE', #35544, 'mechanical' ) ;
#18345 = CARTESIAN_POINT ( 'NONE',  ( 0.7110913793137424443, -1.453804679565707803, 0.7028629728786995878 ) ) ;
#18346 = CARTESIAN_POINT ( 'NONE',  ( 0.6863592619258633842, -1.545543250144949310, 0.6049187728663865116 ) ) ;
#18347 = CARTESIAN_POINT ( 'NONE',  ( 0.04946288932100178365, -0.03516002272507855186, -0.4760097007310896688 ) ) ;
#18348 = CARTESIAN_POINT ( 'NONE',  ( 0.3445219659099013620, -1.630113034087284030, -0.4330379103484557346 ) ) ;
#18349 = ORIENTED_EDGE ( 'NONE', *, *, #2155, .T. ) ;
#18350 = CARTESIAN_POINT ( 'NONE',  ( 0.03113248654051816583, -0.2276394436010286959, -0.1339480508475833498 ) ) ;
#18351 = CARTESIAN_POINT ( 'NONE',  ( 0.2568884488902449248, -1.570716599475997510, 0.8655622903500216347 ) ) ;
#18352 = EDGE_CURVE ( 'NONE', #9503, #26696, #34643, .T. ) ;
#18353 = CARTESIAN_POINT ( 'NONE',  ( 0.1311038971828588640, -0.5870549638996708230, 0.2845027658977437590 ) ) ;
#18355 = ORIENTED_EDGE ( 'NONE', *, *, #36419, .F. ) ;
#18354 = PLANE ( 'NONE',  #9948 ) ;
#18356 = CARTESIAN_POINT ( 'NONE',  ( 0.5549275037195743332, -1.190966985655177890, 0.5563916622750778584 ) ) ;
#18358 = EDGE_LOOP ( 'NONE', ( #35561, #31722, #20822, #34792, #9145, #35058, #7284, #8396, #5243, #24193, #34336, #13760, #26767, #32572 ) ) ;
#18357 = ORIENTED_EDGE ( 'NONE', *, *, #6117, .F. ) ;
#18359 = CARTESIAN_POINT ( 'NONE',  ( 0.6513739094900949933, -1.353581159747916374, 0.7728549212624699072 ) ) ;
#18360 = CARTESIAN_POINT ( 'NONE',  ( 0.6424732214804906860, -1.458111371101026954, -0.4022076521922505754 ) ) ;
#18361 = CARTESIAN_POINT ( 'NONE',  ( 0.3401273707089542131, -1.774294669406801583, 0.5182417262812423209 ) ) ;
#18362 = APPROVAL_ROLE ( '' ) ;
#18363 = B_SPLINE_CURVE_WITH_KNOTS ( 'NONE', 3,
 ( #18192, #11629, #24186, #27055, #39584, #14486 ),
 .UNSPECIFIED., .F., .F.,
 ( 4, 2, 4 ),
 ( 0.0008740713857989025094, 0.001092763134855501183, 0.001311454883912099856 ),
 .UNSPECIFIED. ) ;
#18364 = CARTESIAN_POINT ( 'NONE',  ( -0.04285561529641556539, 0.4433460678679621014, -0.2197428102801899097 ) ) ;
#18365 = EDGE_LOOP ( 'NONE', ( #38889, #37950, #9821, #34131, #17141, #23687 ) ) ;
#18366 = CARTESIAN_POINT ( 'NONE',  ( 0.2343816454659662929, -0.9209986304437879356, 0.6741416622544036397 ) ) ;
#18367 = CARTESIAN_POINT ( 'NONE',  ( 0.3086358606916266845, -1.716562723882868680, 0.8052685041170501989 ) ) ;
#18368 = CARTESIAN_POINT ( 'NONE',  ( 0.5251400411238811294, -1.526848766764422827, 0.5721117033549915076 ) ) ;
#18370 = CARTESIAN_POINT ( 'NONE',  ( 0.0004851977134181738034, -0.6337081043291690197, -0.01359677011322422274 ) ) ;
#18369 = DIRECTION ( 'NONE',  ( -7.771561172376107616E-16, 7.170354002788761615E-17, -1.000000000000000000 ) ) ;
#18371 = CARTESIAN_POINT ( 'NONE',  ( -0.04582713223189532892, -0.3361263728083078717, 0.3523178389613212391 ) ) ;
#18372 = ORIENTED_EDGE ( 'NONE', *, *, #27805, .T. ) ;
#18373 = CARTESIAN_POINT ( 'NONE',  ( 0.4676456642793518359, -1.686044861640426884, 0.5768288019549496770 ) ) ;
#18374 = CARTESIAN_POINT ( 'NONE',  ( 0.5093620481516674126, -1.230189073184877468, 0.9022058255351600442 ) ) ;
#18375 = CARTESIAN_POINT ( 'NONE',  ( 0.2698036132048247104, -0.9625005881386677897, 0.7146062034794288254 ) ) ;
#18376 = CARTESIAN_POINT ( 'NONE',  ( 0.3690006080204021321, -2.059917255124906532, -0.5191234088178223738 ) ) ;
#18377 =( NAMED_UNIT ( * ) PLANE_ANGLE_UNIT ( ) SI_UNIT ( $, .RADIAN. ) );
#18378 = CARTESIAN_POINT ( 'NONE',  ( 0.6407227470148669779, -1.336152316681919805, 0.6057417262806679137 ) ) ;
#18379 = CARTESIAN_POINT ( 'NONE',  ( -2.104432723530627271E-14, -2.062071153782512933, -0.6845211759026355036 ) ) ;
#18380 = DIRECTION ( 'NONE',  ( -7.000205099780314469E-17, -1.000000000000000000, 6.590151126658399604E-16 ) ) ;
#18381 = CARTESIAN_POINT ( 'NONE',  ( 0.2393369856776542404, -0.7683812882957752333, 0.4887749849253086309 ) ) ;
#18382 = PERSON_AND_ORGANIZATION ( #28500, #32463 ) ;
#18383 = CARTESIAN_POINT ( 'NONE',  ( -0.1873388932668322293, 0.5325605939836577374, 0.3599999999999994316 ) ) ;
#18384 = FACE_OUTER_BOUND ( 'NONE', #31480, .T. ) ;
#18385 = PLANE ( 'NONE',  #36584 ) ;
#18386 = CARTESIAN_POINT ( 'NONE',  ( -0.03303708955568183253, -0.08827115631760176773, 0.5134073995267878221 ) ) ;
#18387 = ORIENTED_EDGE ( 'NONE', *, *, #34843, .F. ) ;
#18388 = CARTESIAN_POINT ( 'NONE',  ( 0.2169964291290918945, -1.302220840841494365, -0.4117811260064771495 ) ) ;
#18389 = CARTESIAN_POINT ( 'NONE',  ( -0.02953079040095632490, -0.2329676531120498939, 0.4763574306556330185 ) ) ;
#18390 = CIRCLE ( 'NONE', #8552, 0.01500000000000001506 ) ;
#18391 = LINE ( 'NONE', #28081, #4213 ) ;
#18392 = ORIENTED_EDGE ( 'NONE', *, *, #25359, .T. ) ;
#18393 = CARTESIAN_POINT ( 'NONE',  ( -0.04230258372739731376, -0.004226829447873794131, -0.4686050468223225129 ) ) ;
#18394 = CARTESIAN_POINT ( 'NONE',  ( 0.03183846471128804617, -0.9219432159619347367, 0.5839824611533311893 ) ) ;
#18396 = ORIENTED_EDGE ( 'NONE', *, *, #16779, .T. ) ;
#18395 = ORIENTED_EDGE ( 'NONE', *, *, #26543, .T. ) ;
#18397 = DIRECTION ( 'NONE',  ( 1.000000000000000000, 0.000000000000000000, 0.000000000000000000 ) ) ;
#18398 = VECTOR ( 'NONE', #124, 39.37007874015748143 ) ;
#18399 = VERTEX_POINT ( 'NONE', #23878 ) ;
#18400 = DIRECTION ( 'NONE',  ( -0.4999551463232377313, 0.8660512985181132439, 0.000000000000000000 ) ) ;
#18401 = CARTESIAN_POINT ( 'NONE',  ( 0.05279755784604278634, -0.4562001582273347844, -0.1062924750453443506 ) ) ;
#18402 = CARTESIAN_POINT ( 'NONE',  ( 0.3673504507587657120, -2.034217874421845096, -0.4825990138407615926 ) ) ;
#18403 = CARTESIAN_POINT ( 'NONE',  ( -0.2399999999999999079, -3.194091454214595949, -0.5766534813907827628 ) ) ;
#18405 = CARTESIAN_POINT ( 'NONE',  ( 0.1909286924077255032, -1.257064795538239022, -0.7462941026102624109 ) ) ;
#18404 = CARTESIAN_POINT ( 'NONE',  ( -0.05464101615137785528, -2.230494317742474308, -0.6487310457122437146 ) ) ;
#18406 = CYLINDRICAL_SURFACE ( 'NONE', #3358, 0.05000000000000000971 ) ;
#18407 = VERTEX_POINT ( 'NONE', #30041 ) ;
#18408 = CARTESIAN_POINT ( 'NONE',  ( 0.1396468697112676072, -0.6922978612330201731, 0.5287085477509265719 ) ) ;
#18409 = ORIENTED_EDGE ( 'NONE', *, *, #20732, .F. ) ;
#18410 = CARTESIAN_POINT ( 'NONE',  ( 0.7029356573940241937, -1.521348978687367515, 0.5776904582050019776 ) ) ;
#18411 = CARTESIAN_POINT ( 'NONE',  ( 0.4521839067189716843, -1.514453368521524235, 0.7626995238331509830 ) ) ;
#18412 = CARTESIAN_POINT ( 'NONE',  ( -0.03650581953630595983, -0.5059763899182400104, 0.07647306779615177519 ) ) ;
#18413 = CARTESIAN_POINT ( 'NONE',  ( 0.5643649638864810525, -1.503238486482124658, 0.4993898684233098462 ) ) ;
#18414 = DIRECTION ( 'NONE',  ( 0.4999551463232372872, -0.8660512985181134660, 0.000000000000000000 ) ) ;
#18415 = DIRECTION ( 'NONE',  ( 0.4999551463232373427, -0.8660512985181134660, 0.000000000000000000 ) ) ;
#18416 = CARTESIAN_POINT ( 'NONE',  ( 0.3932181676567889084, -1.978278275894043148, -0.4945254564861773505 ) ) ;
#18417 = CARTESIAN_POINT ( 'NONE',  ( 0.5321775012407692351, -1.423729542427319972, 0.7737387429086715063 ) ) ;
#18418 = CARTESIAN_POINT ( 'NONE',  ( 0.4290948641688455689, -1.693752172740113693, 0.4322454032524135070 ) ) ;
#18419 = B_SPLINE_CURVE_WITH_KNOTS ( 'NONE', 3,
 ( #38852, #5455, #24405, #36940 ),
 .UNSPECIFIED., .F., .F.,
 ( 4, 4 ),
 ( 0.000000000000000000, 0.001604995851825731599 ),
 .UNSPECIFIED. ) ;
#18420 = CARTESIAN_POINT ( 'NONE',  ( -0.06980746140711582837, 0.1750000000000001832, 0.000000000000000000 ) ) ;
#18421 = CARTESIAN_POINT ( 'NONE',  ( -0.2399999999999999079, -3.899630010830198668, -0.3430483616844877681 ) ) ;
#18422 = CARTESIAN_POINT ( 'NONE',  ( 0.5409081234724703036, -1.629499156560143325, 0.4182417262803311830 ) ) ;
#18423 = AXIS2_PLACEMENT_3D ( 'NONE', #22325, #28271, #136 ) ;
#18424 = DIRECTION ( 'NONE',  ( 0.000000000000000000, 0.000000000000000000, -1.000000000000000000 ) ) ;
#18425 = CARTESIAN_POINT ( 'NONE',  ( -0.2746410161513782033, -2.322955634169589612, -0.9336221289765171960 ) ) ;
#18426 = EDGE_CURVE ( 'NONE', #20959, #6091, #17673, .T. ) ;
#18427 = CARTESIAN_POINT ( 'NONE',  ( 0.2690787404081327883, -0.7149439305734058836, 0.6099944544563858928 ) ) ;
#18428 = ADVANCED_FACE ( 'NONE', ( #8828 ), #1935, .T. ) ;
#18429 = AXIS2_PLACEMENT_3D ( 'NONE', #31058, #2878, #31274 ) ;
#18430 = CARTESIAN_POINT ( 'NONE',  ( -0.03647137243075408014, 0.3644785006310322650, 0.3593174381849622012 ) ) ;
#18431 = CARTESIAN_POINT ( 'NONE',  ( 0.01861955870168061425, -0.9920946170940110331, 0.4882401372334904677 ) ) ;
#18433 = EDGE_CURVE ( 'NONE', #25042, #1588, #22426, .T. ) ;
#18432 = VECTOR ( 'NONE', #21983, 39.37007874015748143 ) ;
#18434 = CARTESIAN_POINT ( 'NONE',  ( 0.6327495122412205575, -1.496409968128172396, -0.3957395255592697225 ) ) ;
#18435 = MANIFOLD_SOLID_BREP ( 'Combine1', #14175 ) ;
#18436 = CARTESIAN_POINT ( 'NONE',  ( -0.06919656468380842862, -0.09959325338431362917, 0.09813923389047245205 ) ) ;
#18437 = CARTESIAN_POINT ( 'NONE',  ( 0.08509462337972205359, -0.8106601073492546439, 0.1910513156228427489 ) ) ;
#18438 = EDGE_CURVE ( 'NONE', #18789, #20299, #22216, .T. ) ;
#18439 = DIRECTION ( 'NONE',  ( 0.8660512985181135770, 0.4999551463232370652, 0.000000000000000000 ) ) ;
#18440 = FACE_OUTER_BOUND ( 'NONE', #2394, .T. ) ;
#18441 = ORIENTED_EDGE ( 'NONE', *, *, #28300, .T. ) ;
#18442 = CARTESIAN_POINT ( 'NONE',  ( 0.6723167204675445374, -1.568148218941692429, 0.6167698549942565167 ) ) ;
#18443 = CARTESIAN_POINT ( 'NONE',  ( 0.1499999999999994948, 0.2450655194479797461, -0.4674710490749308112 ) ) ;
#18444 = CARTESIAN_POINT ( 'NONE',  ( 0.6605962927874261537, -1.467029229620433917, 0.4224020735106358559 ) ) ;
#18445 = CARTESIAN_POINT ( 'NONE',  ( 0.4170115945640066046, -1.702980413955158756, -0.6123808887097250686 ) ) ;
#18446 = ORIENTED_EDGE ( 'NONE', *, *, #18335, .F. ) ;
#18447 = CARTESIAN_POINT ( 'NONE',  ( 0.5423380835500176689, -1.654573018669519335, -0.5568946855831939935 ) ) ;
#18448 = ADVANCED_FACE ( 'NONE', ( #38028 ), #232, .T. ) ;
#18449 = CARTESIAN_POINT ( 'NONE',  ( 0.3204450882031337211, -1.182672964233338675, 0.5682417262808777680 ) ) ;
#18450 = LINE ( 'NONE', #18664, #9265 ) ;
#18451 = APPLIED_PERSON_AND_ORGANIZATION_ASSIGNMENT ( #33830, #5822, ( #25768 ) ) ;
#18452 = DIRECTION ( 'NONE',  ( -8.881784197001246407E-16, 2.361472542561082612E-16, -1.000000000000000000 ) ) ;
#18453 = CARTESIAN_POINT ( 'NONE',  ( 0.4997376312364609774, -1.291901472916908045, 0.6589433602268506274 ) ) ;
#18454 = VECTOR ( 'NONE', #16345, 39.37007874015748143 ) ;
#18456 = VERTEX_POINT ( 'NONE', #15813 ) ;
#18455 = CARTESIAN_POINT ( 'NONE',  ( -0.1684323896977243107, 0.5231977508184618708, 0.1451849067762387424 ) ) ;
#18457 = CARTESIAN_POINT ( 'NONE',  ( 0.4130926557567901058, -1.028576094973266963, 0.6508837067575374835 ) ) ;
#18458 = ORIENTED_EDGE ( 'NONE', *, *, #10239, .F. ) ;
#18459 = PERSON_AND_ORGANIZATION ( #28500, #32463 ) ;
#18460 = CARTESIAN_POINT ( 'NONE',  ( -0.2399999999999999079, -2.888408042504194473, -0.3144735572646252253 ) ) ;
#18461 = ORIENTED_EDGE ( 'NONE', *, *, #23796, .F. ) ;
#18462 = EDGE_LOOP ( 'NONE', ( #5994, #29346, #33619 ) ) ;
#18463 = AXIS2_PLACEMENT_3D ( 'NONE', #32017, #787, #407 ) ;
#18464 = CARTESIAN_POINT ( 'NONE',  ( 0.3455691795635327801, -1.573870377985774338, 0.7908454336058577949 ) ) ;
#18466 = CARTESIAN_POINT ( 'NONE',  ( 0.1752893795992640225, -0.8297571003230018727, -0.03550332207696408476 ) ) ;
#18465 = CARTESIAN_POINT ( 'NONE',  ( 0.3663975874019590462, -1.157438136726378408, 0.4269148889825721827 ) ) ;
#18467 = DIRECTION ( 'NONE',  ( 0.000000000000000000, 0.000000000000000000, -1.000000000000000000 ) ) ;
#18468 = AXIS2_PLACEMENT_3D ( 'NONE', #16094, #31713, #35215 ) ;
#18469 = AXIS2_PLACEMENT_3D ( 'NONE', #33789, #2332, #30097 ) ;
#18470 = ORIENTED_EDGE ( 'NONE', *, *, #11717, .F. ) ;
#18471 = CARTESIAN_POINT ( 'NONE',  ( 0.4408732154518923418, -1.039102903811854883, 0.7181090867236722408 ) ) ;
#18472 = CARTESIAN_POINT ( 'NONE',  ( 0.1217566883381065168, -0.6226032096887995637, 0.3725731591225738271 ) ) ;
#18473 = ORIENTED_EDGE ( 'NONE', *, *, #26840, .T. ) ;
#18474 = PLANE ( 'NONE',  #4876 ) ;
#18475 = DIRECTION ( 'NONE',  ( 0.000000000000000000, 0.000000000000000000, -1.000000000000000000 ) ) ;
#18476 = CARTESIAN_POINT ( 'NONE',  ( 0.5934892211655993233, -1.486388914344519696, -0.3866566986715374021 ) ) ;
#18477 = B_SPLINE_CURVE_WITH_KNOTS ( 'NONE', 3,
 ( #22791, #3827, #22581, #996 ),
 .UNSPECIFIED., .F., .F.,
 ( 4, 4 ),
 ( 0.4999999999999995559, 1.000000000000000000 ),
 .UNSPECIFIED. ) ;
#18478 = CARTESIAN_POINT ( 'NONE',  ( -0.1105109110478834505, -0.5048634036869017461, 0.3351973644282421061 ) ) ;
#18479 = AXIS2_PLACEMENT_3D ( 'NONE', #22385, #802, #22594 ) ;
#18480 = DIRECTION ( 'NONE',  ( 0.4999551463232372317, -0.8660512985181135770, 0.000000000000000000 ) ) ;
#18481 = EDGE_CURVE ( 'NONE', #5206, #35865, #37603, .T. ) ;
#18482 = CARTESIAN_POINT ( 'NONE',  ( 0.6586301574024518990, -1.563739711041315816, 0.4687417262808791230 ) ) ;
#18483 = DIRECTION ( 'NONE',  ( 1.000000000000000000, 0.000000000000000000, 0.000000000000000000 ) ) ;
#18484 = CARTESIAN_POINT ( 'NONE',  ( 0.02022720027586020000, -1.618081545761635986, -0.6352904068409364058 ) ) ;
#18485 = CARTESIAN_POINT ( 'NONE',  ( 0.02115399423329476433, -1.083931147575175613, 0.6303919839426973537 ) ) ;
#18486 = DATE_AND_TIME ( #6536, #33180 ) ;
#18487 = ADVANCED_FACE ( 'NONE', ( #22409 ), #3678, .T. ) ;
#18488 = AXIS2_PLACEMENT_3D ( 'NONE', #6001, #9097, #7358 ) ;
#18489 = CARTESIAN_POINT ( 'NONE',  ( 0.3142644354089449421, -0.9846788231241262457, 0.5762604841115940291 ) ) ;
#18490 = CARTESIAN_POINT ( 'NONE',  ( 0.4557391318645251932, -1.137478852754574055, 0.4468712729341908219 ) ) ;
#18491 = ADVANCED_FACE ( 'NONE', ( #4274, #32663 ), #27461, .T. ) ;
#18492 = CARTESIAN_POINT ( 'NONE',  ( 0.4668197292635641871, -1.236307873514313149, 0.6057417262809816627 ) ) ;
#18493 = DIRECTION ( 'NONE',  ( 0.4999999999999988343, 3.389636702121526891E-32, -0.8660254037844391517 ) ) ;
#18494 = CIRCLE ( 'NONE', #27047, 0.1946589359789743512 ) ;
#18495 =( BOUNDED_SURFACE ( )  B_SPLINE_SURFACE ( 3, 2, ( 
 ( #35277, #34858, #25206 ),
 ( #35462, #3192, #19643 ),
 ( #22149, #148, #19449 ),
 ( #37749, #7263, #32177 ),
 ( #7072, #31987, #3988 ),
 ( #16355, #13470, #3799 ),
 ( #13065, #3600, #28890 ),
 ( #19038, #15732, #22750 ),
 ( #22945, #16551, #31569 ),
 ( #31388, #9571, #25428 ),
 ( #28282, #35069, #38559 ),
 ( #751, #22541, #15945 ),
 ( #28490, #25827, #12642 ),
 ( #37957, #13257, #25616 ) ),
 .UNSPECIFIED., .F., .F., .T. ) 
 B_SPLINE_SURFACE_WITH_KNOTS ( ( 4, 2, 2, 2, 2, 2, 4 ),
 ( 3, 3 ),
 ( 1.517883041479706208E-18, 0.0009569864225024638437, 0.001435479633753695061, 0.001913972845004926170, 0.002392466056256157495, 0.002870959267507388821, 0.003827945690009851038 ),
 ( 0.000000000000000000, 1.000000000000000000 ),
 .UNSPECIFIED. ) 
 GEOMETRIC_REPRESENTATION_ITEM ( )  RATIONAL_B_SPLINE_SURFACE ( (
 ( 1.000000000000000000, 0.7071067811865471286, 1.000000000000000000),
 ( 1.000000000000000000, 0.6948232385253381160, 1.000000000000000000),
 ( 1.000000000000000000, 0.6807618830700954415, 1.000000000000000000),
 ( 1.000000000000000000, 0.6583014577179361337, 1.000000000000000000),
 ( 1.000000000000000000, 0.6505217571340542460, 1.000000000000000000),
 ( 1.000000000000000000, 0.6345534479354342228, 1.000000000000000000),
 ( 1.000000000000000000, 0.6262961088974926538, 1.000000000000000000),
 ( 1.000000000000000000, 0.6089017105673123487, 1.000000000000000000),
 ( 1.000000000000000000, 0.5996869661009254227, 1.000000000000000000),
 ( 1.000000000000000000, 0.5806079066951357337, 1.000000000000000000),
 ( 1.000000000000000000, 0.5707163240679670180, 1.000000000000000000),
 ( 1.000000000000000000, 0.5396746807496910492, 1.000000000000000000),
 ( 1.000000000000000000, 0.5169777448399269781, 1.000000000000000000),
 ( 1.000000000000000000, 0.4928180116091783747, 1.000000000000000000) ) ) 
 REPRESENTATION_ITEM ( '' )  SURFACE ( )  );
#18496 = CARTESIAN_POINT ( 'NONE',  ( 0.1057086693319095883, -1.337907155632660716, 0.7376750060448485913 ) ) ;
#18497 = CARTESIAN_POINT ( 'NONE',  ( 0.4778170654558047126, -1.668016138613298560, 0.5682417262808788783 ) ) ;
#18498 = AXIS2_PLACEMENT_3D ( 'NONE', #9901, #25758, #7406 ) ;
#18499 = CARTESIAN_POINT ( 'NONE',  ( 0.0005053628357002480209, -0.4419962224268538242, 0.1895056222691282322 ) ) ;
#18500 = CARTESIAN_POINT ( 'NONE',  ( 0.3177853311222696431, -1.645584418359625545, 0.5133479035088005515 ) ) ;
#18501 = EDGE_LOOP ( 'NONE', ( #32614, #9308, #7400, #30397 ) ) ;
#18502 = ORIENTED_EDGE ( 'NONE', *, *, #20480, .F. ) ;
#18503 = EDGE_CURVE ( 'NONE', #2063, #2060, #27808, .T. ) ;
#18504 = CARTESIAN_POINT ( 'NONE',  ( -0.1049931804392591206, -0.4770575742336283231, 0.3602693336304588212 ) ) ;
#18505 = ORIENTED_EDGE ( 'NONE', *, *, #1524, .T. ) ;
#18506 = CARTESIAN_POINT ( 'NONE',  ( -0.2399999999999999079, -2.183180860297908144, -0.4937760292030871079 ) ) ;
#18507 = DIRECTION ( 'NONE',  ( -0.4999999999999977240, 0.4646411234949380242, -0.7308273574226432645 ) ) ;
#18508 = CARTESIAN_POINT ( 'NONE',  ( -0.02872242845530475694, -0.07817994906156883195, -0.5268390348591152073 ) ) ;
#18510 = ORIENTED_EDGE ( 'NONE', *, *, #8372, .T. ) ;
#18509 = FACE_OUTER_BOUND ( 'NONE', #294, .T. ) ;
#18511 = ORIENTED_EDGE ( 'NONE', *, *, #20793, .T. ) ;
#18512 = CARTESIAN_POINT ( 'NONE',  ( 0.03662792686184426078, 0.4431041838557911450, -0.1872093443778329869 ) ) ;
#18513 = EDGE_LOOP ( 'NONE', ( #35311, #32462, #23071, #31171, #11136 ) ) ;
#18514 = CARTESIAN_POINT ( 'NONE',  ( 0.03048937143879262845, -0.7350047429437137625, 0.5937430055735584133 ) ) ;
#18516 = CARTESIAN_POINT ( 'NONE',  ( 0.2672982121950731038, -1.328276981695355907, 0.4182417262808770797 ) ) ;
#18515 = CARTESIAN_POINT ( 'NONE',  ( 0.3599329779412693275, -1.134708076405642307, 0.7326428524546826360 ) ) ;
#18517 = CARTESIAN_POINT ( 'NONE',  ( 0.6054889487767985967, -1.479703267939684874, 0.5856070495615782745 ) ) ;
#18518 = CIRCLE ( 'NONE', #21141, 0.04999999999999885092 ) ;
#18519 = CARTESIAN_POINT ( 'NONE',  ( -0.1212602504510638252, -0.5073146174426025334, 0.3063129689661515664 ) ) ;
#18521 = ORIENTED_EDGE ( 'NONE', *, *, #8139, .T. ) ;
#18520 = ORIENTED_EDGE ( 'NONE', *, *, #1995, .F. ) ;
#18522 = CARTESIAN_POINT ( 'NONE',  ( 0.4778962374169136162, -1.100111666534134391, -0.4145951911632163034 ) ) ;
#18523 = DIRECTION ( 'NONE',  ( -0.4999551463232377313, 0.8660512985181132439, -0.000000000000000000 ) ) ;
#18524 = CARTESIAN_POINT ( 'NONE',  ( -0.02872242845530404223, -0.5252126300208065368, 0.08844866507292674374 ) ) ;
#18525 = CARTESIAN_POINT ( 'NONE',  ( 0.4402953823516241316, -1.206777924729731444, 0.8122253986942317150 ) ) ;
#18526 = CIRCLE ( 'NONE', #6027, 0.02999999999999994685 ) ;
#18527 = AXIS2_PLACEMENT_3D ( 'NONE', #11105, #4706, #5523 ) ;
#18528 = CARTESIAN_POINT ( 'NONE',  ( 0.2310769326552300218, -0.9374521120563168441, 0.6578705068509248521 ) ) ;
#18529 = CARTESIAN_POINT ( 'NONE',  ( -0.02953079040095687308, 0.3810518745593911571, 0.3687679460475725701 ) ) ;
#18530 = CIRCLE ( 'NONE', #29040, 0.06250000000000001388 ) ;
#18531 = CARTESIAN_POINT ( 'NONE',  ( -0.1138236225804901969, -0.5205343845807010039, 0.3387850541077452871 ) ) ;
#18532 = CARTESIAN_POINT ( 'NONE',  ( 0.4535584603515609992, -1.087313623170466759, -0.4112464619727521642 ) ) ;
#18533 = ADVANCED_FACE ( 'NONE', ( #13728 ), #23223, .T. ) ;
#18534 = DIRECTION ( 'NONE',  ( 0.000000000000000000, -0.1725921171157271672, 0.9849933812516259435 ) ) ;
#18535 = DIRECTION ( 'NONE',  ( -1.000000000000000000, -1.188678714063518030E-15, -1.779758311459931231E-16 ) ) ;
#18536 = CARTESIAN_POINT ( 'NONE',  ( 0.05999999999999990757, -0.1470479536050930680, -0.02961248622716588369 ) ) ;
#18537 =( NAMED_UNIT ( * ) SI_UNIT ( $, .STERADIAN. ) SOLID_ANGLE_UNIT ( ) );
#18538 = ADVANCED_FACE ( 'NONE', ( #3866 ), #1229, .F. ) ;
#18539 = CARTESIAN_POINT ( 'NONE',  ( 0.01548846960707340320, -0.2450655194479847421, 0.4674710490749314218 ) ) ;
#18540 = DIRECTION ( 'NONE',  ( 1.000000000000000000, 0.000000000000000000, 0.000000000000000000 ) ) ;
#18541 = EDGE_CURVE ( 'NONE', #27338, #38731, #39098, .T. ) ;
#18542 = CARTESIAN_POINT ( 'NONE',  ( 0.04583756681245852727, -1.039559191613112832, 0.7214566118523848548 ) ) ;
#18543 = CALENDAR_DATE ( 2026, 13, 10 ) ;
#18544 = CARTESIAN_POINT ( 'NONE',  ( 0.7203159877618242612, -1.479638488134456420, 0.5307775041526673343 ) ) ;
#18545 = ADVANCED_FACE ( 'NONE', ( #35955 ), #5407, .F. ) ;
#18546 = AXIS2_PLACEMENT_3D ( 'NONE', #4696, #20569, #26935 ) ;
#18547 = DIRECTION ( 'NONE',  ( -0.4999551463232377313, 0.8660512985181132439, -0.000000000000000000 ) ) ;
#18548 = CARTESIAN_POINT ( 'NONE',  ( -0.2399999999999999079, -4.233163482269810096, -0.5148221395285308422 ) ) ;
#18549 = CARTESIAN_POINT ( 'NONE',  ( 0.05561176441985739988, -0.2541700551350220549, 0.3845131534397776552 ) ) ;
#18550 = AXIS2_PLACEMENT_3D ( 'NONE', #4147, #7650, #16504 ) ;
#18551 = ADVANCED_FACE ( 'NONE', ( #17034 ), #7763, .T. ) ;
#18552 = ORIENTED_EDGE ( 'NONE', *, *, #6447, .T. ) ;
#18553 = CARTESIAN_POINT ( 'NONE',  ( 0.000000000000000000, -0.3165425539888620521, -0.4137570037148034507 ) ) ;
#18554 = VERTEX_POINT ( 'NONE', #10050 ) ;
#18555 = DIRECTION ( 'NONE',  ( -0.8660254037844392627, -0.2456612931291814739, -0.4354888391889020771 ) ) ;
#18556 = CARTESIAN_POINT ( 'NONE',  ( 0.2643552029519708468, -1.643455541575042700, 0.7762602543266098332 ) ) ;
#18557 = EDGE_CURVE ( 'NONE', #15927, #6967, #25909, .T. ) ;
#18558 = CIRCLE ( 'NONE', #21209, 0.06819284191469469902 ) ;
#18560 = ORIENTED_EDGE ( 'NONE', *, *, #10798, .T. ) ;
#18559 = CARTESIAN_POINT ( 'NONE',  ( 0.1428196694608256101, -0.6338724602092423721, 0.3861684053016066764 ) ) ;
#18562 = ORIENTED_EDGE ( 'NONE', *, *, #14287, .T. ) ;
#18561 = CARTESIAN_POINT ( 'NONE',  ( 0.03113248654051816583, 0.5878163732725504298, -0.1704268771689479434 ) ) ;
#18563 = EDGE_CURVE ( 'NONE', #10925, #4078, #6954, .T. ) ;
#18564 = CARTESIAN_POINT ( 'NONE',  ( 0.4444209036527600465, -1.039833579653637319, 0.7404771872114588316 ) ) ;
#18566 = VERTEX_POINT ( 'NONE', #4869 ) ;
#18565 = EDGE_LOOP ( 'NONE', ( #35117, #6649, #27061, #17945, #18502 ) ) ;
#18567 = CARTESIAN_POINT ( 'NONE',  ( 0.6660153594396612808, -1.377480952862383923, 0.7519195793979284170 ) ) ;
#18568 = CARTESIAN_POINT ( 'NONE',  ( 0.3601266045266868776, -1.712180511123387872, -0.5700849473641345089 ) ) ;
#18569 = CARTESIAN_POINT ( 'NONE',  ( 0.3186320389496528627, -1.760431904683431359, 0.5682417262808792113 ) ) ;
#18570 = DATE_AND_TIME ( #12592, #3733 ) ;
#18571 = DIRECTION ( 'NONE',  ( 0.000000000000000000, 0.000000000000000000, -1.000000000000000000 ) ) ;
#18572 = VERTEX_POINT ( 'NONE', #36751 ) ;
#18573 = CARTESIAN_POINT ( 'NONE',  ( 0.1924078334994414607, -0.8864580494542387834, 0.6093570016390645883 ) ) ;
#18574 = FACE_OUTER_BOUND ( 'NONE', #2124, .T. ) ;
#18575 = CARTESIAN_POINT ( 'NONE',  ( 0.1038860818051843410, -0.5481585384591742827, 0.1713426774629287497 ) ) ;
#18577 = CARTESIAN_POINT ( 'NONE',  ( -0.001987662015349134573, -0.8501386850767141956, 0.1022911480739698287 ) ) ;
#18576 = CARTESIAN_POINT ( 'NONE',  ( 0.3466922049894854974, -1.748660810794147258, 0.4514553480157271204 ) ) ;
#18578 = CARTESIAN_POINT ( 'NONE',  ( 0.03559495875357140959, -1.028803249407966858, 0.5691659535643065482 ) ) ;
#18579 = ORIENTED_EDGE ( 'NONE', *, *, #15038, .F. ) ;
#18580 = VECTOR ( 'NONE', #12560, 39.37007874015747433 ) ;
#18581 = CARTESIAN_POINT ( 'NONE',  ( 0.4468553387825724421, -1.686585475485919972, 0.5936113863420847681 ) ) ;
#18582 = CARTESIAN_POINT ( 'NONE',  ( 0.7431273937626133863, -1.516426637506990360, 0.5641520672112426693 ) ) ;
#18583 = MANIFOLD_SOLID_BREP ( 'Fillet15', #7616 ) ;
#18584 = CYLINDRICAL_SURFACE ( 'NONE', #23333, 0.03749999999977545601 ) ;
#18585 = AXIS2_PLACEMENT_3D ( 'NONE', #11525, #32901, #14195 ) ;
#18586 = AXIS2_PLACEMENT_3D ( 'NONE', #1568, #8111, #12377 ) ;
#18587 = CARTESIAN_POINT ( 'NONE',  ( 0.006100135935846554350, -0.8448938542399410112, 0.1277644845294366172 ) ) ;
#18588 = DIRECTION ( 'NONE',  ( -1.000000000000000000, -2.280301054154495132E-31, 1.664003471950577689E-31 ) ) ;
#18589 = AXIS2_PLACEMENT_3D ( 'NONE', #36265, #30111, #36486 ) ;
#18590 = EDGE_CURVE ( 'NONE', #17094, #21046, #36142, .T. ) ;
#18591 = CARTESIAN_POINT ( 'NONE',  ( 0.3925326341959034515, -1.148401673189667571, 0.4243628868813368316 ) ) ;
#18592 = CARTESIAN_POINT ( 'NONE',  ( 0.05999999999999990757, -0.03575622569115821658, -0.2978615321325044363 ) ) ;
#18593 = EDGE_CURVE ( 'NONE', #23137, #17453, #3463, .T. ) ;
#18594 = CARTESIAN_POINT ( 'NONE',  ( 0.3337689465763037377, -1.163262234248904736, 0.4559311481246714481 ) ) ;
#18595 = CARTESIAN_POINT ( 'NONE',  ( 0.2043709925794569282, -0.7174950807506157435, 0.3538749514786183048 ) ) ;
#18596 = SHAPE_DEFINITION_REPRESENTATION ( #622, #24383 ) ;
#18597 = CARTESIAN_POINT ( 'NONE',  ( 0.6672263256168233791, -1.559577713309469038, 0.6159734170043378310 ) ) ;
#18598 = AXIS2_PLACEMENT_3D ( 'NONE', #4549, #14022, #1716 ) ;
#18599 = CARTESIAN_POINT ( 'NONE',  ( 0.3583058169873264420, -1.905560598654033155, -0.4886429218441480371 ) ) ;
#18600 = DIRECTION ( 'NONE',  ( 2.157041537713701966E-32, -0.8709776783778060416, 0.4913225862583635584 ) ) ;
#18601 = CARTESIAN_POINT ( 'NONE',  ( -0.01899468245561315022, -0.07378005917298360861, 0.5147132347679528319 ) ) ;
#18602 = ORIENTED_EDGE ( 'NONE', *, *, #9267, .F. ) ;
#18603 = CARTESIAN_POINT ( 'NONE',  ( 0.4882304408116465155, -1.126680077128302093, 0.5092034011547009742 ) ) ;
#18604 = CARTESIAN_POINT ( 'NONE',  ( 0.4015936175283410514, -1.155705023113092533, 0.5182417262812423209 ) ) ;
#18605 = CIRCLE ( 'NONE', #11381, 0.1000000000000000194 ) ;
#18606 = DIRECTION ( 'NONE',  ( 1.000000000000000000, -0.000000000000000000, -0.000000000000000000 ) ) ;
#18607 = VERTEX_POINT ( 'NONE', #2013 ) ;
#18608 = CARTESIAN_POINT ( 'NONE',  ( -0.04285534776242663768, 0.07199417564834904859, -0.4895512033229227900 ) ) ;
#18609 = CARTESIAN_POINT ( 'NONE',  ( 0.07659735200988204706, -1.288566765071073261, 0.7428858345647274541 ) ) ;
#18611 = EDGE_LOOP ( 'NONE', ( #14394, #22362, #38735, #12286 ) ) ;
#18610 = VERTEX_POINT ( 'NONE', #17437 ) ;
#18612 = CARTESIAN_POINT ( 'NONE',  ( -0.06980746140711623082, -9.793929126999064681E-17, -0.2150000000000000244 ) ) ;
#18613 = CIRCLE ( 'NONE', #16650, 0.05000000000000000971 ) ;
#18614 = AXIS2_PLACEMENT_3D ( 'NONE', #14345, #20943, #24646 ) ;
#18615 = DIRECTION ( 'NONE',  ( -1.000000000000000000, -0.000000000000000000, -0.000000000000000000 ) ) ;
#18616 = CARTESIAN_POINT ( 'NONE',  ( 0.3638611582725052584, -1.770072597806926940, -0.3444173258735140908 ) ) ;
#18617 = CARTESIAN_POINT ( 'NONE',  ( -0.02000000000000000042, -2.183180860297908144, -0.4937760292030871079 ) ) ;
#18619 = DIRECTION ( 'NONE',  ( 0.9998941247116546194, -0.01455087607601020412, 0.0001066420868422379362 ) ) ;
#18618 = CARTESIAN_POINT ( 'NONE',  ( -0.1323926191616458248, 0.05688556330967550756, 0.02068925706491315727 ) ) ;
#18620 = CARTESIAN_POINT ( 'NONE',  ( 0.03647060353175575476, -0.2291014149038315684, -0.4576769917029361867 ) ) ;
#18621 = EDGE_LOOP ( 'NONE', ( #36941, #32517, #29448, #837 ) ) ;
#18622 = CARTESIAN_POINT ( 'NONE',  ( 0.07405132550584739293, -1.324440054897002561, 0.5176829506697802064 ) ) ;
#18623 = ORIENTED_EDGE ( 'NONE', *, *, #17977, .F. ) ;
#18624 = AXIS2_PLACEMENT_3D ( 'NONE', #21800, #15207, #21186 ) ;
#18625 = DIRECTION ( 'NONE',  ( -0.4999551463232377313, 0.8660512985181132439, 0.000000000000000000 ) ) ;
#18626 = CARTESIAN_POINT ( 'NONE',  ( 0.3727629667123311119, -1.357639913737091808, 0.8616512673511037557 ) ) ;
#18627 = CIRCLE ( 'NONE', #23898, 0.009999999999999995004 ) ;
#18629 = CARTESIAN_POINT ( 'NONE',  ( 0.5726702689957759995, -1.625473326825089160, 0.5525775856678601938 ) ) ;
#18628 = CARTESIAN_POINT ( 'NONE',  ( -0.05562144613422575351, -0.4316454521248627718, 0.1615915407302010720 ) ) ;
#18630 = DIRECTION ( 'NONE',  ( -1.000000000000000000, -2.403560570595279103E-31, 1.725633230170969455E-31 ) ) ;
#18631 = CARTESIAN_POINT ( 'NONE',  ( 0.1509261766453387776, -1.286374238887308064, -0.3063610351341911620 ) ) ;
#18632 = UNCERTAINTY_MEASURE_WITH_UNIT (LENGTH_MEASURE( 1.000000000000000082E-05 ), #324, 'distance_accuracy_value', 'NONE');
#18633 = CARTESIAN_POINT ( 'NONE',  ( 0.3999999999999784284, -2.047156491238096621, -0.7141923294504529673 ) ) ;
#18634 = CARTESIAN_POINT ( 'NONE',  ( 0.1940479051238430952, -1.673580430301878641, -0.3295078277357051388 ) ) ;
#18635 = CARTESIAN_POINT ( 'NONE',  ( 0.5809530576852517392, -1.495264608998207789, 0.5740006802652367623 ) ) ;
#18636 = CARTESIAN_POINT ( 'NONE',  ( 0.4746182331242696506, -1.678388708763134396, 0.4747050670221392710 ) ) ;
#18637 = DIRECTION ( 'NONE',  ( 0.000000000000000000, 0.000000000000000000, -1.000000000000000000 ) ) ;
#18638 = CARTESIAN_POINT ( 'NONE',  ( -0.02869942827333594668, 0.4519168387192263325, 0.2102852866807454479 ) ) ;
#18639 = CARTESIAN_POINT ( 'NONE',  ( 0.2260995971937757310, -1.236443303375862390, 0.5209257643876351596 ) ) ;
#18640 = AXIS2_PLACEMENT_3D ( 'NONE', #17030, #10645, #3863 ) ;
#18641 = CARTESIAN_POINT ( 'NONE',  ( 0.4441836334028865796, -1.145505455753590418, -0.6481113851292223949 ) ) ;
#18642 = CARTESIAN_POINT ( 'NONE',  ( 0.1934691495297424235, -1.255374174182389391, 0.4342266066129076285 ) ) ;
#18643 = CARTESIAN_POINT ( 'NONE',  ( 0.2073655362268157221, -0.5791461380176760043, 0.4026997059449013427 ) ) ;
#18644 = VECTOR ( 'NONE', #33955, 39.37007874015747433 ) ;
#18645 = CARTESIAN_POINT ( 'NONE',  ( -0.04211471441534125892, 0.2686849334112402787, 0.3844466239331203461 ) ) ;
#18646 = CARTESIAN_POINT ( 'NONE',  ( 0.02926306740268063214, -1.136388740552946031, 0.6581294774663873914 ) ) ;
#18647 = CARTESIAN_POINT ( 'NONE',  ( 0.6398031614116831411, -1.462875994906407850, -0.3971521418811111981 ) ) ;
#18648 = CARTESIAN_POINT ( 'NONE',  ( 0.000000000000000000, 0.6304109427692223822, -0.1442409525262416947 ) ) ;
#18649 = CARTESIAN_POINT ( 'NONE',  ( -0.02000000000000000042, -1.490119023906541607, -0.04361282830843733055 ) ) ;
#18650 = CARTESIAN_POINT ( 'NONE',  ( 0.2650653946250867143, -1.676094176783521128, 0.5635705756526244725 ) ) ;
#18651 = CIRCLE ( 'NONE', #30488, 0.5756329413417605734 ) ;
#18652 = DIRECTION ( 'NONE',  ( 0.000000000000000000, 0.000000000000000000, 1.000000000000000000 ) ) ;
#18653 = AXIS2_PLACEMENT_3D ( 'NONE', #1720, #1312, #13819 ) ;
#18654 = ORIENTED_EDGE ( 'NONE', *, *, #6230, .T. ) ;
#18655 = DIRECTION ( 'NONE',  ( 1.000000000000000000, 2.276539994720212446E-15, 0.000000000000000000 ) ) ;
#18656 = CARTESIAN_POINT ( 'NONE',  ( 0.3808107057333847134, -1.740972190922900120, -0.5768324160695250669 ) ) ;
#18657 = CARTESIAN_POINT ( 'NONE',  ( 0.6652220256568632806, -1.517545837045118473, 0.4231643303188328820 ) ) ;
#18658 = DIRECTION ( 'NONE',  ( -2.465190328815661892E-32, -1.000000000000000000, -6.656013887802287108E-31 ) ) ;
#18659 = DIRECTION ( 'NONE',  ( -1.000000000000000000, -2.341930812374887555E-31, 1.664003471950578127E-31 ) ) ;
#18660 = PERSON ( 'NAUO-PER12', 'UNSPECIFIED', 'UNSPECIFIED', ('UNSPECIFIED'), ('UNSPECIFIED'), ('UNSPECIFIED') ) ;
#18661 = ORIENTED_EDGE ( 'NONE', *, *, #1259, .F. ) ;
#18662 = CARTESIAN_POINT ( 'NONE',  ( 0.5467981811930778813, -1.652054351292815637, -0.5405695263049933308 ) ) ;
#18663 = CARTESIAN_POINT ( 'NONE',  ( 0.3390201860129213318, -1.162303158162408812, 0.6024826139476634479 ) ) ;
#18664 = CARTESIAN_POINT ( 'NONE',  ( 0.05999999999999990757, 0.3931478764542372661, 0.2416960844521746365 ) ) ;
#18665 = CARTESIAN_POINT ( 'NONE',  ( -2.070754768975509030, -0.09959325338431655739, 0.09550516381870291505 ) ) ;
#18666 = CARTESIAN_POINT ( 'NONE',  ( 0.3350890287386661948, -1.062171315605431321, 0.7337690394249966053 ) ) ;
#18667 = ORIENTED_EDGE ( 'NONE', *, *, #18331, .T. ) ;
#18668 = CARTESIAN_POINT ( 'NONE',  ( 0.4216623502531439693, -1.034931331451964143, 0.6525378447207771382 ) ) ;
#18669 = EDGE_LOOP ( 'NONE', ( #10470, #20590, #6566, #27381 ) ) ;
#18670 = PERSON_AND_ORGANIZATION ( #28500, #32463 ) ;
#18671 = ORIENTED_EDGE ( 'NONE', *, *, #33175, .T. ) ;
#18672 = AXIS2_PLACEMENT_3D ( 'NONE', #5036, #17392, #20697 ) ;
#18673 = ORIENTED_EDGE ( 'NONE', *, *, #260, .T. ) ;
#18674 = VECTOR ( 'NONE', #4620, 39.37007874015748143 ) ;
#18675 = CARTESIAN_POINT ( 'NONE',  ( 0.2931371671966536696, -1.364037168738611250, 0.8947199202213534930 ) ) ;
#18677 = CARTESIAN_POINT ( 'NONE',  ( 0.1748881817888952583, -0.8846221646991694332, 0.02718377953341061248 ) ) ;
#18676 = DIRECTION ( 'NONE',  ( 0.000000000000000000, -3.330669073875470114E-16, -1.000000000000000000 ) ) ;
#18678 = DIRECTION ( 'NONE',  ( 0.000000000000000000, 0.7055763269171819729, 0.7086339301035887717 ) ) ;
#18679 = EDGE_LOOP ( 'NONE', ( #9447, #33244, #13193, #39305, #13000, #12496, #18279, #37278 ) ) ;
#18680 = ORIENTED_EDGE ( 'NONE', *, *, #23002, .T. ) ;
#18681 = EDGE_LOOP ( 'NONE', ( #34793, #22369, #6517, #2019 ) ) ;
#18682 = ORIENTED_EDGE ( 'NONE', *, *, #492, .T. ) ;
#18683 = CARTESIAN_POINT ( 'NONE',  ( 0.3669132811502856528, -0.9575263150705904946, 0.6684360246000486949 ) ) ;
#18684 = CARTESIAN_POINT ( 'NONE',  ( 0.3813006723851273816, -1.191008781084291313, 0.8308973255029469263 ) ) ;
#18685 = ORIENTED_EDGE ( 'NONE', *, *, #29485, .F. ) ;
#18686 = CARTESIAN_POINT ( 'NONE',  ( 0.2298507129413651373, -1.629337845148150166, -0.3572920125246931145 ) ) ;
#18687 = DIRECTION ( 'NONE',  ( 1.000000000000000000, 6.779273404243070203E-32, 4.314083075427408311E-32 ) ) ;
#18688 = CIRCLE ( 'NONE', #322, 0.009999999999999995004 ) ;
#18689 = DIRECTION ( 'NONE',  ( -0.000000000000000000, 0.7071067811865465735, 0.7071067811865484609 ) ) ;
#18690 = CARTESIAN_POINT ( 'NONE',  ( 0.4200748011392089198, -1.654004974025707897, -0.2869361388274795921 ) ) ;
#18691 = CARTESIAN_POINT ( 'NONE',  ( -0.2600000000000004530, 0.5182417262804744906, 0.08500000000000017264 ) ) ;
#18692 = CARTESIAN_POINT ( 'NONE',  ( 0.4092750486073892247, -1.698390055749431138, 0.4182417262808776903 ) ) ;
#18693 = DIRECTION ( 'NONE',  ( -0.000000000000000000, 0.9396926207859082059, 0.3420201433256691570 ) ) ;
#18694 = ORIENTED_EDGE ( 'NONE', *, *, #7246, .T. ) ;
#18695 = ADVANCED_FACE ( 'NONE', ( #1825 ), #14540, .T. ) ;
#18696 = CARTESIAN_POINT ( 'NONE',  ( 0.08052762188558729162, -1.822603993077213103, -0.6442490663871589529 ) ) ;
#18697 = CARTESIAN_POINT ( 'NONE',  ( 0.1399999999999994582, 0.000000000000000000, 0.000000000000000000 ) ) ;
#18698 = CALENDAR_DATE ( 2026, 13, 10 ) ;
#18699 = APPLIED_PERSON_AND_ORGANIZATION_ASSIGNMENT ( #20421, #7849, ( #39117 ) ) ;
#18700 = CIRCLE ( 'NONE', #1661, 0.08749999999977552123 ) ;
#18701 = CARTESIAN_POINT ( 'NONE',  ( 0.4892015816964360719, -1.080660821007120020, 0.5933591780025184725 ) ) ;
#18702 = AXIS2_PLACEMENT_3D ( 'NONE', #37159, #24825, #18021 ) ;
#18703 = CARTESIAN_POINT ( 'NONE',  ( 0.4427163477200127262, -1.139245542564126357, 0.4379379976781114792 ) ) ;
#18704 = CARTESIAN_POINT ( 'NONE',  ( 0.06518445159565730562, -1.341084469003575030, 0.5526808653810328931 ) ) ;
#18705 = CARTESIAN_POINT ( 'NONE',  ( -0.01548846960707524721, 0.3880410510314791783, 0.3755318131854940567 ) ) ;
#18706 = AXIS2_PLACEMENT_3D ( 'NONE', #40463, #8780, #18250 ) ;
#18707 = AXIS2_PLACEMENT_3D ( 'NONE', #24111, #2291, #36635 ) ;
#18708 = APPLIED_APPROVAL_ASSIGNMENT ( #15957, ( #1177 ) ) ;
#18709 = CARTESIAN_POINT ( 'NONE',  ( -0.002023118427450016753, -0.8974731051190899533, 0.1948784381876195460 ) ) ;
#18710 = CARTESIAN_POINT ( 'NONE',  ( 0.2709623010280027278, -1.672610760848568967, 0.4891849873696615392 ) ) ;
#18711 = CARTESIAN_POINT ( 'NONE',  ( 0.1880670007137922317, -1.959169693390261591, -0.6952383742845916759 ) ) ;
#18712 = CARTESIAN_POINT ( 'NONE',  ( 0.2011892967074958294, -1.251141541415955905, -0.3144976166544465324 ) ) ;
#18713 = AXIS2_PLACEMENT_3D ( 'NONE', #13813, #16719, #38302 ) ;
#18714 = EDGE_LOOP ( 'NONE', ( #6465, #40569, #13787, #22690 ) ) ;
#18715 = ORIENTED_EDGE ( 'NONE', *, *, #24992, .F. ) ;
#18716 = DIRECTION ( 'NONE',  ( -1.000000000000000000, -6.779273404243070203E-32, -4.314083075427408311E-32 ) ) ;
#18717 = ORIENTED_EDGE ( 'NONE', *, *, #11426, .T. ) ;
#18718 = CARTESIAN_POINT ( 'NONE',  ( 0.2667797934877766397, -1.675028870926974500, 0.5053016059147321659 ) ) ;
#18719 = B_SPLINE_CURVE_WITH_KNOTS ( 'NONE', 3,
 ( #27793, #20613, #24120, #4954, #8446, #17519, #18124, #33749, #21439, #1898, #20823, #14411, #26973, #27188, #24303, #5770, #33147, #23908, #39721, #30871, #36436, #8250, #11944 ),
 .UNSPECIFIED., .F., .F.,
 ( 4, 2, 2, 2, 2, 2, 2, 2, 1, 2, 2, 4 ),
 ( 0.000000000000000000, 0.001303949395765936943, 0.001955924093648904981, 0.002607898791531872585, 0.003911848187297809962, 0.005215797583063746905, 0.006519746978829682980, 0.007171721676712655355, 0.007823696374595628597, 0.008475671072478601839, 0.009127645770361575081, 0.01043159516612753024 ),
 .UNSPECIFIED. ) ;
#18720 = DIRECTION ( 'NONE',  ( 0.8660512985181134660, 0.4999551463232373427, 0.000000000000000000 ) ) ;
#18721 = CARTESIAN_POINT ( 'NONE',  ( 0.4256811042841359138, -1.183992690650692348, 0.8157300287015782914 ) ) ;
#18723 = ORIENTED_EDGE ( 'NONE', *, *, #8471, .F. ) ;
#18722 = CARTESIAN_POINT ( 'NONE',  ( 0.01050449021347792111, -0.5294792378225862128, 0.1383083324213474075 ) ) ;
#18724 = EDGE_LOOP ( 'NONE', ( #29688, #10511, #6316 ) ) ;
#18725 = CARTESIAN_POINT ( 'NONE',  ( -0.08000000000000000167, -1.737515812098395118, -0.8661170628529262228 ) ) ;
#18726 = EDGE_CURVE ( 'NONE', #858, #23391, #5722, .T. ) ;
#18727 = ORIENTED_EDGE ( 'NONE', *, *, #687, .F. ) ;
#18728 = CARTESIAN_POINT ( 'NONE',  ( 0.01091791702278631891, -0.5391733969928702574, 0.2078372220302295847 ) ) ;
#18730 = CARTESIAN_POINT ( 'NONE',  ( 0.09670933914072363247, -1.286966393572076761, 0.5906442777704791203 ) ) ;
#18729 = CARTESIAN_POINT ( 'NONE',  ( 0.1606430264876529124, -0.9001996987827759478, 0.5837366715005726236 ) ) ;
#18731 = CARTESIAN_POINT ( 'NONE',  ( 0.01207335092558379890, -0.4550518931080567708, 0.03096792667458423548 ) ) ;
#18732 = DATE_TIME_ROLE ( 'classification_date' ) ;
#18733 = CIRCLE ( 'NONE', #1032, 0.4615209409081865166 ) ;
#18734 = EDGE_CURVE ( 'NONE', #24067, #37440, #13966, .T. ) ;
#18735 = ADVANCED_FACE ( 'NONE', ( #39436 ), #39637, .T. ) ;
#18736 = CARTESIAN_POINT ( 'NONE',  ( 0.1984950629327257021, -1.252696871964387393, -0.5155029497116575543 ) ) ;
#18738 = EDGE_LOOP ( 'NONE', ( #16061, #14447, #11610, #798 ) ) ;
#18737 = EDGE_LOOP ( 'NONE', ( #31349, #6815, #36024, #6360, #11599 ) ) ;
#18739 = AXIS2_PLACEMENT_3D ( 'NONE', #37101, #24174, #39566 ) ;
#18740 = EDGE_CURVE ( 'NONE', #17780, #8227, #25342, .T. ) ;
#18741 = CARTESIAN_POINT ( 'NONE',  ( 0.4688459138424371786, -1.061988423737608045, -0.4248180574663140141 ) ) ;
#18742 = CYLINDRICAL_SURFACE ( 'NONE', #17538, 0.6115209409081865388 ) ;
#18743 = CARTESIAN_POINT ( 'NONE',  ( -0.05281452789367811762, -0.4315450824722529832, 0.1820506770215943593 ) ) ;
#18744 = CIRCLE ( 'NONE', #26620, 1.986674066779348102 ) ;
#18745 = CARTESIAN_POINT ( 'NONE',  ( 0.5371247828146922254, -1.393663287660293237, 0.7819316079650096007 ) ) ;
#18746 = CARTESIAN_POINT ( 'NONE',  ( 0.1270245264032780486, -0.8251090115851287266, 0.2117204377992136233 ) ) ;
#18747 = APPLIED_SECURITY_CLASSIFICATION_ASSIGNMENT ( #26657, ( #36468 ) ) ;
#18748 = FACE_OUTER_BOUND ( 'NONE', #13578, .T. ) ;
#18749 = CARTESIAN_POINT ( 'NONE',  ( 0.06481568609301656403, -0.7456345099580035107, 0.7576189738271701390 ) ) ;
#18750 = APPLICATION_CONTEXT ( 'configuration controlled 3d designs of mechanical parts and assemblies' ) ;
#18751 = CONICAL_SURFACE ( 'NONE', #2308, 0.03999999999999933470, 1.047197551196598742 ) ;
#18752 = CARTESIAN_POINT ( 'NONE',  ( -0.2746410161513776482, -4.162452804151155483, -0.5855328176471856771 ) ) ;
#18753 = LINE ( 'NONE', #10309, #27244 ) ;
#18754 =( BOUNDED_SURFACE ( )  B_SPLINE_SURFACE ( 3, 2, ( 
 ( #12356, #24912, #37438 ),
 ( #22438, #34149, #31074 ),
 ( #25106, #12972, #34966 ),
 ( #22244, #9865, #16059 ) ),
 .UNSPECIFIED., .F., .F., .F. ) 
 B_SPLINE_SURFACE_WITH_KNOTS ( ( 4, 4 ),
 ( 3, 3 ),
 ( -3.123586458930738274E-16, 0.0004255989732716984912 ),
 ( 0.000000000000000000, 1.000000000000000000 ),
 .UNSPECIFIED. ) 
 GEOMETRIC_REPRESENTATION_ITEM ( )  RATIONAL_B_SPLINE_SURFACE ( (
 ( 1.000000000000000000, 0.8997265729122759792, 1.000000000000000000),
 ( 1.000000000000000000, 0.8954993961798249913, 1.000000000000000000),
 ( 1.000000000000000000, 0.8844303544522131855, 1.000000000000000000),
 ( 1.000000000000000000, 0.8624897507815776354, 1.000000000000000000) ) ) 
 REPRESENTATION_ITEM ( '' )  SURFACE ( )  );
#18755 = CARTESIAN_POINT ( 'NONE',  ( 0.4667937283406220494, -1.235624442469605899, 0.6184277979272206904 ) ) ;
#18756 = ADVANCED_FACE ( 'NONE', ( #14957, #36566, #26904, #8562, #39850 ), #24227, .T. ) ;
#18757 = LINE ( 'NONE', #24732, #24047 ) ;
#18758 = LENGTH_MEASURE_WITH_UNIT ( LENGTH_MEASURE( 0.02539999999999999897 ), #25340 );
#18759 = APPLIED_PERSON_AND_ORGANIZATION_ASSIGNMENT ( #24471, #24273, ( #27114 ) ) ;
#18760 = CARTESIAN_POINT ( 'NONE',  ( 0.03875523708677636181, -0.2524014508497919862, 0.4040490413287874394 ) ) ;
#18761 = DIRECTION ( 'NONE',  ( 0.000000000000000000, 0.5877852522924655876, -0.8090169943749527803 ) ) ;
#18762 = CARTESIAN_POINT ( 'NONE',  ( 0.07209178019044594488, -1.135423765654719919, 0.7590189199326136116 ) ) ;
#18763 = PERSON_AND_ORGANIZATION_ROLE ( 'creator' ) ;
#18764 = CARTESIAN_POINT ( 'NONE',  ( 0.2791332027808016703, -0.7342173681784933681, 0.6310308052199803397 ) ) ;
#18765 = CARTESIAN_POINT ( 'NONE',  ( -0.03303737228521335528, 0.4610015631984548667, 0.2426019986921462146 ) ) ;
#18766 = CIRCLE ( 'NONE', #4941, 0.06000000000000031697 ) ;
#18767 = CARTESIAN_POINT ( 'NONE',  ( 0.6889662060151644507, -1.555147259246191016, 0.5968497998442635621 ) ) ;
#18768 = EDGE_CURVE ( 'NONE', #1496, #14919, #21910, .T. ) ;
#18769 = DIRECTION ( 'NONE',  ( 0.000000000000000000, 0.000000000000000000, -1.000000000000000000 ) ) ;
#18770 = CARTESIAN_POINT ( 'NONE',  ( 0.3850572304970821258, -1.658899166394309788, -0.4146413147361216467 ) ) ;
#18771 = EDGE_LOOP ( 'NONE', ( #13830, #33867, #1251, #2369 ) ) ;
#18772 = CARTESIAN_POINT ( 'NONE',  ( -0.02000000000000000042, -1.851224977018630868, -0.7958870385335592434 ) ) ;
#18773 = LOCAL_TIME ( 0, 53, 7.000000000000000000, #37795 ) ;
#18774 = CARTESIAN_POINT ( 'NONE',  ( 0.1882598819837821291, -1.364719520154515475, 0.9410996297614753203 ) ) ;
#18775 = CARTESIAN_POINT ( 'NONE',  ( 0.4749671191778466750, -1.308524979286208367, 0.8177814803665567345 ) ) ;
#18777 = ORIENTED_EDGE ( 'NONE', *, *, #14239, .T. ) ;
#18776 = CARTESIAN_POINT ( 'NONE',  ( 0.000000000000000000, 0.1919340784543128453, -0.1767348310837237868 ) ) ;
#18778 = CIRCLE ( 'NONE', #31264, 0.01499999999999996302 ) ;
#18779 = CARTESIAN_POINT ( 'NONE',  ( 0.1874999999999996669, -0.6872203660140441261, 0.1527381444932270627 ) ) ;
#18781 = ORIENTED_EDGE ( 'NONE', *, *, #6808, .F. ) ;
#18780 = EDGE_LOOP ( 'NONE', ( #7209, #41, #39698, #35231 ) ) ;
#18782 = CARTESIAN_POINT ( 'NONE',  ( 0.3956566811268355521, -0.9596954108736347466, 0.7461004073261953140 ) ) ;
#18783 = EDGE_CURVE ( 'NONE', #17036, #33948, #19931, .T. ) ;
#18784 = CARTESIAN_POINT ( 'NONE',  ( 0.05561176441985765662, 0.4316390549698252421, -0.1616802657107470620 ) ) ;
#18785 = CARTESIAN_POINT ( 'NONE',  ( 0.3186755585808466740, -1.760356642135124439, 0.5625658558758077632 ) ) ;
#18786 = CALENDAR_DATE ( 2026, 13, 10 ) ;
#18787 = EDGE_CURVE ( 'NONE', #8811, #17499, #8615, .T. ) ;
#18788 = FACE_OUTER_BOUND ( 'NONE', #13042, .T. ) ;
#18789 = VERTEX_POINT ( 'NONE', #3412 ) ;
#18790 = EDGE_CURVE ( 'NONE', #14, #32680, #16004, .T. ) ;
#18791 = CARTESIAN_POINT ( 'NONE',  ( 0.08837989099891704892, -0.7491984653599970123, 0.2305845840354824039 ) ) ;
#18792 = CARTESIAN_POINT ( 'NONE',  ( 0.3150771742308554058, -1.733448878803460991, 0.7884676298878301459 ) ) ;
#18793 = CARTESIAN_POINT ( 'NONE',  ( 0.5262589651392098888, -1.523534812712205477, 0.6368633379848268605 ) ) ;
#18794 = DIRECTION ( 'NONE',  ( -1.000000000000000000, -0.000000000000000000, -0.000000000000000000 ) ) ;
#18795 = CARTESIAN_POINT ( 'NONE',  ( -0.05562144613422690537, -0.2542273817772361388, 0.3844451335760749600 ) ) ;
#18796 = ORIENTED_EDGE ( 'NONE', *, *, #1707, .T. ) ;
#18797 = DIRECTION ( 'NONE',  ( 1.000000000000000000, 0.000000000000000000, 0.000000000000000000 ) ) ;
#18798 = B_SPLINE_CURVE_WITH_KNOTS ( 'NONE', 3,
 ( #2194, #34055, #5854, #18413, #1991, #11448, #24015, #33443, #5251, #3801, #13259, #28892, #16170, #753, #6876, #25829 ),
 .UNSPECIFIED., .F., .F.,
 ( 4, 2, 2, 2, 2, 2, 2, 4 ),
 ( 0.002977951493358533663, 0.003350111319365782318, 0.003722271145373030974, 0.004094430971380279630, 0.004466590797387528719, 0.004838750623394776941, 0.005210910449402025163, 0.005955230101416519005 ),
 .UNSPECIFIED. ) ;
#18799 = VECTOR ( 'NONE', #38388, 39.37007874015748143 ) ;
#18800 = CARTESIAN_POINT ( 'NONE',  ( 0.6660103463786463118, -1.561565158697419742, 0.5710166038345764195 ) ) ;
#18801 = AXIS2_PLACEMENT_3D ( 'NONE', #38755, #27042, #1169 ) ;
#18802 = LINE ( 'NONE', #28063, #35815 ) ;
#18803 = EDGE_CURVE ( 'NONE', #3165, #839, #16618, .T. ) ;
#18804 = CARTESIAN_POINT ( 'NONE',  ( -0.1572280491643790745, 0.4879031095700105403, 0.3568535915792940827 ) ) ;
#18805 = EDGE_CURVE ( 'NONE', #23204, #30458, #23215, .T. ) ;
#18806 = LOCAL_TIME ( 0, 53, 7.000000000000000000, #7307 ) ;
#18807 =( NAMED_UNIT ( * ) SI_UNIT ( $, .STERADIAN. ) SOLID_ANGLE_UNIT ( ) );
#18808 = EDGE_CURVE ( 'NONE', #3414, #29923, #27142, .T. ) ;
#18809 = DIRECTION ( 'NONE',  ( 1.000000000000000000, -0.000000000000000000, -0.000000000000000000 ) ) ;
#18810 = EDGE_CURVE ( 'NONE', #3047, #31843, #31068, .T. ) ;
#18811 = CARTESIAN_POINT ( 'NONE',  ( 0.2644881156243384379, -1.676263310743548063, 0.5220153280337084256 ) ) ;
#18812 = AXIS2_PLACEMENT_3D ( 'NONE', #6892, #10201, #22769 ) ;
#18813 = CARTESIAN_POINT ( 'NONE',  ( 0.06824055730039223222, -1.289945330482348496, 0.6789996349980699231 ) ) ;
#18814 = CARTESIAN_POINT ( 'NONE',  ( 0.5549275037195743332, -1.190966985655177890, 0.5563916622750778584 ) ) ;
#18815 = APPROVAL_DATE_TIME ( #21288, #39090 ) ;
#18816 = ADVANCED_FACE ( 'NONE', ( #9378 ), #9593, .T. ) ;
#18817 = CARTESIAN_POINT ( 'NONE',  ( 0.06980746140711582837, 0.000000000000000000, 0.000000000000000000 ) ) ;
#18818 = CARTESIAN_POINT ( 'NONE',  ( 0.6077657638426647857, -1.479710398481848266, 0.5717087807361217466 ) ) ;
#18819 = CARTESIAN_POINT ( 'NONE',  ( -0.05634115714581361400, -0.005221855766565763196, 0.4588864551388208701 ) ) ;
#18820 = ORIENTED_EDGE ( 'NONE', *, *, #6749, .T. ) ;
#18821 = CARTESIAN_POINT ( 'NONE',  ( 0.1876053338355621880, -0.6785855078148245179, 0.1477569985384105666 ) ) ;
#18822 = DIRECTION ( 'NONE',  ( 0.8849907732522489523, 0.000000000000000000, 0.4656085601214676739 ) ) ;
#18823 = CARTESIAN_POINT ( 'NONE',  ( 0.08572064877627985635, -0.7939468086886716236, 0.08347532546618800786 ) ) ;
#18824 = ORIENTED_EDGE ( 'NONE', *, *, #7634, .F. ) ;
#18825 = AXIS2_PLACEMENT_3D ( 'NONE', #26713, #23012, #11065 ) ;
#18826 = CARTESIAN_POINT ( 'NONE',  ( -0.02881329448201249560, -0.06013561456248174564, -0.4945523155237964708 ) ) ;
#18827 = CIRCLE ( 'NONE', #1120, 0.04330708661417340122 ) ;
#18828 = CARTESIAN_POINT ( 'NONE',  ( -0.006649224014923847334, -0.8922124784979929002, 0.4965188763020696450 ) ) ;
#18830 = ORIENTED_EDGE ( 'NONE', *, *, #30543, .F. ) ;
#18829 = ORIENTED_EDGE ( 'NONE', *, *, #9032, .T. ) ;
#18831 = CARTESIAN_POINT ( 'NONE',  ( 0.4159916692016358830, -1.069406866067976081, -0.5155029497116575543 ) ) ;
#18832 = DIRECTION ( 'NONE',  ( 1.000000000000000000, 6.779273404243070203E-32, 4.314083075427408311E-32 ) ) ;
#18833 = LOCAL_TIME ( 0, 53, 7.000000000000000000, #7029 ) ;
#18834 = CARTESIAN_POINT ( 'NONE',  ( 0.3579523269453451229, -1.819438262761551073, -0.3432675831194216820 ) ) ;
#18835 = EDGE_CURVE ( 'NONE', #40111, #30976, #4264, .T. ) ;
#18837 = CARTESIAN_POINT ( 'NONE',  ( 0.3088664963667261398, -1.757905065063135597, 0.5295467280985148850 ) ) ;
#18836 = CARTESIAN_POINT ( 'NONE',  ( 0.01896968469601798685, 0.4667670904252309572, 0.2292592343991468606 ) ) ;
#18838 = B_SPLINE_CURVE_WITH_KNOTS ( 'NONE', 3,
 ( #12409, #24960, #37490, #9311, #6234, #16320 ),
 .UNSPECIFIED., .F., .F.,
 ( 4, 2, 4 ),
 ( 0.000000000000000000, 0.5000000000000000000, 1.000000000000000000 ),
 .UNSPECIFIED. ) ;
#18839 = CARTESIAN_POINT ( 'NONE',  ( 0.04308611741967822983, -0.2425947520953637970, -0.4306844107907368269 ) ) ;
#18840 = ORIENTED_EDGE ( 'NONE', *, *, #2886, .T. ) ;
#18841 = EDGE_CURVE ( 'NONE', #7253, #13057, #13327, .T. ) ;
#18842 = AXIS2_PLACEMENT_3D ( 'NONE', #18817, #37114, #27862 ) ;
#18843 = CARTESIAN_POINT ( 'NONE',  ( 0.09535664604372214026, -0.5879077161293799758, 0.2928325945560249499 ) ) ;
#18844 = ORIENTED_EDGE ( 'NONE', *, *, #3500, .T. ) ;
#18845 = CARTESIAN_POINT ( 'NONE',  ( 0.7043850983579452718, -1.516419193711280311, 0.5648052198873427798 ) ) ;
#18846 = CARTESIAN_POINT ( 'NONE',  ( 0.07323308598001919412, -0.5520613865617218785, 0.2133277464804944623 ) ) ;
#18848 = FACE_OUTER_BOUND ( 'NONE', #2337, .T. ) ;
#18847 = CARTESIAN_POINT ( 'NONE',  ( -0.04582713223189537749, -0.4790191777205499157, 0.08746099429787616841 ) ) ;
#18849 = CARTESIAN_POINT ( 'NONE',  ( -0.05464101615137786222, -2.122347498858831116, -0.8313396097929491857 ) ) ;
#18850 = CARTESIAN_POINT ( 'NONE',  ( 0.2049605114958119589, -0.9388532809880968388, 0.4165185827052858003 ) ) ;
#18851 = CARTESIAN_POINT ( 'NONE',  ( 0.7237670104885922662, -1.526800250143491189, -0.6194292131661300882 ) ) ;
#18852 = CARTESIAN_POINT ( 'NONE',  ( 0.1887412855916273946, -0.4595320686313617564, 0.1458683203705864184 ) ) ;
#18853 = CARTESIAN_POINT ( 'NONE',  ( 0.5808478773694798480, -1.495250919194240691, 0.5721815422400771123 ) ) ;
#18854 = CARTESIAN_POINT ( 'NONE',  ( -0.04293317454820686635, 0.3457449726441636506, 0.3536934093827128756 ) ) ;
#18855 = CARTESIAN_POINT ( 'NONE',  ( -0.01548846960707524721, 0.000000000000000000, 0.000000000000000000 ) ) ;
#18856 = DIRECTION ( 'NONE',  ( 2.526820087036053001E-31, 0.1402348365095093807, -0.9901182710308659152 ) ) ;
#18857 = CARTESIAN_POINT ( 'NONE',  ( 0.07216878364870311924, 0.000000000000000000, 0.1249999999999999029 ) ) ;
#18858 = DIRECTION ( 'NONE',  ( 0.4999551463232372872, -0.8660512985181134660, 0.000000000000000000 ) ) ;
#18859 = VECTOR ( 'NONE', #17776, 39.37007874015748143 ) ;
#18860 = EDGE_CURVE ( 'NONE', #13663, #38278, #9788, .T. ) ;
#18861 = CARTESIAN_POINT ( 'NONE',  ( 0.6807551469422991053, -1.407487954066357183, 0.5751647024762112093 ) ) ;
#18862 = EDGE_CURVE ( 'NONE', #27951, #13401, #17022, .T. ) ;
#18863 = CARTESIAN_POINT ( 'NONE',  ( -0.03301200226531702392, 0.3732424419978498942, 0.3635087277994350496 ) ) ;
#18864 = CARTESIAN_POINT ( 'NONE',  ( 0.01746090273258609979, -1.060756659779402034, 0.6072269701260313290 ) ) ;
#18865 = CARTESIAN_POINT ( 'NONE',  ( -0.05464101615137769569, -2.179113517810423062, -0.3318097452986852880 ) ) ;
#18866 = MANIFOLD_SOLID_BREP ( 'Chamfer1', #19442 ) ;
#18867 = CARTESIAN_POINT ( 'NONE',  ( 0.3999999999999787059, -2.097675824466503691, -0.4688691127277797022 ) ) ;
#18868 = CARTESIAN_POINT ( 'NONE',  ( -0.1603938765018536328, 0.4636889572247743230, 0.1178658435936996290 ) ) ;
#18869 = CARTESIAN_POINT ( 'NONE',  ( 0.05999999999999990757, -0.03575622569115821658, -0.1978615321325044307 ) ) ;
#18870 = CARTESIAN_POINT ( 'NONE',  ( 0.6358155198048017764, -1.579893599062534459, 0.4258446345833196700 ) ) ;
#18871 = EDGE_LOOP ( 'NONE', ( #7783, #18349, #32165 ) ) ;
#18872 = DIRECTION ( 'NONE',  ( 4.930380657631316120E-32, -0.4685245517976818208, -0.8834504764630450868 ) ) ;
#18873 = CARTESIAN_POINT ( 'NONE',  ( 0.4072427871757727247, -1.593905482146963148, -0.4124169901356457557 ) ) ;
#18874 = CARTESIAN_POINT ( 'NONE',  ( 0.3641226214008350115, -1.992333883506425929, -0.5205058662226371702 ) ) ;
#18875 = DIRECTION ( 'NONE',  ( 0.000000000000000000, 0.5365213554527478168, -0.8438867430782083234 ) ) ;
#18876 = CARTESIAN_POINT ( 'NONE',  ( 0.3686268575871315401, -2.054613415874774862, -0.4779605220224154571 ) ) ;
#18877 = B_SPLINE_CURVE_WITH_KNOTS ( 'NONE', 3,
 ( #38346, #363, #34665, #6469, #12867, #9768, #22338, #19243, #31786, #38148, #16168, #28705, #9971, #569, #10181, #29095, #961, #26037, #4402, #7478, #38961, #36078, #1159, #29704, #35675, #32587, #7878, #11187, #14462, #36269, #1344, #1762, #1550, #23362, #13851, #20450, #4583, #14274, #23747, #32984, #8091, #26838, #26424, #7695, #13659, #14071, #20668, #17155, #26224, #16763, #10791, #38746, #11002, #39177 ),
 .UNSPECIFIED., .F., .F.,
 ( 4, 2, 2, 2, 2, 2, 2, 2, 2, 2, 2, 2, 2, 2, 2, 2, 2, 2, 2, 2, 2, 2, 2, 2, 2, 2, 4 ),
 ( 0.000000000000000000, 0.001467739507578043421, 0.002935479015156086842, 0.005870958030312173684, 0.01174191606062434216, 0.01467739507578042814, 0.01761287409093651238, 0.02054835310609260182, 0.02201609261367064654, 0.02348383212124869474, 0.02641931113640478071, 0.02935479015156086668, 0.03082252965913890794, 0.03229026916671694919, 0.03375800867429499391, 0.03522574818187304557, 0.03669348768945108336, 0.03742735744324009184, 0.03816122719702910726, 0.03962896670460712423, 0.04109670621218514119, 0.04256444571976315816, 0.04403218522734117513, 0.04549992473491919209, 0.04623379448870819364, 0.04660072936560270829, 0.04696766424249720906 ),
 .UNSPECIFIED. ) ;
#18878 = B_SPLINE_CURVE_WITH_KNOTS ( 'NONE', 3,
 ( #40543, #15244, #18531, #40336, #12165, #24728, #15653, #28617 ),
 .UNSPECIFIED., .F., .F.,
 ( 4, 2, 2, 4 ),
 ( -9.185902906383436317E-17, 0.0008552058350302804311, 0.001282808752545464394, 0.001710411670060648683 ),
 .UNSPECIFIED. ) ;
#18879 = EDGE_LOOP ( 'NONE', ( #16819, #5497, #18602, #37392 ) ) ;
#18880 = CARTESIAN_POINT ( 'NONE',  ( 0.5198360076875652158, -1.665829548412769201, -0.5914331627923441470 ) ) ;
#18881 = CARTESIAN_POINT ( 'NONE',  ( 0.1871937864180454048, -1.374138184793721518, 0.5181962843648889594 ) ) ;
#18882 = DIRECTION ( 'NONE',  ( -0.9876771640241659433, -0.1565050148243856687, -1.024672052421402957E-13 ) ) ;
#18883 = CARTESIAN_POINT ( 'NONE',  ( 0.01896931156527556159, 0.3622781579086356563, -0.3730773604463906157 ) ) ;
#18884 = CARTESIAN_POINT ( 'NONE',  ( 0.4704808408627720873, -1.246563891206539099, 0.7003883943243975896 ) ) ;
#18885 = EDGE_CURVE ( 'NONE', #36373, #17309, #38275, .T. ) ;
#18887 = ORIENTED_EDGE ( 'NONE', *, *, #7947, .T. ) ;
#18886 = CARTESIAN_POINT ( 'NONE',  ( -0.01548846960707490547, 0.09061086148575973886, 0.5171215251571029681 ) ) ;
#18888 = CARTESIAN_POINT ( 'NONE',  ( 0.4892015816964360719, -1.080660821007120020, 0.5933591780025184725 ) ) ;
#18889 = ORIENTED_EDGE ( 'NONE', *, *, #40222, .T. ) ;
#18890 = CALENDAR_DATE ( 2026, 13, 10 ) ;
#18891 = CARTESIAN_POINT ( 'NONE',  ( 0.02352711120663245753, -0.9586990007338236364, 0.6297157671916142618 ) ) ;
#18892 = ORIENTED_EDGE ( 'NONE', *, *, #22153, .F. ) ;
#18893 = CARTESIAN_POINT ( 'NONE',  ( 0.3851754998513399753, -1.605598480965388708, 0.5732781203792557401 ) ) ;
#18895 = CARTESIAN_POINT ( 'NONE',  ( 0.1755999888594793890, -0.7630904603782766582, -0.07194964429679771845 ) ) ;
#18894 = CARTESIAN_POINT ( 'NONE',  ( 0.06469648274370130847, -0.8304785510687793249, 0.1072521381146411823 ) ) ;
#18896 = CARTESIAN_POINT ( 'NONE',  ( 0.06694067462889406739, -0.6776034894424159960, -0.001903836934785778628 ) ) ;
#18897 = ORIENTED_EDGE ( 'NONE', *, *, #3504, .F. ) ;
#18898 = ORIENTED_EDGE ( 'NONE', *, *, #29100, .F. ) ;
#18899 = EDGE_LOOP ( 'NONE', ( #17369, #28787, #24162, #31063, #28550 ) ) ;
#18900 = ORIENTED_EDGE ( 'NONE', *, *, #27504, .T. ) ;
#18901 = DIRECTION ( 'NONE',  ( 1.000000000000000000, -0.000000000000000000, -0.000000000000000000 ) ) ;
#18902 = CARTESIAN_POINT ( 'NONE',  ( 0.5195437916533927059, -1.430322578995237182, 0.7780002750953179946 ) ) ;
#18903 = ORIENTED_EDGE ( 'NONE', *, *, #37637, .T. ) ;
#18904 = CARTESIAN_POINT ( 'NONE',  ( 0.1873341288634420843, -0.6980686425579779586, 0.03222456286304159478 ) ) ;
#18905 = CARTESIAN_POINT ( 'NONE',  ( 0.1475835875794125895, -1.275005690054430874, -0.3395826425993545561 ) ) ;
#18906 = FACE_BOUND ( 'NONE', #33572, .T. ) ;
#18907 = CARTESIAN_POINT ( 'NONE',  ( -2.128333683970191216E-14, -2.097675824466503691, -0.2907100122647986451 ) ) ;
#18908 = CARTESIAN_POINT ( 'NONE',  ( 0.2999999999999791167, -2.097675824466505023, -0.2588528740066098344 ) ) ;
#18909 = DIRECTION ( 'NONE',  ( 0.000000000000000000, 0.000000000000000000, 1.000000000000000000 ) ) ;
#18910 = LINE ( 'NONE', #18292, #21887 ) ;
#18911 = DIRECTION ( 'NONE',  ( -1.000000000000000000, -2.280301054154495132E-31, 1.664003471950577689E-31 ) ) ;
#18912 = CARTESIAN_POINT ( 'NONE',  ( 0.1782772739027001230, -1.243608455402465340, 0.6125714912171157378 ) ) ;
#18913 = CARTESIAN_POINT ( 'NONE',  ( 0.09553074791598278881, -1.668408090489538864, -0.6432190139176878763 ) ) ;
#18914 = CARTESIAN_POINT ( 'NONE',  ( 0.5971614065082352374, -1.461417804984935342, 0.6057417262805111502 ) ) ;
#18915 = DATE_AND_TIME ( #3259, #15417 ) ;
#18916 = ADVANCED_FACE ( 'NONE', ( #9994 ), #5432, .T. ) ;
#18917 = CARTESIAN_POINT ( 'NONE',  ( 0.1877336102437491272, -0.9152557094465934018, 0.1737200839639440053 ) ) ;
#18918 = CARTESIAN_POINT ( 'NONE',  ( 0.3257277097560854484, -1.167896984018933493, 0.4676436393436195216 ) ) ;
#18919 = CARTESIAN_POINT ( 'NONE',  ( 0.4409357815299598804, -1.228106680636185111, 0.6057417262809895453 ) ) ;
#18921 = ORIENTED_EDGE ( 'NONE', *, *, #8343, .T. ) ;
#18920 = DIRECTION ( 'NONE',  ( 1.000000000000000000, 0.000000000000000000, 0.000000000000000000 ) ) ;
#18922 = CARTESIAN_POINT ( 'NONE',  ( 0.1362517741244128056, -1.308408735431443093, 0.8505046261270597929 ) ) ;
#18923 = CARTESIAN_POINT ( 'NONE',  ( 0.5860224930377164743, -1.538459444162366019, -0.4143855572951781197 ) ) ;
#18924 = CARTESIAN_POINT ( 'NONE',  ( 0.1846519493495785980, -1.936915843690041994, -0.6921256737722615293 ) ) ;
#18925 = CARTESIAN_POINT ( 'NONE',  ( 0.3302717389963351624, -1.638372317322708716, 0.4882842553274441277 ) ) ;
#18926 = CONICAL_SURFACE ( 'NONE', #11022, 0.03999999999999964001, 1.047197551196596299 ) ;
#18927 = ORIENTED_EDGE ( 'NONE', *, *, #39615, .F. ) ;
#18928 = ORIENTED_EDGE ( 'NONE', *, *, #4363, .F. ) ;
#18929 = DIRECTION ( 'NONE',  ( 0.4999999999999956701, 0.7066258520834639567, 0.5006794435238205443 ) ) ;
#18930 = ORIENTED_EDGE ( 'NONE', *, *, #25580, .F. ) ;
#18931 = FACE_OUTER_BOUND ( 'NONE', #39585, .T. ) ;
#18932 = CARTESIAN_POINT ( 'NONE',  ( -0.05283710938261064471, -0.4560492058803821691, -0.1064717188025600669 ) ) ;
#18933 = CARTESIAN_POINT ( 'NONE',  ( 0.4150272135712330113, -1.167431181930913553, 0.8149900857543223021 ) ) ;
#18935 = ORIENTED_EDGE ( 'NONE', *, *, #29588, .F. ) ;
#18934 = CARTESIAN_POINT ( 'NONE',  ( 0.01548846960707524721, 0.2372406987223678043, 0.4850946823762586901 ) ) ;
#18936 = ORIENTED_EDGE ( 'NONE', *, *, #3117, .T. ) ;
#18937 = DIRECTION ( 'NONE',  ( 0.8660254037844402619, 0.2957393706636063380, 0.4031602964572422731 ) ) ;
#18938 = ORIENTED_EDGE ( 'NONE', *, *, #5102, .T. ) ;
#18939 = CARTESIAN_POINT ( 'NONE',  ( 0.2966820077695481173, -1.656469531661595163, 0.5666191999804250923 ) ) ;
#18941 = CARTESIAN_POINT ( 'NONE',  ( 0.1245238869884406352, -1.284104819735092606, 0.6026496813689052878 ) ) ;
#18940 = CARTESIAN_POINT ( 'NONE',  ( 0.2437792440929114346, -0.9773701458837178446, 0.6962579099302033114 ) ) ;
#18942 = DIRECTION ( 'NONE',  ( 0.000000000000000000, 0.8090169943749455639, -0.5877852522924756906 ) ) ;
#18943 = CARTESIAN_POINT ( 'NONE',  ( 0.01182080120375270972, -0.6039130564843261384, -0.09998022549266330494 ) ) ;
#18944 = CARTESIAN_POINT ( 'NONE',  ( 0.3699999999999786793, -2.183180860297921466, -0.4937760292030871079 ) ) ;
#18946 = ORIENTED_EDGE ( 'NONE', *, *, #37295, .T. ) ;
#18945 = ORIENTED_EDGE ( 'NONE', *, *, #36099, .T. ) ;
#18947 = CARTESIAN_POINT ( 'NONE',  ( 0.4667255516235201407, -1.094999438749613585, -0.3992978201560059559 ) ) ;
#18948 = FACE_OUTER_BOUND ( 'NONE', #38324, .T. ) ;
#18949 = CARTESIAN_POINT ( 'NONE',  ( -0.04308449196698675016, -0.4845747790795000287, 0.09763455429601199109 ) ) ;
#18950 = CYLINDRICAL_SURFACE ( 'NONE', #31889, 0.09249999999977555343 ) ;
#18951 = DIRECTION ( 'NONE',  ( -0.000000000000000000, 0.8090169943749540016, 0.5877852522924639223 ) ) ;
#18952 = CARTESIAN_POINT ( 'NONE',  ( -0.2399999999999999079, -3.849534981189179028, -0.1910928155360645808 ) ) ;
#18953 = CARTESIAN_POINT ( 'NONE',  ( 0.01954262108197177966, -0.5199582741543401498, 0.4378456291139402046 ) ) ;
#18954 = AXIS2_PLACEMENT_3D ( 'NONE', #38347, #26225, #19838 ) ;
#18955 = DIRECTION ( 'NONE',  ( -1.000000000000000000, -7.857794173099924470E-32, -8.628166150854818811E-32 ) ) ;
#18956 = DIRECTION ( 'NONE',  ( 1.702140497302372314E-12, -0.5877852522924748024, -0.8090169943749461190 ) ) ;
#18957 = DIRECTION ( 'NONE',  ( 0.8660512985181133550, 0.4999551463232372872, -1.835254611910146959E-15 ) ) ;
#18958 = SHAPE_REPRESENTATION_RELATIONSHIP ( 'NONE' , 'NONE' ,  #7794, #14212 ) ;
#18959 = DIRECTION ( 'NONE',  ( 0.4999551463232372317, -0.8660512985181135770, 0.000000000000000000 ) ) ;
#18960 = CARTESIAN_POINT ( 'NONE',  ( 0.05109603825399443300, -0.7331182637548316894, 0.7465514741729609716 ) ) ;
#18961 = CARTESIAN_POINT ( 'NONE',  ( 0.07257591959104818524, -1.183556761366722387, 0.7640614581424595153 ) ) ;
#18962 = EDGE_CURVE ( 'NONE', #26219, #28034, #18991, .T. ) ;
#18963 = APPROVAL_STATUS ( 'not_yet_approved' ) ;
#18964 = EDGE_CURVE ( 'NONE', #16904, #24117, #16574, .T. ) ;
#18965 = CARTESIAN_POINT ( 'NONE',  ( -0.05634402396114354672, 0.4396062797411981471, 0.1319984305213857956 ) ) ;
#18966 = CARTESIAN_POINT ( 'NONE',  ( 0.7050067303326591484, -1.529446169236064135, 0.5714306314579442603 ) ) ;
#18967 = EDGE_CURVE ( 'NONE', #25362, #19095, #28728, .T. ) ;
#18968 = FACE_OUTER_BOUND ( 'NONE', #29358, .T. ) ;
#18969 = ORIENTED_EDGE ( 'NONE', *, *, #5663, .T. ) ;
#18970 = CARTESIAN_POINT ( 'NONE',  ( 0.4488015593626361044, -1.143595277755407036, -0.6412565985276246217 ) ) ;
#18971 = CARTESIAN_POINT ( 'NONE',  ( 0.2742629518370554575, -1.653361553673516227, 0.7386680983805660183 ) ) ;
#18972 = CARTESIAN_POINT ( 'NONE',  ( 0.4015825763966658912, -1.182054300648716083, 0.8205428547305109177 ) ) ;
#18974 = ORIENTED_EDGE ( 'NONE', *, *, #20091, .F. ) ;
#18973 = CARTESIAN_POINT ( 'NONE',  ( 0.3460651993684921712, -1.167700608961039332, 0.4299100439411554508 ) ) ;
#18976 = VERTEX_POINT ( 'NONE', #4011 ) ;
#18975 = VERTEX_POINT ( 'NONE', #19660 ) ;
#18977 = DIRECTION ( 'NONE',  ( -0.4999551463232369541, 0.8660512985181135770, 0.000000000000000000 ) ) ;
#18978 = CARTESIAN_POINT ( 'NONE',  ( 0.3393113466938358358, -1.652445952795071227, -0.5834520628848905988 ) ) ;
#18979 = ADVANCED_FACE ( 'NONE', ( #10814 ), #29771, .T. ) ;
#18980 = APPLIED_PERSON_AND_ORGANIZATION_ASSIGNMENT ( #37607, #229, ( #19398 ) ) ;
#18981 = LINE ( 'NONE', #15888, #15409 ) ;
#18982 = SECURITY_CLASSIFICATION_LEVEL ( 'unclassified' ) ;
#18983 = DIRECTION ( 'NONE',  ( 0.000000000000000000, 0.000000000000000000, -1.000000000000000000 ) ) ;
#18984 = ORIENTED_EDGE ( 'NONE', *, *, #4969, .F. ) ;
#18985 = CARTESIAN_POINT ( 'NONE',  ( 0.2010125963195148191, -0.8858709603250995990, 0.6259238706880295711 ) ) ;
#18986 = CARTESIAN_POINT ( 'NONE',  ( 0.3978748429313913038, -1.632648866504059049, -0.3859154407376138018 ) ) ;
#18987 = CARTESIAN_POINT ( 'NONE',  ( 0.1039182570229498503, -0.5495296521639349008, 0.1804408898608185485 ) ) ;
#18988 = CARTESIAN_POINT ( 'NONE',  ( 0.5759858430877791147, -1.611702281530391856, -0.5409994141166248882 ) ) ;
#18989 = CARTESIAN_POINT ( 'NONE',  ( -0.1617555154933773554, 0.4683069300263263957, 0.1178658435716314345 ) ) ;
#18990 = VERTEX_POINT ( 'NONE', #1362 ) ;
#18991 = B_SPLINE_CURVE_WITH_KNOTS ( 'NONE', 3,
 ( #35094, #22776, #29118, #13494, #38765, #10209, #28910, #7286, #32196, #29335, #23169, #22961, #7502, #6898, #32398, #29522, #19863, #7091 ),
 .UNSPECIFIED., .F., .F.,
 ( 4, 2, 2, 2, 2, 2, 2, 2, 4 ),
 ( 0.0003425652276237299478, 0.001007165397454245050, 0.001671765567284760152, 0.002336365737115275037, 0.003000965906945790573, 0.003665566076776305242, 0.004330166246606820778, 0.004994766416437335446, 0.005659366586267850982 ),
 .UNSPECIFIED. ) ;
#18992 = CARTESIAN_POINT ( 'NONE',  ( 0.2923286432308245808, -1.660243258845594649, -0.6250000000000000000 ) ) ;
#18993 = CARTESIAN_POINT ( 'NONE',  ( 0.7430585616337137544, -1.516428101037593512, 0.5626827419390632024 ) ) ;
#18994 = B_SPLINE_CURVE_WITH_KNOTS ( 'NONE', 3,
 ( #38383, #7103, #7299, #19671, #34695, #28737, #15986, #32207, #19281, #19072, #4022, #15772, #28531, #16588, #34893, #6706, #12685, #13093 ),
 .UNSPECIFIED., .F., .F.,
 ( 4, 2, 2, 2, 2, 2, 2, 2, 4 ),
 ( 0.000000000000000000, 0.0005104183120475769102, 0.001020836624095153820, 0.001531254936142730731, 0.002041673248190307641, 0.002552091560237884551, 0.003062509872285461461, 0.003572928184333038371, 0.004083346496380615281 ),
 .UNSPECIFIED. ) ;
#18995 = ADVANCED_FACE ( 'NONE', ( #32610 ), #36304, .F. ) ;
#18996 = LINE ( 'NONE', #31528, #27290 ) ;
#18997 = CARTESIAN_POINT ( 'NONE',  ( 0.1460988943316244848, -0.6240739943263109435, 0.3647668637918258239 ) ) ;
#18998 = CARTESIAN_POINT ( 'NONE',  ( -0.1625122179509649878, 0.5048329626761703937, 0.3461446680885723604 ) ) ;
#18999 = B_SPLINE_CURVE_WITH_KNOTS ( 'NONE', 3,
 ( #22975, #13694, #600, #13094, #25652, #39213 ),
 .UNSPECIFIED., .F., .F.,
 ( 4, 2, 4 ),
 ( 0.000000000000000000, 0.0006234106414633451380, 0.001246821282926690276 ),
 .UNSPECIFIED. ) ;
#19000 = LENGTH_MEASURE_WITH_UNIT ( LENGTH_MEASURE( 0.02539999999999999897 ), #3561 );
#19001 = DIRECTION ( 'NONE',  ( 1.000000000000000000, 0.000000000000000000, 8.537024980200792236E-16 ) ) ;
#19002 = CARTESIAN_POINT ( 'NONE',  ( 0.2640998637001502058, -1.676998255898582091, 0.4887480333912877506 ) ) ;
#19003 = AXIS2_PLACEMENT_3D ( 'NONE', #8305, #26839, #27030 ) ;
#19004 = CARTESIAN_POINT ( 'NONE',  ( 0.06399702207960011879, -1.267566535398010563, 0.6886354586937382116 ) ) ;
#19005 = CARTESIAN_POINT ( 'NONE',  ( 0.2706875035899702353, -0.8747201880513900685, 0.5443116846754595395 ) ) ;
#19006 = EDGE_CURVE ( 'NONE', #13940, #17702, #40027, .T. ) ;
#19007 = DATE_TIME_ROLE ( 'classification_date' ) ;
#19008 = CYLINDRICAL_SURFACE ( 'NONE', #13580, 0.03000000000000022787 ) ;
#19009 = EDGE_CURVE ( 'NONE', #39975, #3578, #5030, .T. ) ;
#19010 = CARTESIAN_POINT ( 'NONE',  ( -0.2746410161513776482, -3.812085038045152974, -0.02801711824816590160 ) ) ;
#19011 = ADVANCED_FACE ( 'NONE', ( #39387 ), #36515, .T. ) ;
#19012 = CARTESIAN_POINT ( 'NONE',  ( -0.05544444631433745330, 0.02030017825816688229, 0.4608552147122319531 ) ) ;
#19013 = ORIENTED_EDGE ( 'NONE', *, *, #18810, .F. ) ;
#19014 = CARTESIAN_POINT ( 'NONE',  ( -0.08411373178446428234, 0.05688556330967591002, -0.1043107429350862841 ) ) ;
#19015 = DIRECTION ( 'NONE',  ( 5.551115123125400598E-17, 3.263080277421932464E-16, -1.000000000000000000 ) ) ;
#19016 = CARTESIAN_POINT ( 'NONE',  ( 0.08862505653733224187, -0.6119536582126900992, 0.04826979502260971000 ) ) ;
#19017 = ORIENTED_EDGE ( 'NONE', *, *, #15422, .T. ) ;
#19018 = CARTESIAN_POINT ( 'NONE',  ( 0.2320755761173002307, -1.232873731908348480, 0.4177417262808779674 ) ) ;
#19019 = CARTESIAN_POINT ( 'NONE',  ( 0.03746391227491855519, -1.107308778534258131, 0.7549414212349836450 ) ) ;
#19021 = VERTEX_POINT ( 'NONE', #23776 ) ;
#19020 = VERTEX_POINT ( 'NONE', #31103 ) ;
#19022 = DIRECTION ( 'NONE',  ( 1.000000000000000000, 0.000000000000000000, 0.000000000000000000 ) ) ;
#19023 = ORIENTED_EDGE ( 'NONE', *, *, #12452, .T. ) ;
#19024 = FACE_OUTER_BOUND ( 'NONE', #23897, .T. ) ;
#19025 = ADVANCED_FACE ( 'NONE', ( #29945 ), #26858, .T. ) ;
#19026 = CARTESIAN_POINT ( 'NONE',  ( 0.2578922072143235433, -1.569585936607025944, -0.3484340070010775170 ) ) ;
#19028 = FACE_OUTER_BOUND ( 'NONE', #22757, .T. ) ;
#19027 = DIRECTION ( 'NONE',  ( 1.000000000000000000, 0.000000000000000000, 0.000000000000000000 ) ) ;
#19029 = CARTESIAN_POINT ( 'NONE',  ( 0.05078310099560445767, -0.2374900923169175615, -0.4099167927582010873 ) ) ;
#19030 = EDGE_LOOP ( 'NONE', ( #17903, #8482, #4713, #17744 ) ) ;
#19031 = LINE ( 'NONE', #36588, #26404 ) ;
#19032 = ORIENTED_EDGE ( 'NONE', *, *, #38499, .F. ) ;
#19033 = CARTESIAN_POINT ( 'NONE',  ( 0.09184176262540320879, -0.6123617702671079188, 0.2291278788234172303 ) ) ;
#19034 = ORIENTED_EDGE ( 'NONE', *, *, #38663, .T. ) ;
#19035 = ORIENTED_EDGE ( 'NONE', *, *, #21741, .F. ) ;
#19036 = CARTESIAN_POINT ( 'NONE',  ( -0.05464101615137795936, -1.712002775963388235, -0.1631032362481502906 ) ) ;
#19037 = CARTESIAN_POINT ( 'NONE',  ( 0.1528396677094553124, -0.8424192790127347230, 0.6801078269868232606 ) ) ;
#19039 = DIRECTION ( 'NONE',  ( -1.000000000000000000, -2.276539994720197063E-15, 0.000000000000000000 ) ) ;
#19038 = CARTESIAN_POINT ( 'NONE',  ( 0.5065174388604494204, -1.605197562044919701, -0.4068557283993430862 ) ) ;
#19040 = CARTESIAN_POINT ( 'NONE',  ( 0.1399999999999994582, 0.000000000000000000, 0.000000000000000000 ) ) ;
#19041 = CARTESIAN_POINT ( 'NONE',  ( 0.1723742836622136898, -0.9181944984900098916, 0.1915515737749588221 ) ) ;
#19042 = UNCERTAINTY_MEASURE_WITH_UNIT (LENGTH_MEASURE( 1.000000000000000082E-05 ), #12411, 'distance_accuracy_value', 'NONE');
#19043 = FACE_OUTER_BOUND ( 'NONE', #16164, .T. ) ;
#19044 = CARTESIAN_POINT ( 'NONE',  ( 0.1887412855915411858, -0.4595320686313046910, 0.1385946963835863743 ) ) ;
#19045 = CARTESIAN_POINT ( 'NONE',  ( 0.1269878671055759134, -0.5786664369199111535, 0.2632502270387737653 ) ) ;
#19046 = CARTESIAN_POINT ( 'NONE',  ( -0.03174036153404918847, 0.3664551212196169860, -0.3753291932915809315 ) ) ;
#19047 = FACE_BOUND ( 'NONE', #27227, .T. ) ;
#19048 = CARTESIAN_POINT ( 'NONE',  ( -0.2399999999999999079, -2.853330612949663170, -0.6088139570729240724 ) ) ;
#19049 = CARTESIAN_POINT ( 'NONE',  ( 0.06924657687967017416, -0.5400045886221176428, 0.1476626190087814705 ) ) ;
#19050 = FACE_OUTER_BOUND ( 'NONE', #21989, .T. ) ;
#19051 = CARTESIAN_POINT ( 'NONE',  ( 0.4107733320947055122, -0.9780847931859447675, 0.7674390821536307694 ) ) ;
#19052 = ADVANCED_FACE ( 'NONE', ( #2165 ), #39200, .T. ) ;
#19053 = CARTESIAN_POINT ( 'NONE',  ( 0.4570320186965683984, -1.145281013718252305, 0.4021993759966799864 ) ) ;
#19054 = CARTESIAN_POINT ( 'NONE',  ( 0.03430157769017382757, -1.168583015135568504, 0.6655574557517952572 ) ) ;
#19055 = EDGE_CURVE ( 'NONE', #9108, #28184, #6767, .T. ) ;
#19056 = CARTESIAN_POINT ( 'NONE',  ( 0.6089144417693378442, -1.582852168051670505, -0.4632939045166076242 ) ) ;
#19057 = MANIFOLD_SOLID_BREP ( 'Fillet2', #14854 ) ;
#19058 = CARTESIAN_POINT ( 'NONE',  ( 0.3996070378906176890, -2.075685236164255265, -0.4730688532139160629 ) ) ;
#19059 = CARTESIAN_POINT ( 'NONE',  ( 0.1887090023420391338, -0.9018070888474317703, 0.5958977073701414717 ) ) ;
#19060 = CARTESIAN_POINT ( 'NONE',  ( 0.02869942827333533952, 0.2420058122830180403, -0.4357544236535293991 ) ) ;
#19061 = DIRECTION ( 'NONE',  ( -9.042510699458645841E-13, 1.566396143878659165E-12, -1.000000000000000000 ) ) ;
#19062 = VECTOR ( 'NONE', #26911, 39.37007874015748143 ) ;
#19063 = EDGE_LOOP ( 'NONE', ( #27625, #4627, #36478, #20197 ) ) ;
#19064 = EDGE_CURVE ( 'NONE', #33803, #7743, #11361, .T. ) ;
#19065 = DIRECTION ( 'NONE',  ( 5.264498737790503632E-15, -0.8834504764630464191, 0.4685245517976792673 ) ) ;
#19066 = CARTESIAN_POINT ( 'NONE',  ( 0.1499999999999994948, -0.4730347584886754331, 0.2341461249029889169 ) ) ;
#19067 = CARTESIAN_POINT ( 'NONE',  ( 0.6578511400472081272, -1.468260077009814202, 0.4182417262808778013 ) ) ;
#19068 = CARTESIAN_POINT ( 'NONE',  ( 0.1734973056165642902, -1.209394307038482497, -0.5155029497116575543 ) ) ;
#19069 = ORIENTED_EDGE ( 'NONE', *, *, #32113, .T. ) ;
#19070 = CARTESIAN_POINT ( 'NONE',  ( 0.4072455522228593527, -1.612170731801505941, -0.6686547157232122229 ) ) ;
#19071 = DIRECTION ( 'NONE',  ( -1.000000000000000000, -0.000000000000000000, -0.000000000000000000 ) ) ;
#19072 = CARTESIAN_POINT ( 'NONE',  ( 0.4824891092964968542, -1.662412547341785896, 0.4835662331627371135 ) ) ;
#19073 = EDGE_CURVE ( 'NONE', #20917, #17096, #30717, .T. ) ;
#19074 = CARTESIAN_POINT ( 'NONE',  ( 0.05634206451479451677, 0.2613530514269510330, -0.3773282889206430180 ) ) ;
#19075 = CARTESIAN_POINT ( 'NONE',  ( 0.3489069294160111467, -1.081181803243002504, 0.7355034317277300282 ) ) ;
#19077 = DIRECTION ( 'NONE',  ( 1.000000000000000000, 1.445897915516965072E-15, -8.881784197001242463E-16 ) ) ;
#19076 = DIRECTION ( 'NONE',  ( 0.4999551463232373427, -0.8660512985181134660, 0.000000000000000000 ) ) ;
#19078 = CARTESIAN_POINT ( 'NONE',  ( 0.4851165728318759252, -1.078419517084477697, 0.6030839855583299824 ) ) ;
#19079 = ORIENTED_EDGE ( 'NONE', *, *, #26296, .T. ) ;
#19080 = EDGE_CURVE ( 'NONE', #11876, #20992, #1548, .T. ) ;
#19081 = PERSON_AND_ORGANIZATION ( #28500, #32463 ) ;
#19082 = CARTESIAN_POINT ( 'NONE',  ( 0.04035408590310328447, -1.027233222095623510, 0.7038666329257657894 ) ) ;
#19083 = ORIENTED_EDGE ( 'NONE', *, *, #35356, .F. ) ;
#19084 = VERTEX_POINT ( 'NONE', #7713 ) ;
#19085 = CARTESIAN_POINT ( 'NONE',  ( 0.3863278360478267781, -1.605740116755117075, 0.5905161093819162321 ) ) ;
#19087 = CARTESIAN_POINT ( 'NONE',  ( 0.1859259531917270003, -0.7321509755579215240, -0.01543098434727066537 ) ) ;
#19086 = DIRECTION ( 'NONE',  ( 1.000000000000000000, 1.138269997360109379E-15, 0.000000000000000000 ) ) ;
#19088 = CARTESIAN_POINT ( 'NONE',  ( 0.06795783451517332929, -0.5973041244007833983, 0.02846421222436375589 ) ) ;
#19089 = ORIENTED_EDGE ( 'NONE', *, *, #8172, .T. ) ;
#19090 = AXIS2_PLACEMENT_3D ( 'NONE', #34085, #36970, #40472 ) ;
#19091 = EDGE_LOOP ( 'NONE', ( #5998, #19170, #25974, #239, #13028, #13366, #4245, #21871, #35052, #9921 ) ) ;
#19092 = ORIENTED_EDGE ( 'NONE', *, *, #5434, .T. ) ;
#19093 = CARTESIAN_POINT ( 'NONE',  ( -0.1142670043590670176, -0.4723146173917492918, 0.1178658435936998927 ) ) ;
#19094 = CARTESIAN_POINT ( 'NONE',  ( 0.5670196490188851302, -1.503246592690220540, 0.5746465183166465929 ) ) ;
#19095 = VERTEX_POINT ( 'NONE', #23985 ) ;
#19096 = CARTESIAN_POINT ( 'NONE',  ( 0.1874000730451391150, -0.6935093423028750870, 0.03601873687098033211 ) ) ;
#19097 = SPHERICAL_SURFACE ( 'NONE', #37076, 0.01499999999999999944 ) ;
#19098 = DIRECTION ( 'NONE',  ( 0.000000000000000000, -2.986499936241660365E-14, 1.000000000000000000 ) ) ;
#19099 = CIRCLE ( 'NONE', #29599, 0.01500000000000005669 ) ;
#19100 = DIRECTION ( 'NONE',  ( -1.000000000000000000, -0.000000000000000000, -0.000000000000000000 ) ) ;
#19101 = LINE ( 'NONE', #10249, #34363 ) ;
#19102 = FACE_OUTER_BOUND ( 'NONE', #57, .T. ) ;
#19103 = DIRECTION ( 'NONE',  ( 1.000000000000000000, 2.325617669281439721E-12, 1.136734431350428609E-12 ) ) ;
#19104 = B_SPLINE_CURVE_WITH_KNOTS ( 'NONE', 3,
 ( #3112, #22451, #12987, #25731 ),
 .UNSPECIFIED., .F., .F.,
 ( 4, 4 ),
 ( 0.000000000000000000, 0.0003323657284514935093 ),
 .UNSPECIFIED. ) ;
#19105 = CARTESIAN_POINT ( 'NONE',  ( 0.4191100986681119411, -1.701672718972377929, 0.4233639548768234895 ) ) ;
#19106 = CYLINDRICAL_SURFACE ( 'NONE', #2920, 0.2500000000000000000 ) ;
#19107 = CARTESIAN_POINT ( 'NONE',  ( 0.07945738019374083694, -1.321132034926529419, 0.5723852862170456524 ) ) ;
#19108 = CARTESIAN_POINT ( 'NONE',  ( 0.1591109521009923256, -1.922302435482596383, -0.6593845993814091422 ) ) ;
#19109 = CARTESIAN_POINT ( 'NONE',  ( 0.08214737558356681457, -1.311413488239922431, 0.7308976325429462628 ) ) ;
#19110 = APPROVAL_ROLE ( '' ) ;
#19111 = EDGE_CURVE ( 'NONE', #38965, #26127, #8326, .T. ) ;
#19112 = CARTESIAN_POINT ( 'NONE',  ( 0.1885390680155161480, -0.9156976364345736918, 0.1977769869421455440 ) ) ;
#19113 = DIRECTION ( 'NONE',  ( -1.416619696839553052E-11, -0.9510565162951529761, 0.3090169943749491166 ) ) ;
#19114 = EDGE_CURVE ( 'NONE', #34037, #34358, #23862, .T. ) ;
#19115 = CARTESIAN_POINT ( 'NONE',  ( 0.4857742178082134488, -1.202222293638773420, 0.6057417262810468328 ) ) ;
#19116 = CARTESIAN_POINT ( 'NONE',  ( 0.2615177342056695942, -1.679396441256837846, 0.5426384715137531067 ) ) ;
#19117 = CARTESIAN_POINT ( 'NONE',  ( 0.1230419690069037980, -1.441173760443279050, 0.5802947806848592904 ) ) ;
#19118 = CARTESIAN_POINT ( 'NONE',  ( -0.0003704575336267049244, -0.9283305954846620134, 0.08133701872469059624 ) ) ;
#19119 = CARTESIAN_POINT ( 'NONE',  ( 0.1833713392910780726, -1.690506555516771092, -0.6838718444642555294 ) ) ;
#19120 = AXIS2_PLACEMENT_3D ( 'NONE', #27881, #11637, #21096 ) ;
#19121 = CARTESIAN_POINT ( 'NONE',  ( 0.3629635372387383652, -1.169857193776045357, 0.4182417262808778013 ) ) ;
#19122 = ORIENTED_EDGE ( 'NONE', *, *, #27569, .T. ) ;
#19123 = ORIENTED_EDGE ( 'NONE', *, *, #879, .F. ) ;
#19124 = VECTOR ( 'NONE', #25701, 39.37007874015748854 ) ;
#19125 = DIRECTION ( 'NONE',  ( -1.387778780781449423E-15, 6.460451336368206514E-16, -1.000000000000000000 ) ) ;
#19126 = ORIENTED_EDGE ( 'NONE', *, *, #6142, .T. ) ;
#19127 = AXIS2_PLACEMENT_3D ( 'NONE', #6203, #18555, #31112 ) ;
#19128 = CARTESIAN_POINT ( 'NONE',  ( 0.7053410326410682885, -1.513865973459305625, 0.5669051209305092653 ) ) ;
#19129 = DIRECTION ( 'NONE',  ( 1.000000000000000000, -0.000000000000000000, -0.000000000000000000 ) ) ;
#19130 = CIRCLE ( 'NONE', #5945, 0.009999999999999991535 ) ;
#19131 = CARTESIAN_POINT ( 'NONE',  ( 0.5256885457656272909, -1.340177190190134704, 0.7859048212681565282 ) ) ;
#19133 = VERTEX_POINT ( 'NONE', #4602 ) ;
#19132 = CARTESIAN_POINT ( 'NONE',  ( 0.5800224671949608668, -1.618884289167087376, 0.4664561499407959833 ) ) ;
#19134 = VERTEX_POINT ( 'NONE', #29724 ) ;
#19135 = CARTESIAN_POINT ( 'NONE',  ( 0.1987699546958638652, -0.5941503706980315602, 0.3237227049863830031 ) ) ;
#19136 = ORIENTED_EDGE ( 'NONE', *, *, #25522, .T. ) ;
#19137 = CARTESIAN_POINT ( 'NONE',  ( 0.2964680571446819402, -1.656381576221859664, 0.5636775978236220341 ) ) ;
#19139 = CARTESIAN_POINT ( 'NONE',  ( 0.09204888577508196779, -1.303414576269683822, 0.5990285209990867665 ) ) ;
#19138 = CARTESIAN_POINT ( 'NONE',  ( 0.6374551337379976701, -1.567405544265130013, 0.4255985356709496292 ) ) ;
#19140 = CARTESIAN_POINT ( 'NONE',  ( 0.3812071769896587803, -1.763750790280042002, -0.4536492913031247021 ) ) ;
#19141 = DIRECTION ( 'NONE',  ( -0.4999999999999998890, -0.7377595849475270251, -0.4535535192433776119 ) ) ;
#19142 = EDGE_CURVE ( 'NONE', #8899, #22200, #5227, .T. ) ;
#19143 = CARTESIAN_POINT ( 'NONE',  ( -0.004088490883478934287, -1.369644552158580053, -0.6494983983435047570 ) ) ;
#19145 = ORIENTED_EDGE ( 'NONE', *, *, #26840, .F. ) ;
#19144 = ORIENTED_EDGE ( 'NONE', *, *, #21024, .F. ) ;
#19146 = SPHERICAL_SURFACE ( 'NONE', #13889, 0.01499999999999999944 ) ;
#19147 = CARTESIAN_POINT ( 'NONE',  ( 0.1852851918485090843, -0.8388979443186348472, 0.1523375349326095973 ) ) ;
#19148 = CARTESIAN_POINT ( 'NONE',  ( -0.03158843595483506322, -0.05459869295505906384, -0.4890616322892848977 ) ) ;
#19149 = CARTESIAN_POINT ( 'NONE',  ( 0.5787394239162922949, -1.425886802764863459, 0.7111292081977039770 ) ) ;
#19150 = CARTESIAN_POINT ( 'NONE',  ( -0.2399999999999999079, -2.811755946567116471, -0.3200729990151717774 ) ) ;
#19151 = CARTESIAN_POINT ( 'NONE',  ( 0.1386179493822486397, -1.168326298757728754, 0.9079011523149604912 ) ) ;
#19152 = CIRCLE ( 'NONE', #32927, 0.01000000000000001756 ) ;
#19153 = CARTESIAN_POINT ( 'NONE',  ( 0.05112782467887915655, -0.6866549243560603477, 0.6943072588412673163 ) ) ;
#19154 = VECTOR ( 'NONE', #9027, 39.37007874015748143 ) ;
#19155 = CARTESIAN_POINT ( 'NONE',  ( 0.4483572554135741850, -1.096823335528599674, -0.4056879302696327350 ) ) ;
#19156 = CIRCLE ( 'NONE', #30294, 0.01500000000000001159 ) ;
#19157 = DIRECTION ( 'NONE',  ( 0.4999551463232373427, -0.8660512985181134660, 0.000000000000000000 ) ) ;
#19158 = CARTESIAN_POINT ( 'NONE',  ( 0.3690276056097920865, -1.103968407447001088, 0.7607293476182939163 ) ) ;
#19159 = CARTESIAN_POINT ( 'NONE',  ( 0.3696577572605105888, -1.751079222393305823, -0.4256963421901115430 ) ) ;
#19160 = CIRCLE ( 'NONE', #32198, 0.03749999999977551152 ) ;
#19161 = VECTOR ( 'NONE', #22687, 39.37007874015748143 ) ;
#19162 = DIRECTION ( 'NONE',  ( 0.000000000000000000, 0.000000000000000000, 1.000000000000000000 ) ) ;
#19163 = CARTESIAN_POINT ( 'NONE',  ( 0.006340579314978117206, -0.5092170189304694450, 0.4201425565785884553 ) ) ;
#19164 = CARTESIAN_POINT ( 'NONE',  ( 0.1024573188296521581, -1.387117369751432516, 0.6458262573307184118 ) ) ;
#19165 = APPROVAL_ROLE ( '' ) ;
#19166 = CARTESIAN_POINT ( 'NONE',  ( -0.05634206451479800704, 0.4332270636364471406, 0.1516455289248359872 ) ) ;
#19167 = DIRECTION ( 'NONE',  ( -1.000000000000000000, -0.000000000000000000, -0.000000000000000000 ) ) ;
#19168 = ORIENTED_EDGE ( 'NONE', *, *, #1033, .T. ) ;
#19169 = DIRECTION ( 'NONE',  ( 0.000000000000000000, -0.7071067811865474617, -0.7071067811865474617 ) ) ;
#19170 = ORIENTED_EDGE ( 'NONE', *, *, #26043, .T. ) ;
#19171 = LINE ( 'NONE', #12578, #2055 ) ;
#19172 = CARTESIAN_POINT ( 'NONE',  ( 0.2620066386687194826, -1.629889363925806522, 0.8018636163776085013 ) ) ;
#19173 = AXIS2_PLACEMENT_3D ( 'NONE', #33348, #17912, #39729 ) ;
#19174 = CARTESIAN_POINT ( 'NONE',  ( 0.5618993035917507761, -1.439841365341236301, 0.7442830156648372331 ) ) ;
#19176 = VERTEX_POINT ( 'NONE', #2921 ) ;
#19175 = CARTESIAN_POINT ( 'NONE',  ( 0.4768848212686795929, -1.682051206446436797, -0.4156371400837810537 ) ) ;
#19178 = ORIENTED_EDGE ( 'NONE', *, *, #7018, .T. ) ;
#19177 = ORIENTED_EDGE ( 'NONE', *, *, #11210, .T. ) ;
#19179 = CARTESIAN_POINT ( 'NONE',  ( 0.5260973920735738663, -1.675551188129234204, -0.5699138614793077817 ) ) ;
#19180 = AXIS2_PLACEMENT_3D ( 'NONE', #34758, #37646, #3101 ) ;
#19181 = ORIENTED_EDGE ( 'NONE', *, *, #40315, .F. ) ;
#19182 = CIRCLE ( 'NONE', #4064, 0.2232808441893194829 ) ;
#19183 = CARTESIAN_POINT ( 'NONE',  ( 0.6278493015080260919, -1.616811722168019605, -0.5276078387673933667 ) ) ;
#19184 = PERSON_AND_ORGANIZATION ( #28918, #10295 ) ;
#19185 = DIRECTION ( 'NONE',  ( 0.8185200378235019114, 0.4725162423735941863, -0.3267313091433876049 ) ) ;
#19186 = VERTEX_POINT ( 'NONE', #11628 ) ;
#19187 = EDGE_CURVE ( 'NONE', #17094, #7319, #2176, .T. ) ;
#19188 = CARTESIAN_POINT ( 'NONE',  ( 0.1421881664906101961, -0.8149641224533534789, 0.5057660219216387754 ) ) ;
#19189 = CARTESIAN_POINT ( 'NONE',  ( 0.3941416742250357097, -1.601254223528187470, -0.3530575408666304371 ) ) ;
#19190 = CARTESIAN_POINT ( 'NONE',  ( 0.1111526859351814611, -0.6027224132271093993, 0.3326396559898295857 ) ) ;
#19191 = CARTESIAN_POINT ( 'NONE',  ( 0.6062242576285924445, -1.566401754662989587, -0.6176321414136997090 ) ) ;
#19192 = CARTESIAN_POINT ( 'NONE',  ( -0.02000000000000000042, -2.196071624283071788, -0.8624000883860228894 ) ) ;
#19193 = ORIENTED_EDGE ( 'NONE', *, *, #34731, .F. ) ;
#19194 = CARTESIAN_POINT ( 'NONE',  ( -0.1339136704200476757, -0.4685718226220191851, 0.09550516381870235993 ) ) ;
#19195 = CARTESIAN_POINT ( 'NONE',  ( 0.6208886523625545273, -1.439521707992974298, 0.8392336777283556648 ) ) ;
#19196 = EDGE_CURVE ( 'NONE', #25557, #5600, #32370, .T. ) ;
#19197 = VERTEX_POINT ( 'NONE', #5983 ) ;
#19198 = CARTESIAN_POINT ( 'NONE',  ( -0.02000000000000000042, -1.622350287959229087, -0.009600792027532436754 ) ) ;
#19199 = CARTESIAN_POINT ( 'NONE',  ( 0.1492234730455878899, -0.6341753046231629609, 0.3839420049399517310 ) ) ;
#19200 = CARTESIAN_POINT ( 'NONE',  ( 0.1902649460295288697, -0.8349739946900058829, 0.2559003878554159117 ) ) ;
#19201 = TOROIDAL_SURFACE ( 'NONE', #31032, 0.9237847906030132172, 0.01499999999999999944 ) ;
#19202 = CARTESIAN_POINT ( 'NONE',  ( 0.05567535398968421340, -1.335339640988971288, 0.4687417262808780127 ) ) ;
#19203 = CARTESIAN_POINT ( 'NONE',  ( -0.2043922129835731294, -0.5166151207188712791, 0.3750000000000001110 ) ) ;
#19204 = CARTESIAN_POINT ( 'NONE',  ( 0.07208523036626358904, -1.310649742666034401, 0.6665797303350883274 ) ) ;
#19205 = CARTESIAN_POINT ( 'NONE',  ( 0.5030539720840632167, -1.104010818905506675, 0.6157662270679344907 ) ) ;
#19206 = DATE_AND_TIME ( #19423, #12836 ) ;
#19207 = CIRCLE ( 'NONE', #20501, 0.1000000000000000194 ) ;
#19208 = DIRECTION ( 'NONE',  ( -3.406373435249024214E-19, -1.000000000000000000, -7.170354002788761615E-17 ) ) ;
#19209 = EDGE_CURVE ( 'NONE', #1394, #24994, #26779, .T. ) ;
#19210 = APPROVAL ( #12571, 'UNSPECIFIED' ) ;
#19211 = AXIS2_PLACEMENT_3D ( 'NONE', #28688, #555, #13051 ) ;
#19212 = DIRECTION ( 'NONE',  ( -1.000000000000000000, -2.280301054154495132E-31, 1.664003471950577689E-31 ) ) ;
#19213 = CARTESIAN_POINT ( 'NONE',  ( -0.03171102739523346675, 0.05432883045314864517, 0.4888204606144165854 ) ) ;
#19214 = ORIENTED_EDGE ( 'NONE', *, *, #26046, .T. ) ;
#19215 = CARTESIAN_POINT ( 'NONE',  ( 0.4491434351882165887, -1.570148841160289299, 0.6050572309278747785 ) ) ;
#19216 = DIRECTION ( 'NONE',  ( -1.355854680848614260E-31, 3.330669073875470114E-16, 1.000000000000000000 ) ) ;
#19217 = CARTESIAN_POINT ( 'NONE',  ( 0.08726992027127385143, -0.7030455430075180923, 0.02343504253866055334 ) ) ;
#19218 = B_SPLINE_CURVE_WITH_KNOTS ( 'NONE', 3,
 ( #730, #16529, #32158, #6640, #3780, #34830, #19430, #35039, #10157, #9744, #4172, #13043, #28873, #38534, #38121, #28463, #13448, #13638, #19215, #22727 ),
 .UNSPECIFIED., .F., .F.,
 ( 4, 2, 2, 2, 2, 2, 2, 2, 2, 4 ),
 ( 0.001303671507411563674, 0.001768902510528973845, 0.002234133513646384232, 0.002350441264425739106, 0.002466749015205093980, 0.002524902890594771850, 0.002583056765984450154, 0.002699364516763816738, 0.002931980018322547302, 0.003164595519881276998 ),
 .UNSPECIFIED. ) ;
#19219 = ORIENTED_EDGE ( 'NONE', *, *, #5886, .T. ) ;
#19220 = CARTESIAN_POINT ( 'NONE',  ( 0.3363288196684174891, -1.747766409858011238, 0.4536835104966877585 ) ) ;
#19221 = CARTESIAN_POINT ( 'NONE',  ( 0.04869497213076193903, -1.160534407236927246, 0.7642094061772998215 ) ) ;
#19223 = ORIENTED_EDGE ( 'NONE', *, *, #27507, .F. ) ;
#19222 = ORIENTED_EDGE ( 'NONE', *, *, #19530, .T. ) ;
#19224 = DIRECTION ( 'NONE',  ( -1.000000000000000000, -2.280301054154495132E-31, 1.664003471950577689E-31 ) ) ;
#19225 =( BOUNDED_SURFACE ( )  B_SPLINE_SURFACE ( 3, 2, ( 
 ( #1160, #12868, #34859 ),
 ( #6668, #4198, #19244 ),
 ( #31787, #13471, #3601 ),
 ( #10182, #16169, #26038 ),
 ( #28706, #25617, #9972 ),
 ( #31988, #3800, #16356 ),
 ( #28891, #22751, #35278 ),
 ( #38560, #7073, #19644 ) ),
 .UNSPECIFIED., .F., .F., .T. ) 
 B_SPLINE_SURFACE_WITH_KNOTS ( ( 4, 2, 2, 4 ),
 ( 3, 3 ),
 ( 0.001363486440777415343, 0.002314916752335400337, 0.002790631908114392726, 0.003266347063893385548 ),
 ( 0.000000000000000000, 1.000000000000000000 ),
 .UNSPECIFIED. ) 
 GEOMETRIC_REPRESENTATION_ITEM ( )  RATIONAL_B_SPLINE_SURFACE ( (
 ( 1.000000000000000000, 0.9128709291752513666, 1.000000000000000000),
 ( 1.000000000000000000, 0.9128773865067255633, 1.000000000000000000),
 ( 1.000000000000000000, 0.9126892044530536818, 1.000000000000000000),
 ( 1.000000000000000000, 0.9123262075125851966, 1.000000000000000000),
 ( 1.000000000000000000, 0.9121926916485024739, 1.000000000000000000),
 ( 1.000000000000000000, 0.9119580040447240465, 1.000000000000000000),
 ( 1.000000000000000000, 0.9118544196722184747, 1.000000000000000000),
 ( 1.000000000000000000, 0.9117915798251763349, 1.000000000000000000) ) ) 
 REPRESENTATION_ITEM ( '' )  SURFACE ( )  );
#19226 = ORIENTED_EDGE ( 'NONE', *, *, #8005, .T. ) ;
#19227 = CARTESIAN_POINT ( 'NONE',  ( -0.08000000000000000167, -2.183180860297908144, -0.4937760292030871079 ) ) ;
#19228 = CIRCLE ( 'NONE', #11354, 0.1762268159172233339 ) ;
#19230 = DIRECTION ( 'NONE',  ( -1.000000000000000000, 0.000000000000000000, 0.000000000000000000 ) ) ;
#19229 = CARTESIAN_POINT ( 'NONE',  ( 0.5982834170520250350, -1.597405224470788365, 0.4331267408012325903 ) ) ;
#19231 = CARTESIAN_POINT ( 'NONE',  ( 0.04946288932100069424, -0.3082365379450882070, -0.3644333945507132189 ) ) ;
#19232 = ORIENTED_EDGE ( 'NONE', *, *, #33062, .T. ) ;
#19233 = DIRECTION ( 'NONE',  ( -1.000000000000000000, -7.857794173099924470E-32, -8.628166150854818811E-32 ) ) ;
#19234 = ORIENTED_EDGE ( 'NONE', *, *, #13496, .F. ) ;
#19235 = CARTESIAN_POINT ( 'NONE',  ( 0.09655467777909068627, -0.5920640895833686468, 0.3065293990379648892 ) ) ;
#19236 = ORIENTED_EDGE ( 'NONE', *, *, #22119, .F. ) ;
#19237 = EDGE_LOOP ( 'NONE', ( #27124, #18317, #37852, #18717, #37123, #40489, #25054, #16001, #34150, #25884, #30015, #32133, #30369, #2679 ) ) ;
#19238 = ADVANCED_FACE ( 'NONE', ( #16289 ), #16117, .T. ) ;
#19239 = CIRCLE ( 'NONE', #17265, 0.4488493849861021068 ) ;
#19240 = LINE ( 'NONE', #38344, #21394 ) ;
#19241 = AXIS2_PLACEMENT_3D ( 'NONE', #22831, #25690, #19708 ) ;
#19242 = CARTESIAN_POINT ( 'NONE',  ( 0.07967440850021659249, -0.5998154657116770982, 0.3398716057233205912 ) ) ;
#19244 = CARTESIAN_POINT ( 'NONE',  ( -0.1157351144567332346, -0.4800210170677816079, 0.3382895569177964967 ) ) ;
#19243 = CARTESIAN_POINT ( 'NONE',  ( 0.009002175164704872418, -0.6190142101949668296, 0.4357503115026744034 ) ) ;
#19245 = CARTESIAN_POINT ( 'NONE',  ( 0.3699999999999786793, -2.183180860297921466, -0.5437760292030870968 ) ) ;
#19246 = FACE_OUTER_BOUND ( 'NONE', #29546, .T. ) ;
#19247 = CIRCLE ( 'NONE', #25832, 0.1346589359789736318 ) ;
#19248 = EDGE_CURVE ( 'NONE', #39819, #34187, #37460, .T. ) ;
#19249 = FACE_OUTER_BOUND ( 'NONE', #21319, .T. ) ;
#19250 = CARTESIAN_POINT ( 'NONE',  ( 0.2914072444767246695, -1.544007756657866270, -0.3072620149518441313 ) ) ;
#19251 = EDGE_CURVE ( 'NONE', #6931, #4571, #35673, .T. ) ;
#19252 = CARTESIAN_POINT ( 'NONE',  ( 0.2732903649954732117, -0.9481965803008104432, 0.7299041271556375721 ) ) ;
#19253 = CARTESIAN_POINT ( 'NONE',  ( -0.05083665881509068230, 0.3162195626322023556, 0.3525671453250067700 ) ) ;
#19254 = AXIS2_PLACEMENT_3D ( 'NONE', #34866, #13074, #12654 ) ;
#19255 = CARTESIAN_POINT ( 'NONE',  ( -0.03672309138969640646, -0.4430277080971899983, -0.1868557463394342477 ) ) ;
#19256 = CARTESIAN_POINT ( 'NONE',  ( 0.1382093149295521017, -0.7546047068524435186, 0.5802775608379149297 ) ) ;
#19257 = CARTESIAN_POINT ( 'NONE',  ( 0.3544525855956190963, -1.628498139902242681, -0.6593841416022943047 ) ) ;
#19258 = CARTESIAN_POINT ( 'NONE',  ( 0.3319931610750171957, -0.8547376211461308326, 0.6892644829257473793 ) ) ;
#19259 = DIRECTION ( 'NONE',  ( -1.000000000000000000, -0.000000000000000000, -0.000000000000000000 ) ) ;
#19260 = EDGE_CURVE ( 'NONE', #29556, #18607, #10713, .T. ) ;
#19261 = CARTESIAN_POINT ( 'NONE',  ( 0.06116565050235212714, -1.313871996917011398, 0.6258069960581069680 ) ) ;
#19262 = CIRCLE ( 'NONE', #24526, 0.05330708661417327826 ) ;
#19263 = B_SPLINE_CURVE_WITH_KNOTS ( 'NONE', 3,
 ( #30783, #27911, #30588, #40450 ),
 .UNSPECIFIED., .F., .F.,
 ( 4, 4 ),
 ( 0.000000000000000000, 5.151976560715283563E-05 ),
 .UNSPECIFIED. ) ;
#19264 = CARTESIAN_POINT ( 'NONE',  ( -0.2399999999999999079, -4.233163482269810096, -0.5148221395285308422 ) ) ;
#19265 = MANIFOLD_SOLID_BREP ( 'Chamfer1', #33228 ) ;
#19266 = CYLINDRICAL_SURFACE ( 'NONE', #9422, 0.1000000000000000194 ) ;
#19267 = CARTESIAN_POINT ( 'NONE',  ( 0.1767056452462499871, -0.9130954350749045378, 0.6111087866971379734 ) ) ;
#19268 = CARTESIAN_POINT ( 'NONE',  ( 0.03868264068766660846, 0.03360988006412097412, 0.4753775160315155124 ) ) ;
#19269 = CARTESIAN_POINT ( 'NONE',  ( 0.6910433967563797131, -1.503458314657174721, 0.4665392483146700298 ) ) ;
#19270 = AXIS2_PLACEMENT_3D ( 'NONE', #28307, #12665, #28120 ) ;
#19271 = ORIENTED_EDGE ( 'NONE', *, *, #14668, .T. ) ;
#19272 = DIRECTION ( 'NONE',  ( 0.8660512985181135770, 0.4999551463232368431, 0.000000000000000000 ) ) ;
#19273 = CARTESIAN_POINT ( 'NONE',  ( 0.01548846960712797240, -0.07651041855115535417, -0.5222379212567069828 ) ) ;
#19274 = DIRECTION ( 'NONE',  ( 0.000000000000000000, 0.000000000000000000, -1.000000000000000000 ) ) ;
#19275 = CARTESIAN_POINT ( 'NONE',  ( 0.3484677573834994435, -1.177852168535778565, 0.4182417262808778013 ) ) ;
#19276 = AXIS2_PLACEMENT_3D ( 'NONE', #19523, #12944, #32057 ) ;
#19277 = VERTEX_POINT ( 'NONE', #10500 ) ;
#19278 = DIRECTION ( 'NONE',  ( 0.4999551463232373427, -0.8660512985181134660, 0.000000000000000000 ) ) ;
#19279 = CIRCLE ( 'NONE', #26501, 0.04330708661417340122 ) ;
#19280 = CARTESIAN_POINT ( 'NONE',  ( 0.2953996865216445000, -1.312084307709316278, 0.4675629788832125211 ) ) ;
#19281 = CARTESIAN_POINT ( 'NONE',  ( 0.4857864678016971527, -1.660707689634011386, 0.4964627840106182188 ) ) ;
#19282 = DIRECTION ( 'NONE',  ( -0.7956551220374292743, -0.4593167559955302903, 0.3949190352937497761 ) ) ;
#19283 = CARTESIAN_POINT ( 'NONE',  ( 0.4580930487831912923, -1.228282708841101689, 0.7098083865471490617 ) ) ;
#19284 = PLANE ( 'NONE',  #23948 ) ;
#19285 = CARTESIAN_POINT ( 'NONE',  ( 0.4907992349987285730, -1.081537398447262266, 0.5876768462667140147 ) ) ;
#19286 = ORIENTED_EDGE ( 'NONE', *, *, #24589, .F. ) ;
#19287 = PERSON_AND_ORGANIZATION_ROLE ( 'classification_officer' ) ;
#19288 = CARTESIAN_POINT ( 'NONE',  ( 0.08396792514988114797, -1.274408769650567708, 0.7373487296590384155 ) ) ;
#19289 = ORIENTED_EDGE ( 'NONE', *, *, #38123, .T. ) ;
#19290 = EDGE_CURVE ( 'NONE', #4083, #1840, #26765, .T. ) ;
#19291 = CARTESIAN_POINT ( 'NONE',  ( 0.1520549073577694699, -0.9832709360364392248, 0.7962433701957113419 ) ) ;
#19293 = DIRECTION ( 'NONE',  ( 0.4999551463232373427, -0.8660512985181134660, 0.000000000000000000 ) ) ;
#19292 = CARTESIAN_POINT ( 'NONE',  ( 0.06524015413155181964, -0.8058748789547460767, 0.05685236492229539529 ) ) ;
#19294 = CARTESIAN_POINT ( 'NONE',  ( 0.1970768337340418341, -2.011495956325795920, -0.3159642937727323853 ) ) ;
#19295 = ORIENTED_EDGE ( 'NONE', *, *, #34421, .T. ) ;
#19296 = ADVANCED_FACE ( 'NONE', ( #10321 ), #26490, .T. ) ;
#19297 = ORIENTED_EDGE ( 'NONE', *, *, #20480, .T. ) ;
#19298 = CARTESIAN_POINT ( 'NONE',  ( 0.3417327841951403045, -1.285448577080334998, 0.5750830755287759111 ) ) ;
#19299 = EDGE_CURVE ( 'NONE', #2835, #2630, #8732, .T. ) ;
#19300 = CARTESIAN_POINT ( 'NONE',  ( 0.5552477155703334777, -1.480784202266746341, 0.7056114995199435080 ) ) ;
#19301 = VERTEX_POINT ( 'NONE', #1278 ) ;
#19302 = CARTESIAN_POINT ( 'NONE',  ( -0.3000000000000000999, -2.183180860297908144, -0.4937760292030871079 ) ) ;
#19303 = CARTESIAN_POINT ( 'NONE',  ( 0.5284862694945503536, -1.177654592776627318, -0.5155029497116575543 ) ) ;
#19304 = CIRCLE ( 'NONE', #11417, 0.01499999999999995434 ) ;
#19305 = VECTOR ( 'NONE', #1421, 39.37007874015748143 ) ;
#19306 = CARTESIAN_POINT ( 'NONE',  ( 1.132682595522134681E-16, -4.942613344993767655E-17, 0.07499999999999977518 ) ) ;
#19307 = ADVANCED_FACE ( 'NONE', ( #13783 ), #13389, .T. ) ;
#19308 = CARTESIAN_POINT ( 'NONE',  ( 0.1844690651293379724, -0.8537165418084496915, 0.1701664619867762351 ) ) ;
#19309 = LINE ( 'NONE', #16612, #12817 ) ;
#19310 = CARTESIAN_POINT ( 'NONE',  ( 0.08875358319671960983, -0.6432264665877226451, 0.1460232572880605928 ) ) ;
#19311 = CIRCLE ( 'NONE', #33095, 0.5156329413417588547 ) ;
#19312 = CARTESIAN_POINT ( 'NONE',  ( 0.5337404313129848754, -1.165174529015815530, 0.8761190665599410954 ) ) ;
#19313 = CARTESIAN_POINT ( 'NONE',  ( 0.1949656944119497748, -2.006413414762151515, -0.7037340768493718368 ) ) ;
#19314 = EDGE_CURVE ( 'NONE', #9065, #9709, #35063, .T. ) ;
#19315 = AXIS2_PLACEMENT_3D ( 'NONE', #24808, #25981, #10334 ) ;
#19316 = DIRECTION ( 'NONE',  ( -0.9378410757839559242, 0.1072489841977647268, -0.3300784330442382841 ) ) ;
#19317 = DIRECTION ( 'NONE',  ( -0.4999551463232372317, 0.8660512985181135770, -0.000000000000000000 ) ) ;
#19318 = APPROVAL_ROLE ( '' ) ;
#19319 = EDGE_CURVE ( 'NONE', #7253, #1152, #23281, .T. ) ;
#19320 = DIRECTION ( 'NONE',  ( -0.05576617208936890391, -0.2535907321052872088, -0.9657027879429589401 ) ) ;
#19321 = EDGE_CURVE ( 'NONE', #30110, #7904, #3670, .T. ) ;
#19322 = CARTESIAN_POINT ( 'NONE',  ( 0.02953079040095728247, 0.000000000000000000, 0.000000000000000000 ) ) ;
#19323 = CARTESIAN_POINT ( 'NONE',  ( 0.5434391066227751699, -1.168983680377609691, 0.5856983068965047057 ) ) ;
#19324 = CARTESIAN_POINT ( 'NONE',  ( 0.2643655332618012888, -1.686843913603420342, 0.5679419890486603339 ) ) ;
#19325 = CARTESIAN_POINT ( 'NONE',  ( 0.005948235723147832048, -0.6142029534155015735, 0.3540208382306603840 ) ) ;
#19326 = CARTESIAN_POINT ( 'NONE',  ( 0.0003922654375693484163, -0.4465883730080376646, 0.08090056108615809038 ) ) ;
#19327 = B_SPLINE_CURVE_WITH_KNOTS ( 'NONE', 3,
 ( #27714, #15582, #30604, #9388, #18876, #21965, #40043, #18253 ),
 .UNSPECIFIED., .F., .F.,
 ( 4, 2, 2, 4 ),
 ( 0.000000000000000000, 0.001677695221323086258, 0.002516542831984629278, 0.003355390442646172516 ),
 .UNSPECIFIED. ) ;
#19328 = CIRCLE ( 'NONE', #33108, 0.07999999999999996003 ) ;
#19329 = CARTESIAN_POINT ( 'NONE',  ( 0.2488895021796825036, -1.574756068310029455, -0.7071313240274791356 ) ) ;
#19330 = DIRECTION ( 'NONE',  ( -8.881784197001246407E-16, 2.361472542561082612E-16, -1.000000000000000000 ) ) ;
#19331 = ORIENTED_EDGE ( 'NONE', *, *, #2991, .F. ) ;
#19332 = AXIS2_PLACEMENT_3D ( 'NONE', #34282, #6305, #27519 ) ;
#19333 = ORIENTED_EDGE ( 'NONE', *, *, #37220, .F. ) ;
#19334 = CIRCLE ( 'NONE', #33087, 0.1600000000000005029 ) ;
#19335 = DIRECTION ( 'NONE',  ( 1.000000000000000000, -1.213308482346468028E-12, -2.286601241528066538E-12 ) ) ;
#19336 = EDGE_LOOP ( 'NONE', ( #18123, #8398, #14713 ) ) ;
#19337 = CARTESIAN_POINT ( 'NONE',  ( -0.04230188431063477972, -0.008729788072060947965, 0.4686063437799720677 ) ) ;
#19338 = CARTESIAN_POINT ( 'NONE',  ( 0.3543393621149266148, -1.718158840355286765, -0.4818782773072323722 ) ) ;
#19339 = CARTESIAN_POINT ( 'NONE',  ( 0.5962429284462779089, -1.457299488734417281, 0.6386903328529611734 ) ) ;
#19341 = VERTEX_POINT ( 'NONE', #15209 ) ;
#19340 = CARTESIAN_POINT ( 'NONE',  ( 0.1984950629327257021, -1.252696871964387393, -0.5155029497116575543 ) ) ;
#19342 = AXIS2_PLACEMENT_3D ( 'NONE', #8965, #37154, #11841 ) ;
#19343 = EDGE_LOOP ( 'NONE', ( #25613, #16197, #9203, #33521 ) ) ;
#19344 = CARTESIAN_POINT ( 'NONE',  ( -0.08000000000000000167, -1.622350287959229087, -0.009600792027532436754 ) ) ;
#19345 = VERTEX_POINT ( 'NONE', #37012 ) ;
#19346 = CARTESIAN_POINT ( 'NONE',  ( 0.01081953179195815559, -0.5297023241700838936, 0.1457185332388694354 ) ) ;
#19348 = CARTESIAN_POINT ( 'NONE',  ( 0.1959282438327735465, -1.265725308457275045, -0.3194741108003418262 ) ) ;
#19347 = CARTESIAN_POINT ( 'NONE',  ( 0.6358170330921433244, -1.565712325321040987, 0.4189323858537951639 ) ) ;
#19349 = FACE_OUTER_BOUND ( 'NONE', #27776, .T. ) ;
#19350 = CARTESIAN_POINT ( 'NONE',  ( 0.01200886551622900103, -0.4814612145085635508, -0.01224044998698113965 ) ) ;
#19351 = ADVANCED_FACE ( 'NONE', ( #33505 ), #5746, .F. ) ;
#19352 = CARTESIAN_POINT ( 'NONE',  ( 0.04109334229010794953, -1.703983732577595056, -0.3380635556694617239 ) ) ;
#19354 = ORIENTED_EDGE ( 'NONE', *, *, #20114, .F. ) ;
#19353 = ORIENTED_EDGE ( 'NONE', *, *, #36279, .T. ) ;
#19355 = B_SPLINE_CURVE_WITH_KNOTS ( 'NONE', 3,
 ( #34603, #6406, #3315, #15880, #29240, #10113, #29442, #38084, #35605, #3925 ),
 .UNSPECIFIED., .F., .F.,
 ( 4, 2, 2, 2, 4 ),
 ( 0.000000000000000000, 0.2500000000000000000, 0.5000000000000000000, 0.7500000000000000000, 1.000000000000000000 ),
 .UNSPECIFIED. ) ;
#19356 = EDGE_CURVE ( 'NONE', #25455, #35064, #17266, .T. ) ;
#19357 = CARTESIAN_POINT ( 'NONE',  ( 0.4751758298663427693, -1.652426242819087010, -0.6334442537810193175 ) ) ;
#19358 = CARTESIAN_POINT ( 'NONE',  ( 0.1109049718728753187, -0.9286333055842326267, 0.1462684119608117506 ) ) ;
#19359 = CARTESIAN_POINT ( 'NONE',  ( -0.01548846960712824648, 0.07651041855115098267, -0.5222379212567075379 ) ) ;
#19360 = CARTESIAN_POINT ( 'NONE',  ( 0.5765078172467388296, -1.467567902266393887, 0.7032344926564899623 ) ) ;
#19361 =( BOUNDED_SURFACE ( )  B_SPLINE_SURFACE ( 3, 2, ( 
 ( #34895, #3641, #4023 ),
 ( #35494, #19672, #13511 ),
 ( #26074, #4236, #38592 ),
 ( #16203, #10414, #28738 ) ),
 .UNSPECIFIED., .F., .F., .T. ) 
 B_SPLINE_SURFACE_WITH_KNOTS ( ( 4, 4 ),
 ( 3, 3 ),
 ( -8.673617379884035472E-19, 0.0003267904260525523758 ),
 ( 0.000000000000000000, 1.000000000000000000 ),
 .UNSPECIFIED. ) 
 GEOMETRIC_REPRESENTATION_ITEM ( )  RATIONAL_B_SPLINE_SURFACE ( (
 ( 1.000000000000000000, 0.7071189998922904341, 1.000000000000000000),
 ( 1.000000000000000000, 0.7071106962636509730, 1.000000000000000000),
 ( 1.000000000000000000, 0.7071067813167358773, 1.000000000000000000),
 ( 1.000000000000000000, 0.7071067811865512365, 1.000000000000000000) ) ) 
 REPRESENTATION_ITEM ( '' )  SURFACE ( )  );
#19362 = CARTESIAN_POINT ( 'NONE',  ( 0.1678358338209908485, -0.8626253651800752653, 0.4958334663961649902 ) ) ;
#19363 = CARTESIAN_POINT ( 'NONE',  ( -1.019575837292305609, -0.04310840302198155199, 0.3599999999999999867 ) ) ;
#19364 = DIRECTION ( 'NONE',  ( -1.000000000000000000, -2.276539994720197063E-15, 5.691349986800492658E-16 ) ) ;
#19365 = AXIS2_PLACEMENT_3D ( 'NONE', #35986, #16875, #17263 ) ;
#19366 = VECTOR ( 'NONE', #24687, 39.37007874015748143 ) ;
#19367 = DIRECTION ( 'NONE',  ( -1.000000000000000000, -2.276539994720197063E-15, 5.691349986800492658E-16 ) ) ;
#19368 = DIRECTION ( 'NONE',  ( -0.4999551463232372317, 0.8660512985181134660, -0.000000000000000000 ) ) ;
#19369 = VECTOR ( 'NONE', #32021, 39.37007874015748143 ) ;
#19370 = CARTESIAN_POINT ( 'NONE',  ( 0.1852718761952666104, -0.8389489029336036907, 0.1457185345930598341 ) ) ;
#19371 = CARTESIAN_POINT ( 'NONE',  ( 0.4434344506101033923, -1.107353083073178146, -0.6343966985258274738 ) ) ;
#19372 = DIRECTION ( 'NONE',  ( 0.000000000000000000, 0.000000000000000000, 1.000000000000000000 ) ) ;
#19373 = APPROVAL_PERSON_ORGANIZATION ( #6, #30992, #15169 ) ;
#19374 = CARTESIAN_POINT ( 'NONE',  ( 0.04308611741967745268, -0.3346393142056199310, 0.3638101219460039282 ) ) ;
#19375 = LINE ( 'NONE', #680, #24467 ) ;
#19376 = CIRCLE ( 'NONE', #981, 0.06250000000000001388 ) ;
#19377 = CARTESIAN_POINT ( 'NONE',  ( 0.1801850755352660816, -1.895435244648604245, -0.6572603376541747977 ) ) ;
#19378 = DATE_AND_TIME ( #37668, #23403 ) ;
#19379 = CARTESIAN_POINT ( 'NONE',  ( 0.4101899714674371866, -1.674693119776962336, -0.5152975299054542990 ) ) ;
#19380 = CARTESIAN_POINT ( 'NONE',  ( -0.04285640132273837999, 0.4433417433457839119, 0.2197472875419949068 ) ) ;
#19381 = DIRECTION ( 'NONE',  ( -1.000000000000000000, -0.000000000000000000, -0.000000000000000000 ) ) ;
#19382 = ORIENTED_EDGE ( 'NONE', *, *, #9377, .T. ) ;
#19383 = CARTESIAN_POINT ( 'NONE',  ( 0.1942945430039405008, -0.5567045476596680365, 0.2821869111984989242 ) ) ;
#19384 = EDGE_LOOP ( 'NONE', ( #38102, #19023, #12743, #30748, #31340 ) ) ;
#19385 = FACE_OUTER_BOUND ( 'NONE', #3318, .T. ) ;
#19386 = DIRECTION ( 'NONE',  ( -0.4999999999999969469, 0.2622817173645498601, 0.8253534398888184853 ) ) ;
#19387 = VECTOR ( 'NONE', #6057, 39.37007874015748143 ) ;
#19388 = CARTESIAN_POINT ( 'NONE',  ( 0.5916383604625806703, -1.478183414026097653, 0.6639549887419504692 ) ) ;
#19390 = VERTEX_POINT ( 'NONE', #17677 ) ;
#19389 = DIRECTION ( 'NONE',  ( -6.162975822039154730E-33, 0.000000000000000000, -1.000000000000000000 ) ) ;
#19391 = CIRCLE ( 'NONE', #1665, 0.04330708661417327632 ) ;
#19393 = ORIENTED_EDGE ( 'NONE', *, *, #14984, .T. ) ;
#19392 = ORIENTED_EDGE ( 'NONE', *, *, #28978, .T. ) ;
#19394 = FACE_OUTER_BOUND ( 'NONE', #12703, .T. ) ;
#19395 = AXIS2_PLACEMENT_3D ( 'NONE', #34886, #26064, #25643 ) ;
#19396 = ORIENTED_EDGE ( 'NONE', *, *, #4372, .F. ) ;
#19397 = CYLINDRICAL_SURFACE ( 'NONE', #23930, 0.1749999999999999889 ) ;
#19398 = PRODUCT_DEFINITION_FORMATION_WITH_SPECIFIED_SOURCE ( 'ANY', '', #21216, .NOT_KNOWN. ) ;
#19399 = CARTESIAN_POINT ( 'NONE',  ( 0.6209541335343498059, -1.620792173117170609, -0.5418768570690311037 ) ) ;
#19400 = B_SPLINE_CURVE_WITH_KNOTS ( 'NONE', 3,
 ( #17523, #30073, #39130, #25992, #13620, #13810, #29872, #38516, #8042, #10954, #32538, #10347, #4356, #23516, #1711, #26185, #36228, #14229, #38709, #32939, #36031, #10529, #16917, #29461, #1305, #26380, #7835, #20406, #26794, #39321, #30474, #34717, #31636, #30684, #28345, #9629, #27591, #23911, #36441, #12505 ),
 .UNSPECIFIED., .F., .F.,
 ( 4, 2, 2, 2, 2, 2, 2, 2, 2, 2, 2, 2, 2, 2, 2, 2, 2, 2, 2, 4 ),
 ( -5.999999991662925479E-08, 0.0006628589721972678959, 0.001325777944394452386, 0.001988696916591636658, 0.002651615888788821148, 0.003314534860986005638, 0.003977453833183190561, 0.004640372805380374617, 0.005303291777577559540, 0.006629129721971918111, 0.007292048694169097831, 0.007954967666366280152, 0.008617886638563462473, 0.009280805610760644794, 0.01060664355515499729, 0.01193248149954934806, 0.01325831944394370229, 0.01590999533273240382, 0.01856167122152111229, 0.02121334711030981729 ),
 .UNSPECIFIED. ) ;
#19401 = CALENDAR_DATE ( 2026, 13, 10 ) ;
#19402 = CARTESIAN_POINT ( 'NONE',  ( -2.070754768975505034, -0.09959325338431362917, 0.3602693341844379060 ) ) ;
#19403 = ORIENTED_EDGE ( 'NONE', *, *, #12490, .T. ) ;
#19404 = CARTESIAN_POINT ( 'NONE',  ( 0.1009731816307408991, -0.7855298059080080275, 0.3453887576930584902 ) ) ;
#19405 = CIRCLE ( 'NONE', #24663, 0.5614999999999926716 ) ;
#19406 = CARTESIAN_POINT ( 'NONE',  ( 0.08990536851188023204, -0.5646295468556784547, 0.1437216542238681782 ) ) ;
#19407 = CARTESIAN_POINT ( 'NONE',  ( 0.5100517597868143849, -1.467776873700488371, 0.7596160885929598150 ) ) ;
#19408 = CARTESIAN_POINT ( 'NONE',  ( 0.1876095839365586326, -1.270310460104812966, 0.4182417262808778013 ) ) ;
#19409 = DIRECTION ( 'NONE',  ( -1.000000000000000000, -2.280301054154495132E-31, 1.664003471950577689E-31 ) ) ;
#19410 = CARTESIAN_POINT ( 'NONE',  ( 0.7036498145888742117, -1.518298014128231843, 0.5677572928519309947 ) ) ;
#19411 = CARTESIAN_POINT ( 'NONE',  ( 0.3924667225388316916, -1.718121829093100406, 0.6106704844410693056 ) ) ;
#19412 = CARTESIAN_POINT ( 'NONE',  ( 0.6620118083207074955, -1.538948419689354363, 0.7089722153523403403 ) ) ;
#19413 = CARTESIAN_POINT ( 'NONE',  ( 0.4521982902084413225, -1.612316853396095429, -0.6577709497374332193 ) ) ;
#19414 = CARTESIAN_POINT ( 'NONE',  ( 0.2858528607535977262, -0.9443831972166216726, 0.7228252558026528884 ) ) ;
#19415 = CARTESIAN_POINT ( 'NONE',  ( -0.002306167831732802449, -0.8472269691890851329, 0.1380695624520867359 ) ) ;
#19416 = AXIS2_PLACEMENT_3D ( 'NONE', #17264, #4905, #32695 ) ;
#19417 = CARTESIAN_POINT ( 'NONE',  ( 0.4959778976180506116, -1.681391946368784751, -0.5155029497116575543 ) ) ;
#19418 = VECTOR ( 'NONE', #4648, 39.37007874015748143 ) ;
#19419 = DIMENSIONAL_EXPONENTS ( 1.000000000000000000, 0.000000000000000000, 0.000000000000000000, 0.000000000000000000, 0.000000000000000000, 0.000000000000000000, 0.000000000000000000 ) ;
#19420 = DIRECTION ( 'NONE',  ( 0.000000000000000000, 0.000000000000000000, -1.000000000000000000 ) ) ;
#19421 = CARTESIAN_POINT ( 'NONE',  ( 0.03259135683726806926, -1.157323147438684030, 0.6652026314908382476 ) ) ;
#19422 = CARTESIAN_POINT ( 'NONE',  ( 0.3146548270004942971, -0.9167534899940792403, 0.6079632372063322743 ) ) ;
#19423 = CALENDAR_DATE ( 2026, 13, 10 ) ;
#19424 = CARTESIAN_POINT ( 'NONE',  ( -0.1082158540381434886, -0.4935046016075740338, 0.3575786101922727722 ) ) ;
#19425 = SECURITY_CLASSIFICATION ( '', '', #5980 ) ;
#19426 = CARTESIAN_POINT ( 'NONE',  ( -0.03159140494780127151, 0.4819881711443534389, -0.09921162977303643604 ) ) ;
#19427 = AXIS2_PLACEMENT_3D ( 'NONE', #9078, #34772, #6188 ) ;
#19428 = CARTESIAN_POINT ( 'NONE',  ( 0.4155056390950594980, -1.153651200484786532, 0.4182417262808778569 ) ) ;
#19429 = VERTEX_POINT ( 'NONE', #2058 ) ;
#19430 = CARTESIAN_POINT ( 'NONE',  ( 0.4358234066720084177, -1.577671767360221411, 0.5885670104086981880 ) ) ;
#19431 = CARTESIAN_POINT ( 'NONE',  ( 0.002296835029421147919, -0.5198933010532066357, 0.1431176680404081247 ) ) ;
#19432 = CARTESIAN_POINT ( 'NONE',  ( 0.08515941055999551312, -0.8106121384747535519, 0.1370161859660417591 ) ) ;
#19433 = ORIENTED_EDGE ( 'NONE', *, *, #16057, .F. ) ;
#19434 = DIRECTION ( 'NONE',  ( 0.9480245940703961871, 0.3181970600707375030, -1.138269997360106420E-15 ) ) ;
#19435 = CARTESIAN_POINT ( 'NONE',  ( 0.1637184504418466302, -1.361439334600449413, 0.6509539637277043100 ) ) ;
#19437 = EDGE_LOOP ( 'NONE', ( #19493, #6925, #34294, #10218 ) ) ;
#19436 = ORIENTED_EDGE ( 'NONE', *, *, #39902, .F. ) ;
#19438 = FACE_OUTER_BOUND ( 'NONE', #14455, .T. ) ;
#19439 = CARTESIAN_POINT ( 'NONE',  ( 0.1464009668243671236, -1.281690631858763085, 0.4243433165416301001 ) ) ;
#19440 = DIRECTION ( 'NONE',  ( -0.8660512985181132439, -0.4999551463232376758, 0.000000000000000000 ) ) ;
#19441 = CARTESIAN_POINT ( 'NONE',  ( 0.5933601670058918920, -1.600162351846436959, 0.4297890903611187308 ) ) ;
#19442 = CLOSED_SHELL ( 'NONE', ( #21480, #18269, #24090, #18545, #21599, #30577, #7361, #22740, #29500, #24537, #16275, #21291, #1163, #4379, #9668, #39565, #5986, #32119, #32553, #34209, #29961, #33536, #37064, #37583, #4131, #8274, #2893, #5932, #33641, #35130, #26892, #38972, #21260, #17681, #14917, #38147, #19351, #23053, #35935, #14906, #16591, #2391, #5833, #5608, #18487, #28869, #37621, #33404, #18028, #14167, #9681 ) ) ;
#19443 = CARTESIAN_POINT ( 'NONE',  ( 0.05076679145662187087, -0.3165345149637547872, -0.3525336044145329084 ) ) ;
#19444 = ORIENTED_EDGE ( 'NONE', *, *, #29769, .F. ) ;
#19445 = CARTESIAN_POINT ( 'NONE',  ( 0.04687499999999977102, -0.4772001287898267607, 0.3417740242638161452 ) ) ;
#19446 = CARTESIAN_POINT ( 'NONE',  ( 0.1008052951643304829, -0.6052764826558847400, 0.3473834472754093738 ) ) ;
#19447 = CARTESIAN_POINT ( 'NONE',  ( 0.05299811827002062770, -0.7416351888791600233, 0.7575765924777226878 ) ) ;
#19448 = CARTESIAN_POINT ( 'NONE',  ( 0.4694448353715036659, -1.557891597669167849, 0.5687246758769614052 ) ) ;
#19450 = DIRECTION ( 'NONE',  ( -1.000000000000000000, -0.000000000000000000, -0.000000000000000000 ) ) ;
#19449 = CARTESIAN_POINT ( 'NONE',  ( 0.5008954076588254534, -1.585800327213603200, -0.4745784240349925631 ) ) ;
#19451 = DIRECTION ( 'NONE',  ( 1.000000000000000000, 2.280301054154495132E-31, -1.664003471950577689E-31 ) ) ;
#19452 = CARTESIAN_POINT ( 'NONE',  ( 0.2113724693258398346, -0.9282255387282759562, 0.3698535518934624733 ) ) ;
#19453 = APPROVAL_PERSON_ORGANIZATION ( #17357, #4827, #32025 ) ;
#19454 = APPROVAL ( #6713, 'UNKNOWN' ) ;
#19455 = VERTEX_POINT ( 'NONE', #21413 ) ;
#19456 = UNCERTAINTY_MEASURE_WITH_UNIT (LENGTH_MEASURE( 1.000000000000000082E-05 ), #7660, 'distance_accuracy_value', 'NONE');
#19457 = CARTESIAN_POINT ( 'NONE',  ( 0.6865478901158108549, -1.574312610877731000, 0.5182417262812423209 ) ) ;
#19458 = CARTESIAN_POINT ( 'NONE',  ( 0.1897112079047655053, -0.5340520988485696341, 0.1458683203705843090 ) ) ;
#19459 = VECTOR ( 'NONE', #19519, 39.37007874015748854 ) ;
#19460 = CARTESIAN_POINT ( 'NONE',  ( -0.01899468245561687987, 0.3622301702732946826, -0.3730449234618297694 ) ) ;
#19461 = CARTESIAN_POINT ( 'NONE',  ( -0.02881302694829757094, -0.4517620879735247397, -0.2100235834770130539 ) ) ;
#19462 = CARTESIAN_POINT ( 'NONE',  ( 0.03113248654051816583, 0.1919340784543128453, -0.1767348310837237868 ) ) ;
#19463 = B_SPLINE_CURVE_WITH_KNOTS ( 'NONE', 3,
 ( #8773, #30789, #17826, #27101, #37361, #34072, #36749, #12281, #30181, #24423, #2418, #15146, #14756, #33660, #14537, #30385, #5873, #20742, #18244, #2011, #24225, #12075, #30987, #40457 ),
 .UNSPECIFIED., .F., .F.,
 ( 4, 2, 2, 2, 2, 2, 2, 2, 2, 2, 2, 4 ),
 ( 0.000000000000000000, 0.002721158394890018685, 0.005442316789780037370, 0.008163475184670055187, 0.01088463357956007474, 0.01360579197445009429, 0.01632695036934011037, 0.01768752956678512275, 0.01904810876423013166, 0.01972839836295263091, 0.02040868796167513710, 0.02176926715912013560 ),
 .UNSPECIFIED. ) ;
#19464 = CARTESIAN_POINT ( 'NONE',  ( 0.1918124086860224231, -0.5891232155910660628, 0.2119633080407007653 ) ) ;
#19465 = EDGE_CURVE ( 'NONE', #14547, #13190, #2274, .T. ) ;
#19466 = DIRECTION ( 'NONE',  ( -8.881784197001246407E-16, 2.361472542561082612E-16, -1.000000000000000000 ) ) ;
#19467 = CARTESIAN_POINT ( 'NONE',  ( 0.05768477182288792027, -1.318213558294332621, 0.6059538573116379778 ) ) ;
#19468 = CARTESIAN_POINT ( 'NONE',  ( 0.04762035657659004911, 0.4700462218748536758, -0.1075639008183982559 ) ) ;
#19469 = CARTESIAN_POINT ( 'NONE',  ( 0.1940226371263356897, -0.6293705748991054172, 0.3231715484426654350 ) ) ;
#19470 = CARTESIAN_POINT ( 'NONE',  ( 0.2934445204131819196, -1.040484148307386780, 0.7330325571301972154 ) ) ;
#19471 = DIRECTION ( 'NONE',  ( -1.664003471950577032E-31, -3.330669073875470607E-16, -1.000000000000000000 ) ) ;
#19472 = CARTESIAN_POINT ( 'NONE',  ( 0.6753500143071270445, -1.527325197043427174, 0.4408735696681176930 ) ) ;
#19473 = ADVANCED_FACE ( 'NONE', ( #5933 ), #34129, .F. ) ;
#19474 = APPROVAL_PERSON_ORGANIZATION ( #33801, #32756, #18362 ) ;
#19475 = ORIENTED_EDGE ( 'NONE', *, *, #5018, .F. ) ;
#19476 = CARTESIAN_POINT ( 'NONE',  ( 0.4738786505895521417, -1.126875767161299002, -0.6503782676396133722 ) ) ;
#19477 = DIRECTION ( 'NONE',  ( -1.000000000000000000, -2.341930812374887555E-31, 1.664003471950578127E-31 ) ) ;
#19478 = EDGE_CURVE ( 'NONE', #19301, #507, #11543, .T. ) ;
#19479 = DIRECTION ( 'NONE',  ( -0.8660512985181130219, -0.4999551463232377868, 0.000000000000000000 ) ) ;
#19480 = EDGE_CURVE ( 'NONE', #9996, #35502, #35023, .T. ) ;
#19481 = CARTESIAN_POINT ( 'NONE',  ( 0.3270275536375774617, -1.166728321694489034, 0.5708165179803514899 ) ) ;
#19482 = ADVANCED_FACE ( 'NONE', ( #23882 ), #22566, .F. ) ;
#19483 = CIRCLE ( 'NONE', #27364, 0.04330708661417327632 ) ;
#19484 = ORIENTED_EDGE ( 'NONE', *, *, #36669, .F. ) ;
#19485 = CARTESIAN_POINT ( 'NONE',  ( -0.1508021419688997666, 0.4665171419162779665, 0.3472338286680826669 ) ) ;
#19486 = CARTESIAN_POINT ( 'NONE',  ( 0.2589322829653118996, -1.332681345024160136, 0.5684962963264375002 ) ) ;
#19487 = FACE_OUTER_BOUND ( 'NONE', #7206, .T. ) ;
#19488 = LINE ( 'NONE', #25459, #31797 ) ;
#19489 = CARTESIAN_POINT ( 'NONE',  ( 0.4486771734934781319, -1.213265135394009597, 0.7011102436740401789 ) ) ;
#19491 = DIRECTION ( 'NONE',  ( 0.000000000000000000, -0.5365213554527469286, 0.8438867430782091006 ) ) ;
#19490 = DIRECTION ( 'NONE',  ( 0.8660512985181134660, 0.4999551463232373427, 0.000000000000000000 ) ) ;
#19492 = CARTESIAN_POINT ( 'NONE',  ( 0.3611884512188844321, -1.010424417365897831, 0.6143157383772529512 ) ) ;
#19493 = ORIENTED_EDGE ( 'NONE', *, *, #3868, .T. ) ;
#19494 = COORDINATED_UNIVERSAL_TIME_OFFSET ( 0, 0, .AHEAD. ) ;
#19495 = CARTESIAN_POINT ( 'NONE',  ( 0.04445114182618741666, -1.045807839346486023, 0.7169660596555416099 ) ) ;
#19496 = VERTEX_POINT ( 'NONE', #30446 ) ;
#19497 = ORIENTED_EDGE ( 'NONE', *, *, #34585, .F. ) ;
#19498 = CARTESIAN_POINT ( 'NONE',  ( 0.04805158389062868379, -0.5422655091108523617, 0.1936128867396182673 ) ) ;
#19499 = EDGE_CURVE ( 'NONE', #28471, #31608, #34116, .T. ) ;
#19501 = CARTESIAN_POINT ( 'NONE',  ( 0.1957912801600528441, -0.6579173162935690877, 0.3309778881921752736 ) ) ;
#19500 = CARTESIAN_POINT ( 'NONE',  ( 0.06443734679387699837, -0.8352580946475701706, 0.1484956170147023191 ) ) ;
#19502 = DIRECTION ( 'NONE',  ( 0.5784884052584775560, 0.000000000000000000, 0.8156906061623510062 ) ) ;
#19503 = ORIENTED_EDGE ( 'NONE', *, *, #26093, .F. ) ;
#19504 = ORIENTED_EDGE ( 'NONE', *, *, #21203, .T. ) ;
#19505 = CARTESIAN_POINT ( 'NONE',  ( 0.3249184713931745350, -1.295165278265719699, 0.5695263721355144915 ) ) ;
#19506 = CARTESIAN_POINT ( 'NONE',  ( 0.5666678245060221553, -1.503163312012688602, 0.5681760653518421744 ) ) ;
#19507 = ORIENTED_EDGE ( 'NONE', *, *, #11400, .F. ) ;
#19508 = CARTESIAN_POINT ( 'NONE',  ( 0.1874447297040617022, -0.6903549970268514357, 0.04771061563518469439 ) ) ;
#19509 = CARTESIAN_POINT ( 'NONE',  ( 0.4787354706056592413, -1.098877335703110969, -0.6155895193482675554 ) ) ;
#19510 = FACE_OUTER_BOUND ( 'NONE', #18737, .T. ) ;
#19511 = CARTESIAN_POINT ( 'NONE',  ( 0.5931354683067489031, -1.451137063721512854, 0.6550951170253309641 ) ) ;
#19512 = CARTESIAN_POINT ( 'NONE',  ( 0.3890391140888923016, -1.644011320431554513, -0.7368878597108073913 ) ) ;
#19513 = CARTESIAN_POINT ( 'NONE',  ( 0.08393556449649998419, -1.318818014269400818, 0.4567686614275936474 ) ) ;
#19514 = CARTESIAN_POINT ( 'NONE',  ( 0.1999999999999760025, -1.903589451742650818, -0.3294945365547880534 ) ) ;
#19515 = DIRECTION ( 'NONE',  ( 0.000000000000000000, -0.8090169943749496717, -0.5877852522924700285 ) ) ;
#19516 = CONICAL_SURFACE ( 'NONE', #1789, 0.1600000000000006972, 1.047197551196598297 ) ;
#19517 = CARTESIAN_POINT ( 'NONE',  ( 0.7390121836339409445, -1.515703229308124955, 0.4860421661703527851 ) ) ;
#19518 = CARTESIAN_POINT ( 'NONE',  ( 0.3933511135026758199, -1.980813283754576659, -0.7022017663186461700 ) ) ;
#19519 = DIRECTION ( 'NONE',  ( -0.4999999999999981681, -0.6509737717187603634, 0.5711682313769322894 ) ) ;
#19520 = DIRECTION ( 'NONE',  ( 1.000000000000000000, 0.000000000000000000, 0.000000000000000000 ) ) ;
#19521 = CALENDAR_DATE ( 2026, 13, 10 ) ;
#19522 = CARTESIAN_POINT ( 'NONE',  ( -0.1450923023275435264, -0.5230583524816332375, 0.3181161673586322403 ) ) ;
#19523 = CARTESIAN_POINT ( 'NONE',  ( 0.000000000000000000, -0.05999999999999990757, 0.000000000000000000 ) ) ;
#19524 = CARTESIAN_POINT ( 'NONE',  ( 0.1835961851041346959, -0.5126270562563732813, 0.08826789480522242992 ) ) ;
#19525 = DIRECTION ( 'NONE',  ( 0.8660254037844390407, 0.3322823180458172043, -0.3736153919662543732 ) ) ;
#19526 = CARTESIAN_POINT ( 'NONE',  ( -0.2399999999999999079, -2.323257895298838971, -0.7902071827178637209 ) ) ;
#19527 = EDGE_CURVE ( 'NONE', #15591, #33383, #21396, .T. ) ;
#19528 = CARTESIAN_POINT ( 'NONE',  ( -8.537024980200822558E-17, -0.6872203660140394632, 0.1631394164078588394 ) ) ;
#19529 = DIRECTION ( 'NONE',  ( 0.000000000000000000, 0.000000000000000000, -1.000000000000000000 ) ) ;
#19530 = EDGE_CURVE ( 'NONE', #38515, #14658, #31460, .T. ) ;
#19531 = CARTESIAN_POINT ( 'NONE',  ( -2.134683096299215694E-14, -2.107936428766274073, -0.2870436526301869407 ) ) ;
#19532 = CARTESIAN_POINT ( 'NONE',  ( -19685.04193433331602, 285.7890798983738136, -1.951739244310253252 ) ) ;
#19533 = AXIS2_PLACEMENT_3D ( 'NONE', #13601, #3527, #6799 ) ;
#19534 = DIRECTION ( 'NONE',  ( -8.881784197001245421E-16, 2.361472542561082612E-16, -1.000000000000000000 ) ) ;
#19535 = ADVANCED_FACE ( 'NONE', ( #28173 ), #37839, .F. ) ;
#19536 =( REPRESENTATION_RELATIONSHIP ('NONE','NONE', #27514, #21742 ) REPRESENTATION_RELATIONSHIP_WITH_TRANSFORMATION ( #24760 )SHAPE_REPRESENTATION_RELATIONSHIP( ) );
#19537 = ORIENTED_EDGE ( 'NONE', *, *, #22315, .F. ) ;
#19538 = ORIENTED_EDGE ( 'NONE', *, *, #12547, .T. ) ;
#19539 = CARTESIAN_POINT ( 'NONE',  ( 0.05562144613422616291, -0.2542273817772364719, -0.3844451335760745159 ) ) ;
#19540 = EDGE_LOOP ( 'NONE', ( #31682, #38503 ) ) ;
#19541 = DIRECTION ( 'NONE',  ( -1.000000000000000000, -2.403560570595279103E-31, 1.725633230170969455E-31 ) ) ;
#19542 = DIRECTION ( 'NONE',  ( 0.000000000000000000, 0.000000000000000000, 1.000000000000000000 ) ) ;
#19543 = CARTESIAN_POINT ( 'NONE',  ( 0.5474171421754882028, -1.374785517832714854, 0.7657286113707925113 ) ) ;
#19545 = ORIENTED_EDGE ( 'NONE', *, *, #26009, .T. ) ;
#19544 = CARTESIAN_POINT ( 'NONE',  ( 0.4597632563371517600, -1.044138351040537982, -0.6056023639864149821 ) ) ;
#19546 = CARTESIAN_POINT ( 'NONE',  ( 0.5549519752308349485, -1.188726111083455939, 0.5935319974400015131 ) ) ;
#19547 = ORIENTED_EDGE ( 'NONE', *, *, #33826, .F. ) ;
#19548 = DIRECTION ( 'NONE',  ( -5.551115123125767911E-17, 5.007578356027541926E-16, 1.000000000000000000 ) ) ;
#19549 = ORIENTED_EDGE ( 'NONE', *, *, #38323, .F. ) ;
#19550 = CARTESIAN_POINT ( 'NONE',  ( 0.2975162600608768360, -1.656784140337124844, 0.5778434474647357044 ) ) ;
#19551 = EDGE_CURVE ( 'NONE', #37239, #6091, #12711, .T. ) ;
#19553 = CARTESIAN_POINT ( 'NONE',  ( 0.1109615456377447129, -0.9286233301030853982, 0.1297943113072267118 ) ) ;
#19552 = CARTESIAN_POINT ( 'NONE',  ( 0.6514719573431750899, -1.551752319599670971, 0.4274254745435299152 ) ) ;
#19554 = CARTESIAN_POINT ( 'NONE',  ( 0.3173964913805102928, -1.761064994645753723, 0.5509206800346062582 ) ) ;
#19555 = DIRECTION ( 'NONE',  ( -1.935058995512185017E-14, 1.000000000000000000, -2.162712994984206616E-14 ) ) ;
#19556 = EDGE_CURVE ( 'NONE', #34622, #2786, #6750, .T. ) ;
#19557 = CARTESIAN_POINT ( 'NONE',  ( 0.02125805212145761777, -1.630277869852022166, -0.3723835954392284986 ) ) ;
#19559 = EDGE_LOOP ( 'NONE', ( #11609, #18216 ) ) ;
#19558 = ORIENTED_EDGE ( 'NONE', *, *, #11756, .F. ) ;
#19560 = CARTESIAN_POINT ( 'NONE',  ( -0.08000000000000000167, -2.183180860297908144, -0.5562760292030870524 ) ) ;
#19561 = CARTESIAN_POINT ( 'NONE',  ( 0.1853397838168331091, -0.8389294303635135286, 0.1596565228427437311 ) ) ;
#19562 = CARTESIAN_POINT ( 'NONE',  ( -0.04229956186878645191, -0.008769846780144991555, -0.4686106502047107658 ) ) ;
#19563 = DIRECTION ( 'NONE',  ( -2.563099466555616810E-12, -0.9510565162951545304, -0.3090169943749443426 ) ) ;
#19564 = CARTESIAN_POINT ( 'NONE',  ( 0.3065843538909625021, -1.143276311498060194, 0.7392926086299859145 ) ) ;
#19565 = CARTESIAN_POINT ( 'NONE',  ( 0.01054817777343857940, -0.5296544771352952319, 0.1457185332388703236 ) ) ;
#19566 = CARTESIAN_POINT ( 'NONE',  ( 0.01548846960707528191, 0.3772621329472758411, 0.3651003739303370632 ) ) ;
#19567 = CARTESIAN_POINT ( 'NONE',  ( -0.1552056223146390523, 0.4812861443614941392, 0.3591723288241918666 ) ) ;
#19568 = DIRECTION ( 'NONE',  ( 0.8660512985181135770, 0.4999551463232368431, 0.000000000000000000 ) ) ;
#19569 = CARTESIAN_POINT ( 'NONE',  ( 0.4709867352971914833, -1.164672508904967652, -0.5155029497116575543 ) ) ;
#19570 = CARTESIAN_POINT ( 'NONE',  ( 0.4922290639190164963, -1.198585196483133553, -0.6250000000000000000 ) ) ;
#19571 = DIRECTION ( 'NONE',  ( 0.8339551856406566266, 0.4814266632674260027, -0.2697167333300817260 ) ) ;
#19572 = DIRECTION ( 'NONE',  ( 5.551115123125788865E-17, -3.676620095425087221E-16, -1.000000000000000000 ) ) ;
#19573 = DIRECTION ( 'NONE',  ( 0.000000000000000000, 0.000000000000000000, -1.000000000000000000 ) ) ;
#19574 = CARTESIAN_POINT ( 'NONE',  ( 0.1058691297379534685, -1.387140299098825746, 0.6606319638582223153 ) ) ;
#19575 = CARTESIAN_POINT ( 'NONE',  ( 0.4752104778612297187, -1.162234221663497546, -0.6186948529734399571 ) ) ;
#19576 = CARTESIAN_POINT ( 'NONE',  ( 0.6400160853294423191, -1.459529829645036081, -0.3976988710621562895 ) ) ;
#19577 = ADVANCED_FACE ( 'NONE', ( #25084 ), #34381, .T. ) ;
#19578 = CARTESIAN_POINT ( 'NONE',  ( -0.01896931156526107318, 0.5123785568735040874, 0.08888416637130031051 ) ) ;
#19579 = FACE_OUTER_BOUND ( 'NONE', #29853, .T. ) ;
#19580 = CARTESIAN_POINT ( 'NONE',  ( 0.4638079127942061897, -1.130673443964558267, 0.4607559890518187484 ) ) ;
#19581 = ORIENTED_EDGE ( 'NONE', *, *, #24305, .T. ) ;
#19582 = CARTESIAN_POINT ( 'NONE',  ( 0.4611535779349406061, -1.147956045046751639, -0.4054009984114392284 ) ) ;
#19583 = CYLINDRICAL_SURFACE ( 'NONE', #23038, 0.03000000000000022787 ) ;
#19584 = CARTESIAN_POINT ( 'NONE',  ( 0.5944485256643038396, -1.487068444243248022, 0.5633783733039713360 ) ) ;
#19585 = B_SPLINE_CURVE_WITH_KNOTS ( 'NONE', 3,
 ( #17891, #9057, #2487, #11930, #12145, #2288, #24710, #21619, #8848, #34143, #24906, #5951, #18512, #31065, #37430, #21818, #34347, #15638 ),
 .UNSPECIFIED., .F., .F.,
 ( 4, 2, 2, 2, 2, 2, 2, 2, 4 ),
 ( 0.0003425652276237246894, 0.001007165397454238762, 0.001671765567284752996, 0.002336365737115266798, 0.003000965906945781032, 0.003665566076776295267, 0.004330166246606809502, 0.004994766416437324170, 0.005659366586267837972 ),
 .UNSPECIFIED. ) ;
#19587 = VERTEX_POINT ( 'NONE', #9440 ) ;
#19586 = DIRECTION ( 'NONE',  ( 0.000000000000000000, 0.000000000000000000, -1.000000000000000000 ) ) ;
#19589 = VERTEX_POINT ( 'NONE', #16243 ) ;
#19588 = ORIENTED_EDGE ( 'NONE', *, *, #8723, .T. ) ;
#19590 = CARTESIAN_POINT ( 'NONE',  ( 0.6130353677484411401, -1.423293888972499976, 0.8492375987371474366 ) ) ;
#19591 =( BOUNDED_SURFACE ( )  B_SPLINE_SURFACE ( 3, 2, ( 
 ( #2900, #31484, #15450 ),
 ( #3291, #25326, #8641 ),
 ( #21214, #33750, #35190 ),
 ( #6990, #6569, #28996 ),
 ( #3506, #29209, #13581 ),
 ( #26146, #16063, #19358 ),
 ( #32482, #10081, #860 ),
 ( #38660, #1071, #25528 ),
 ( #19147, #34970, #6777 ),
 ( #19561, #28611, #22442 ),
 ( #481, #22655, #31895 ),
 ( #9683, #10480, #7373 ),
 ( #13368, #7173, #3715 ),
 ( #1261, #23046, #13155 ),
 ( #22248, #25943, #32091 ),
 ( #16267, #25720, #31684 ),
 ( #35572, #13762, #35383 ),
 ( #28805, #12976, #38467 ),
 ( #19947, #38055, #38251 ),
 ( #4308, #9869, #16874 ),
 ( #10302, #29414, #37866 ),
 ( #668, #3898, #16455 ),
 ( #34762, #22865, #19740 ),
 ( #32277, #4092, #16660 ),
 ( #9023, #8593, #33925 ),
 ( #5725, #14990, #15182 ),
 ( #21990, #27738, #37203 ),
 ( #27543, #3062, #34106 ),
 ( #18683, #34307, #21584 ),
 ( #24456, #17858, #40275 ),
 ( #30421, #9206, #31244 ),
 ( #18075, #18280, #5911 ),
 ( #27352, #25058, #34517 ),
 ( #37592, #9413, #39883 ),
 ( #18471, #12317, #15606 ),
 ( #2644, #28152, #12109 ),
 ( #24255, #16, #24675 ),
 ( #31023, #21166, #30824 ),
 ( #2844, #40064, #15394 ),
 ( #2250, #27952, #40491 ),
 ( #11892, #12501, #24872 ),
 ( #36989, #37394, #8809 ),
 ( #33697, #21778, #6116 ),
 ( #5510, #14790, #11701 ),
 ( #30628, #36778, #2453 ),
 ( #21388, #28940, #1017 ),
 ( #7121, #12920, #31841 ),
 ( #210, #22390, #3658 ),
 ( #3842, #12704, #38404 ),
 ( #16218, #22810, #25266 ) ),
 .UNSPECIFIED., .F., .F., .T. ) 
 B_SPLINE_SURFACE_WITH_KNOTS ( ( 4, 2, 2, 2, 2, 2, 2, 2, 2, 2, 2, 2, 2, 2, 2, 2, 2, 2, 2, 2, 2, 2, 2, 2, 4 ),
 ( 3, 3 ),
 ( 0.005623516400726650925, 0.005723388427146605673, 0.005773324440356582612, 0.005823260453566559552, 0.006023004506406469047, 0.006422492612086288036, 0.007221468823445924279, 0.008819421246165196765, 0.01201532609160374174, 0.01361327851432301422, 0.01521123093704228671, 0.01840713578248083168, 0.02000508820520010417, 0.02160304062791937665, 0.02240201683927901116, 0.02320099305063864914, 0.02479894547335792163, 0.02559792168471755613, 0.02639689789607719411, 0.02719587410743683209, 0.02799485031879646660, 0.02879382653015610111, 0.02959280274151573908, 0.03039177895287537706, 0.03119075516423501157 ),
 ( 0.000000000000000000, 1.000000000000000000 ),
 .UNSPECIFIED. ) 
 GEOMETRIC_REPRESENTATION_ITEM ( )  RATIONAL_B_SPLINE_SURFACE ( (
 ( 1.000000000000000000, 0.7620600366887108068, 1.000000000000000000),
 ( 1.000000000000000000, 0.7620600366887108068, 1.000000000000000000),
 ( 1.000000000000000000, 0.7620600366887158028, 1.000000000000000000),
 ( 1.000000000000000000, 0.7620600366887158028, 1.000000000000000000),
 ( 1.000000000000000000, 0.7620600366887131383, 1.000000000000000000),
 ( 1.000000000000000000, 0.7620600366887131383, 1.000000000000000000),
 ( 1.000000000000000000, 0.7620601373306783444, 1.000000000000000000),
 ( 1.000000000000000000, 0.7620613354069938339, 1.000000000000000000),
 ( 1.000000000000000000, 0.7620643364853295632, 1.000000000000000000),
 ( 1.000000000000000000, 0.7620789881756452333, 1.000000000000000000),
 ( 1.000000000000000000, 0.7620966974486877987, 1.000000000000000000),
 ( 1.000000000000000000, 0.7621581026411062831, 1.000000000000000000),
 ( 1.000000000000000000, 0.7622273003792526813, 1.000000000000000000),
 ( 1.000000000000000000, 0.7624999364063211882, 1.000000000000000000),
 ( 1.000000000000000000, 0.7627161346585163981, 1.000000000000000000),
 ( 1.000000000000000000, 0.7636758486171694171, 1.000000000000000000),
 ( 1.000000000000000000, 0.7646916490131634436, 1.000000000000000000),
 ( 1.000000000000000000, 0.7677082388477355357, 1.000000000000000000),
 ( 1.000000000000000000, 0.7689336181571234663, 1.000000000000000000),
 ( 1.000000000000000000, 0.7719590375727899412, 1.000000000000000000),
 ( 1.000000000000000000, 0.7737898733456646250, 1.000000000000000000),
 ( 1.000000000000000000, 0.7800033286103639218, 1.000000000000000000),
 ( 1.000000000000000000, 0.7857684595439522468, 1.000000000000000000),
 ( 1.000000000000000000, 0.7921457430830625146, 1.000000000000000000),
 ( 1.000000000000000000, 0.7937413855588997258, 1.000000000000000000),
 ( 1.000000000000000000, 0.7926007200054989710, 1.000000000000000000),
 ( 1.000000000000000000, 0.7894156645656090765, 1.000000000000000000),
 ( 1.000000000000000000, 0.7801802461530837896, 1.000000000000000000),
 ( 1.000000000000000000, 0.7764660701984593683, 1.000000000000000000),
 ( 1.000000000000000000, 0.7687415604991519880, 1.000000000000000000),
 ( 1.000000000000000000, 0.7647330715239430976, 1.000000000000000000),
 ( 1.000000000000000000, 0.7535529938687155482, 1.000000000000000000),
 ( 1.000000000000000000, 0.7471814462217952757, 1.000000000000000000),
 ( 1.000000000000000000, 0.7390326041316310768, 1.000000000000000000),
 ( 1.000000000000000000, 0.7365891473593165761, 1.000000000000000000),
 ( 1.000000000000000000, 0.7323603040016591903, 1.000000000000000000),
 ( 1.000000000000000000, 0.7305422876197090742, 1.000000000000000000),
 ( 1.000000000000000000, 0.7274945417416857074, 1.000000000000000000),
 ( 1.000000000000000000, 0.7263021831926989025, 1.000000000000000000),
 ( 1.000000000000000000, 0.7242655549562223571, 1.000000000000000000),
 ( 1.000000000000000000, 0.7233863612473971916, 1.000000000000000000),
 ( 1.000000000000000000, 0.7214440151235159693, 1.000000000000000000),
 ( 1.000000000000000000, 0.7204350154428263986, 1.000000000000000000),
 ( 1.000000000000000000, 0.7178948928364506932, 1.000000000000000000),
 ( 1.000000000000000000, 0.7163188285908211883, 1.000000000000000000),
 ( 1.000000000000000000, 0.7134120004149256955, 1.000000000000000000),
 ( 1.000000000000000000, 0.7119817938359319642, 1.000000000000000000),
 ( 1.000000000000000000, 0.7091286251562103349, 1.000000000000000000),
 ( 1.000000000000000000, 0.7077534102919452730, 1.000000000000000000),
 ( 1.000000000000000000, 0.7067354993702915644, 1.000000000000000000) ) ) 
 REPRESENTATION_ITEM ( '' )  SURFACE ( )  );
#19592 = ORIENTED_EDGE ( 'NONE', *, *, #11050, .F. ) ;
#19593 = DIRECTION ( 'NONE',  ( -6.162975822039149256E-32, 0.5237184928541296358, -0.8518913899333639961 ) ) ;
#19594 = B_SPLINE_CURVE_WITH_KNOTS ( 'NONE', 3,
 ( #25898, #28952, #19700, #38417 ),
 .UNSPECIFIED., .F., .F.,
 ( 4, 4 ),
 ( 0.1593719612050745749, 0.5040661668275804308 ),
 .UNSPECIFIED. ) ;
#19595 = CARTESIAN_POINT ( 'NONE',  ( 0.6106509172825420606, -1.615137135503808441, -0.5296025793890921651 ) ) ;
#19596 = EDGE_CURVE ( 'NONE', #39882, #16145, #12037, .T. ) ;
#19597 = PERSON_AND_ORGANIZATION ( #1986, #17536 ) ;
#19598 = CARTESIAN_POINT ( 'NONE',  ( -0.003741027592045935348, -0.8469330747986104635, 0.09509064842809024365 ) ) ;
#19599 = ORIENTED_EDGE ( 'NONE', *, *, #13789, .F. ) ;
#19600 = ADVANCED_FACE ( 'NONE', ( #25498 ), #6107, .F. ) ;
#19601 = CARTESIAN_POINT ( 'NONE',  ( 0.2749031748901358263, -1.001131492694471437, 0.6892845736347759100 ) ) ;
#19602 = AXIS2_PLACEMENT_3D ( 'NONE', #1551, #4792, #20056 ) ;
#19603 = CARTESIAN_POINT ( 'NONE',  ( 0.06925372759623750485, -0.5401403334181544835, 0.1535009965860707482 ) ) ;
#19604 = CARTESIAN_POINT ( 'NONE',  ( 0.1122763543019365540, -0.5767954232603237363, 0.2660804929407222796 ) ) ;
#19605 = EDGE_LOOP ( 'NONE', ( #29813, #16436, #24851, #17389, #39110 ) ) ;
#19606 = CARTESIAN_POINT ( 'NONE',  ( 0.6379677523173985509, -1.610970530585465355, -0.5598555352671841234 ) ) ;
#19607 = LINE ( 'NONE', #7221, #12638 ) ;
#19608 = CARTESIAN_POINT ( 'NONE',  ( -0.05083674528492039546, 0.04859289555129508303, 0.4711018118971380120 ) ) ;
#19609 = CARTESIAN_POINT ( 'NONE',  ( 0.3135891416034363721, -1.762206823249338639, 0.5687299299776570338 ) ) ;
#19610 = CARTESIAN_POINT ( 'NONE',  ( -0.2399999999999999079, -4.350369088120884520, -0.8413950570247814564 ) ) ;
#19611 = CARTESIAN_POINT ( 'NONE',  ( 0.5280871129044060197, -1.601407886612749021, -0.5973377142089556502 ) ) ;
#19612 = CARTESIAN_POINT ( 'NONE',  ( 0.1554726304735147280, -0.6543779252168671068, 0.4222922872362036006 ) ) ;
#19613 = CARTESIAN_POINT ( 'NONE',  ( -2.493673021531738797E-05, -0.9153651195070918734, 0.01783759308780035260 ) ) ;
#19614 = CARTESIAN_POINT ( 'NONE',  ( 0.4094665197507286747, -1.132124008075320098, 0.5707417262808780478 ) ) ;
#19615 = CARTESIAN_POINT ( 'NONE',  ( 0.4781054596003559420, -1.118034740588623954, -0.3965712557909421565 ) ) ;
#19616 = CARTESIAN_POINT ( 'NONE',  ( 0.01373823669757498131, -0.9963338274435274977, 0.5786879937691099540 ) ) ;
#19617 = CARTESIAN_POINT ( 'NONE',  ( 0.5134194225791607336, -1.118797547403455273, 0.5580923141791981346 ) ) ;
#19618 = APPROVAL_STATUS ( 'not_yet_approved' ) ;
#19619 = CARTESIAN_POINT ( 'NONE',  ( -0.3000000000000000999, -1.804235510932644004, -0.1501860188971498311 ) ) ;
#19620 = EDGE_CURVE ( 'NONE', #1885, #4225, #29807, .T. ) ;
#19621 = CARTESIAN_POINT ( 'NONE',  ( 0.6935470237484337996, -1.428868995382490237, 0.5856070495622788252 ) ) ;
#19622 = CARTESIAN_POINT ( 'NONE',  ( 0.3136119174726084147, -1.762228313981181849, 0.5679019586572930933 ) ) ;
#19623 = EDGE_LOOP ( 'NONE', ( #40325, #4171, #24661, #23400, #20646 ) ) ;
#19624 = CARTESIAN_POINT ( 'NONE',  ( -0.3000000000000000999, -3.217981293616048344, -0.2530108926800491709 ) ) ;
#19625 = FACE_OUTER_BOUND ( 'NONE', #20343, .T. ) ;
#19626 = CARTESIAN_POINT ( 'NONE',  ( -0.08000000000000000167, -1.669835911085076674, -0.2333336242928227278 ) ) ;
#19627 = VERTEX_POINT ( 'NONE', #32667 ) ;
#19628 = CARTESIAN_POINT ( 'NONE',  ( 0.05579155178881651383, -1.335540925555324332, 0.3667417262808778111 ) ) ;
#19629 = CARTESIAN_POINT ( 'NONE',  ( 0.6027116599735458102, -1.274749097762014616, 0.7879118535713135474 ) ) ;
#19631 = ORIENTED_EDGE ( 'NONE', *, *, #39716, .T. ) ;
#19630 = EDGE_LOOP ( 'NONE', ( #18667, #29531, #40009, #23491 ) ) ;
#19632 = CARTESIAN_POINT ( 'NONE',  ( -0.2746410161513770931, -2.861028283584748699, -0.4103205306338890690 ) ) ;
#19633 = ORIENTED_EDGE ( 'NONE', *, *, #8735, .T. ) ;
#19634 = FACE_OUTER_BOUND ( 'NONE', #34232, .T. ) ;
#19635 = PRODUCT ( 'pulley bushing cover', 'pulley bushing cover', '', ( #4055 ) ) ;
#19636 = FACE_OUTER_BOUND ( 'NONE', #2070, .T. ) ;
#19637 = DIRECTION ( 'NONE',  ( -1.000000000000000000, -0.000000000000000000, -0.000000000000000000 ) ) ;
#19638 = VERTEX_POINT ( 'NONE', #23444 ) ;
#19639 = CARTESIAN_POINT ( 'NONE',  ( 0.1718750000000003608, -0.4565580874172214809, 0.1856949347217508317 ) ) ;
#19640 = CARTESIAN_POINT ( 'NONE',  ( 0.2472017802686538868, -0.9017822974133011815, 0.7202505716065562558 ) ) ;
#19641 = CARTESIAN_POINT ( 'NONE',  ( 0.007466387553240696855, -0.5173474752212334771, 0.4375680074810365250 ) ) ;
#19642 = CARTESIAN_POINT ( 'NONE',  ( 0.4697186253659513255, -1.557987743023917071, 0.5732339134589082841 ) ) ;
#19644 = CARTESIAN_POINT ( 'NONE',  ( -0.1210148435730238475, -0.5061394519557863569, 0.3122829191279349881 ) ) ;
#19643 = CARTESIAN_POINT ( 'NONE',  ( 0.5040251875448504837, -1.584373116627600275, -0.4836906369935438654 ) ) ;
#19645 = CARTESIAN_POINT ( 'NONE',  ( 0.2188631975425677223, -0.9478063358918615844, 0.4590906284417705097 ) ) ;
#19646 = ORIENTED_EDGE ( 'NONE', *, *, #40100, .T. ) ;
#19647 = ORIENTED_EDGE ( 'NONE', *, *, #15688, .T. ) ;
#19648 = EDGE_CURVE ( 'NONE', #14789, #23080, #7147, .T. ) ;
#19649 = CARTESIAN_POINT ( 'NONE',  ( 0.6638313581005879094, -1.459541049076493735, -0.6171250890061030780 ) ) ;
#19650 = CARTESIAN_POINT ( 'NONE',  ( 0.2524564437961140939, -1.572036326075024526, -0.3190288371789616328 ) ) ;
#19651 = CARTESIAN_POINT ( 'NONE',  ( -0.05615703521555169553, 0.2783003116137218180, -0.3655156233916866948 ) ) ;
#19652 = DIRECTION ( 'NONE',  ( -1.000000000000000000, 0.000000000000000000, -5.691349986800505477E-16 ) ) ;
#19653 = CYLINDRICAL_SURFACE ( 'NONE', #4330, 0.08749999999977552123 ) ;
#19654 = CARTESIAN_POINT ( 'NONE',  ( 0.4381829047093346863, -1.020301330954181518, 0.7847444992166355826 ) ) ;
#19655 = DIRECTION ( 'NONE',  ( 1.000000000000000000, 0.000000000000000000, 0.000000000000000000 ) ) ;
#19656 = CARTESIAN_POINT ( 'NONE',  ( 0.008016308253612618520, -0.8914097450206520667, 0.5066122301535544992 ) ) ;
#19657 = CARTESIAN_POINT ( 'NONE',  ( 0.05279905671745396128, 0.4561941007107730428, -0.1063003320160303133 ) ) ;
#19658 = FACE_OUTER_BOUND ( 'NONE', #26636, .T. ) ;
#19659 = CARTESIAN_POINT ( 'NONE',  ( 0.3575911698065382116, -1.086899798299411302, 0.7623387881491152651 ) ) ;
#19660 = CARTESIAN_POINT ( 'NONE',  ( 0.4738546087217606062, -1.652018268363231845, -0.3975985852014427002 ) ) ;
#19661 = CARTESIAN_POINT ( 'NONE',  ( 0.1798596100760564143, -1.237890289190527904, -0.6192247734168379036 ) ) ;
#19662 = EDGE_LOOP ( 'NONE', ( #16149, #18715, #19558, #8418, #12974 ) ) ;
#19663 = CARTESIAN_POINT ( 'NONE',  ( 0.4806378395295556882, -1.105637800341302102, -0.6194292131661300882 ) ) ;
#19664 = CARTESIAN_POINT ( 'NONE',  ( 0.3972854997516396258, -1.646912688252536006, -0.3935780560914288184 ) ) ;
#19665 = DIRECTION ( 'NONE',  ( 8.881784197001246407E-16, -2.361472542561082612E-16, 1.000000000000000000 ) ) ;
#19666 = CARTESIAN_POINT ( 'NONE',  ( 0.3549243309889831277, -1.132073402205351131, 0.6013745090441735552 ) ) ;
#19667 = CARTESIAN_POINT ( 'NONE',  ( 0.05555397280955033656, -0.8368505189396917565, 0.1801077275890973495 ) ) ;
#19668 = VERTEX_POINT ( 'NONE', #35539 ) ;
#19669 = CARTESIAN_POINT ( 'NONE',  ( -0.1646293987946935988, 0.5114631127588012971, 0.3384789781300959755 ) ) ;
#19670 = CARTESIAN_POINT ( 'NONE',  ( 0.000000000000000000, 0.3931478764542372661, 0.2416960844521746365 ) ) ;
#19671 = CARTESIAN_POINT ( 'NONE',  ( 0.4858726280787338259, -1.662107068784129504, 0.5433456355363511792 ) ) ;
#19672 = CARTESIAN_POINT ( 'NONE',  ( 0.1842694382075218962, -1.260909057897439789, -0.7430131060672421350 ) ) ;
#19673 = CARTESIAN_POINT ( 'NONE',  ( 0.4568688193648175466, -1.223409423111213368, 0.6787920684031271135 ) ) ;
#19675 = CARTESIAN_POINT ( 'NONE',  ( 0.3143066584002391917, -1.762151917645995880, 0.5150212063305845689 ) ) ;
#19674 = CARTESIAN_POINT ( 'NONE',  ( 0.02953079040095687308, 0.09152108205202803826, 0.5223162075576412988 ) ) ;
#19676 = CARTESIAN_POINT ( 'NONE',  ( 0.4678749147552476173, -1.068959612060700115, 0.6229948197350051453 ) ) ;
#19677 = ORIENTED_EDGE ( 'NONE', *, *, #39589, .T. ) ;
#19678 = DATE_AND_TIME ( #22981, #16802 ) ;
#19679 = LINE ( 'NONE', #32214, #40147 ) ;
#19680 = ORIENTED_EDGE ( 'NONE', *, *, #23081, .T. ) ;
#19681 = CARTESIAN_POINT ( 'NONE',  ( 0.2690476586069101561, -1.239345786690793316, 0.8867825711151151591 ) ) ;
#19683 = CARTESIAN_POINT ( 'NONE',  ( 0.2031833423866013510, -0.6661378789744705209, 0.3462199175563250297 ) ) ;
#19682 = CARTESIAN_POINT ( 'NONE',  ( 0.08702963661190515898, -0.7199049649723878730, 0.02678892191856024202 ) ) ;
#19684 = FACE_BOUND ( 'NONE', #27892, .T. ) ;
#19685 = ORIENTED_EDGE ( 'NONE', *, *, #39339, .F. ) ;
#19686 = CARTESIAN_POINT ( 'NONE',  ( 0.3696611067744549062, -1.269317993774967235, 0.5790240320825449372 ) ) ;
#19687 = EDGE_CURVE ( 'NONE', #35558, #21667, #4157, .T. ) ;
#19688 = ADVANCED_FACE ( 'NONE', ( #4472 ), #39630, .T. ) ;
#19689 = CARTESIAN_POINT ( 'NONE',  ( 0.3249529450033704081, -1.071926163521130793, 0.7974727990734679084 ) ) ;
#19690 = VERTEX_POINT ( 'NONE', #7344 ) ;
#19691 = CARTESIAN_POINT ( 'NONE',  ( 0.5376330384393707140, -1.631732069091240689, -0.4370647559278275085 ) ) ;
#19692 = CARTESIAN_POINT ( 'NONE',  ( 0.1961868571575540177, -1.348426346360368955, -0.3372674651588674632 ) ) ;
#19693 = ADVANCED_FACE ( 'NONE', ( #1234 ), #36149, .F. ) ;
#19694 = FACE_OUTER_BOUND ( 'NONE', #28879, .T. ) ;
#19695 = FACE_OUTER_BOUND ( 'NONE', #3088, .T. ) ;
#19696 = EDGE_CURVE ( 'NONE', #10838, #16489, #17959, .T. ) ;
#19697 = DIRECTION ( 'NONE',  ( 0.000000000000000000, -0.3563057211773426602, -0.9343694307158671997 ) ) ;
#19698 = CARTESIAN_POINT ( 'NONE',  ( 0.1202810120457312587, -1.413329640664104714, 0.4915196355915492643 ) ) ;
#19699 = ADVANCED_FACE ( 'NONE', ( #26300 ), #10344, .T. ) ;
#19700 = CARTESIAN_POINT ( 'NONE',  ( 0.5140726076881749762, -1.533129850232453073, 0.5729469988205835307 ) ) ;
#19701 = CARTESIAN_POINT ( 'NONE',  ( 0.3890272469822507184, -1.925427499875787651, -0.6972876674577032086 ) ) ;
#19702 = CARTESIAN_POINT ( 'NONE',  ( 2.048885995248197414E-16, 0.2900000000000004796, -5.122214988120493288E-16 ) ) ;
#19703 = CARTESIAN_POINT ( 'NONE',  ( 0.3582292064121807007, -1.745863530688037013, -0.4681685754184095605 ) ) ;
#19704 = COORDINATED_UNIVERSAL_TIME_OFFSET ( 0, 0, .AHEAD. ) ;
#19705 = LINE ( 'NONE', #16236, #8764 ) ;
#19706 = CARTESIAN_POINT ( 'NONE',  ( 0.1742110732111710192, -1.381820364732997630, 0.4951799650135631503 ) ) ;
#19707 = CARTESIAN_POINT ( 'NONE',  ( -0.1212602504510426477, -0.5073146174426373944, 0.3063129689661391875 ) ) ;
#19708 = DIRECTION ( 'NONE',  ( 0.000000000000000000, 0.000000000000000000, -1.000000000000000000 ) ) ;
#19709 = CARTESIAN_POINT ( 'NONE',  ( 0.1676694287369189240, -1.385544946528693089, 0.5182417262812420988 ) ) ;
#19710 = EDGE_CURVE ( 'NONE', #34558, #12973, #19920, .T. ) ;
#19711 = APPLIED_PERSON_AND_ORGANIZATION_ASSIGNMENT ( #8513, #36901, ( #17711 ) ) ;
#19712 = CARTESIAN_POINT ( 'NONE',  ( 0.2510700677566410910, -1.656657411791499168, 0.6264822711378978948 ) ) ;
#19713 = CARTESIAN_POINT ( 'NONE',  ( 3.174100321265008938E-05, -0.6549929327938652790, -0.1017423426240838952 ) ) ;
#19714 = DIRECTION ( 'NONE',  ( -1.387778780781449423E-15, -6.590151126658397631E-16, -1.000000000000000000 ) ) ;
#19715 = CARTESIAN_POINT ( 'NONE',  ( 0.5368059768295552203, -1.632287305134593858, -0.5948306701282568554 ) ) ;
#19716 = DIRECTION ( 'NONE',  ( 0.000000000000000000, 0.000000000000000000, -1.000000000000000000 ) ) ;
#19717 = EDGE_LOOP ( 'NONE', ( #18307, #6774, #24665, #32247 ) ) ;
#19718 = EDGE_LOOP ( 'NONE', ( #29908, #15534, #33184, #27954 ) ) ;
#19719 = DIRECTION ( 'NONE',  ( -1.000000000000000000, 0.000000000000000000, 0.000000000000000000 ) ) ;
#19720 = EDGE_LOOP ( 'NONE', ( #26248, #16688, #26171, #12292 ) ) ;
#19721 = DIRECTION ( 'NONE',  ( -0.2147743920926257211, -0.9766636885342073748, -1.901964324923283986E-17 ) ) ;
#19722 = CARTESIAN_POINT ( 'NONE',  ( -0.02000000000000000042, -2.183180860297908144, -0.4937760292030871079 ) ) ;
#19723 = CARTESIAN_POINT ( 'NONE',  ( 0.4754990182428835421, -1.260416879592009209, 0.7839229098787490191 ) ) ;
#19724 = CIRCLE ( 'NONE', #2003, 0.1600000000000000588 ) ;
#19726 = EDGE_LOOP ( 'NONE', ( #7583, #31333, #4690, #25365 ) ) ;
#19725 = DIRECTION ( 'NONE',  ( -1.000000000000000000, -2.465190328815662439E-32, 0.000000000000000000 ) ) ;
#19727 = CARTESIAN_POINT ( 'NONE',  ( 0.5440395270977919084, -1.170651503450800268, 0.6371399293509031336 ) ) ;
#19728 = CARTESIAN_POINT ( 'NONE',  ( 0.3324871086615489024, -1.659137217475706860, -0.6399689536651946842 ) ) ;
#19729 = EDGE_LOOP ( 'NONE', ( #30660, #30919, #25425, #6084 ) ) ;
#19730 = CARTESIAN_POINT ( 'NONE',  ( 0.5305894487643406654, -1.569038067003539316, -0.5473203437262895710 ) ) ;
#19731 = VERTEX_POINT ( 'NONE', #11069 ) ;
#19732 = TOROIDAL_SURFACE ( 'NONE', #34840, 0.1333070866141732314, 0.02999999999999999889 ) ;
#19733 = CARTESIAN_POINT ( 'NONE',  ( 0.02321681876055776625, -0.5326713631696793350, 0.1642138666653286949 ) ) ;
#19735 = CARTESIAN_POINT ( 'NONE',  ( 0.1114269046118611800, -0.9037280467778343596, 0.03884140610461449955 ) ) ;
#19734 = FACE_OUTER_BOUND ( 'NONE', #25086, .T. ) ;
#19736 = LINE ( 'NONE', #29205, #33888 ) ;
#19737 = B_SPLINE_CURVE_WITH_KNOTS ( 'NONE', 3,
 ( #28610, #9868, #31077, #9067, #15845, #15449, #5963, #3713, #479, #15647 ),
 .UNSPECIFIED., .F., .F.,
 ( 4, 2, 2, 2, 4 ),
 ( -2.424788074806314843E-05, 0.002669425500014234020, 0.004016262190395372689, 0.004689680535585941806, 0.005363098880776510057 ),
 .UNSPECIFIED. ) ;
#19738 = ORIENTED_EDGE ( 'NONE', *, *, #24783, .T. ) ;
#19739 = CARTESIAN_POINT ( 'NONE',  ( 0.3211368908745024231, -1.297361866234852279, 0.5668322337678470824 ) ) ;
#19740 = CARTESIAN_POINT ( 'NONE',  ( 0.2048707271511035211, -0.9816035136465564026, 0.5387368206152267636 ) ) ;
#19741 = DIRECTION ( 'NONE',  ( 1.000000000000000000, 6.779273404243070203E-32, 4.314083075427408311E-32 ) ) ;
#19742 = EDGE_CURVE ( 'NONE', #15898, #16107, #31100, .T. ) ;
#19743 = FACE_OUTER_BOUND ( 'NONE', #21302, .T. ) ;
#19744 = CARTESIAN_POINT ( 'NONE',  ( 0.4035173398106813303, -1.183714493217256525, 0.6980592135633917339 ) ) ;
#19745 = CARTESIAN_POINT ( 'NONE',  ( 0.08149770795327589135, -0.9555731122693961188, 0.8005031696937210395 ) ) ;
#19746 = ADVANCED_FACE ( 'NONE', ( #35753 ), #31767, .F. ) ;
#19747 = CARTESIAN_POINT ( 'NONE',  ( 0.4621675984227249789, -1.110867290327286261, 0.5635151220948720896 ) ) ;
#19748 = EDGE_CURVE ( 'NONE', #14090, #14891, #23631, .T. ) ;
#19749 = CARTESIAN_POINT ( 'NONE',  ( 0.4470762725457128051, -1.224665299296468168, 0.5557458780183651692 ) ) ;
#19750 = CARTESIAN_POINT ( 'NONE',  ( 0.6610220512682888350, -1.531173313024449145, 0.4235823276999062248 ) ) ;
#19751 = FACE_OUTER_BOUND ( 'NONE', #39751, .T. ) ;
#19752 = CARTESIAN_POINT ( 'NONE',  ( -0.02000000000000000042, -1.717917452254872357, -0.2877234685858645613 ) ) ;
#19753 = PERSON_AND_ORGANIZATION_ROLE ( 'classification_officer' ) ;
#19754 = CIRCLE ( 'NONE', #12529, 0.06000000000000021289 ) ;
#19755 = CARTESIAN_POINT ( 'NONE',  ( 0.04946426091936632213, -0.3082279967728515091, 0.3644356914998804764 ) ) ;
#19756 = CARTESIAN_POINT ( 'NONE',  ( 0.1798968830709493649, -1.237954855633865536, -0.4125659523519146221 ) ) ;
#19757 = CARTESIAN_POINT ( 'NONE',  ( 0.1180724459482614536, -1.405395761025577173, 0.6161712495310950333 ) ) ;
#19758 = EDGE_CURVE ( 'NONE', #4083, #28686, #32401, .T. ) ;
#19759 = CARTESIAN_POINT ( 'NONE',  ( 0.4823721729254818458, -1.674185189763958359, 0.4975600008975328281 ) ) ;
#19760 = CARTESIAN_POINT ( 'NONE',  ( 0.3573610978452740894, -1.882114898915002055, -0.4864032973032175744 ) ) ;
#19761 = CONICAL_SURFACE ( 'NONE', #6614, 0.5515209409081860414, 1.047197551196597409 ) ;
#19762 = CARTESIAN_POINT ( 'NONE',  ( 0.3080579051995495088, -1.757131687391454644, 0.6134035025875401725 ) ) ;
#19763 = CARTESIAN_POINT ( 'NONE',  ( 0.6635321361362904735, -1.532953086552128141, 0.4286296017635089495 ) ) ;
#19764 = EDGE_LOOP ( 'NONE', ( #25812, #2995, #15676, #29154 ) ) ;
#19765 = DIRECTION ( 'NONE',  ( -1.000000000000000000, -2.341930812374887555E-31, 1.664003471950578127E-31 ) ) ;
#19766 = ORIENTED_EDGE ( 'NONE', *, *, #27146, .F. ) ;
#19767 = CARTESIAN_POINT ( 'NONE',  ( -0.05464101615137786222, -2.196071624283071788, -0.8624000883860228894 ) ) ;
#19768 = CARTESIAN_POINT ( 'NONE',  ( 0.1891999079356043167, -0.7494799771669461430, 0.5572005692116146491 ) ) ;
#19770 = ORIENTED_EDGE ( 'NONE', *, *, #36298, .T. ) ;
#19769 = DIRECTION ( 'NONE',  ( -1.000000000000000000, -2.280301054154495132E-31, 1.664003471950577689E-31 ) ) ;
#19772 = EDGE_LOOP ( 'NONE', ( #6149, #7683, #35000, #1359, #9382, #26782 ) ) ;
#19771 = ORIENTED_EDGE ( 'NONE', *, *, #25559, .T. ) ;
#19773 = DIRECTION ( 'NONE',  ( 0.000000000000000000, 0.000000000000000000, -1.000000000000000000 ) ) ;
#19774 = ORIENTED_EDGE ( 'NONE', *, *, #7210, .F. ) ;
#19775 = VERTEX_POINT ( 'NONE', #32856 ) ;
#19776 = CARTESIAN_POINT ( 'NONE',  ( 0.06954796871655651025, -1.315582234632707515, 0.5182417262812430980 ) ) ;
#19777 = CARTESIAN_POINT ( 'NONE',  ( 0.6277051948539001947, -1.616894912232479831, -0.5046519086154381828 ) ) ;
#19778 = CONTEXT_DEPENDENT_SHAPE_REPRESENTATION ( #25839, #26557 ) ;
#19779 = CIRCLE ( 'NONE', #35540, 0.1400000000000009570 ) ;
#19780 = DIRECTION ( 'NONE',  ( 1.000000000000000000, -0.000000000000000000, -0.000000000000000000 ) ) ;
#19781 = ORIENTED_EDGE ( 'NONE', *, *, #35512, .T. ) ;
#19782 = CARTESIAN_POINT ( 'NONE',  ( 0.1672826910485447904, -0.8876356709551983526, 0.5561758849923722492 ) ) ;
#19783 = EDGE_CURVE ( 'NONE', #14101, #37863, #30451, .T. ) ;
#19784 = CARTESIAN_POINT ( 'NONE',  ( 0.4170376818810827002, -1.621705073591293678, -0.3781026430796730065 ) ) ;
#19785 = CIRCLE ( 'NONE', #17169, 0.9087847906030154244 ) ;
#19786 = CARTESIAN_POINT ( 'NONE',  ( 0.3315238338797135698, -1.140207891145209596, 0.8255108127574939392 ) ) ;
#19787 = ORIENTED_EDGE ( 'NONE', *, *, #33417, .T. ) ;
#19788 = CARTESIAN_POINT ( 'NONE',  ( 0.1768208203293339109, -0.4924928695182538840, 0.1890629170402937931 ) ) ;
#19789 = DIRECTION ( 'NONE',  ( 1.000000000000000000, -0.000000000000000000, -0.000000000000000000 ) ) ;
#19790 = CONICAL_SURFACE ( 'NONE', #11888, 0.1500000000000009936, 1.047197551196599630 ) ;
#19791 = CYLINDRICAL_SURFACE ( 'NONE', #29149, 0.01500000000000004802 ) ;
#19792 = AXIS2_PLACEMENT_3D ( 'NONE', #23100, #38909, #4744 ) ;
#19793 = EDGE_CURVE ( 'NONE', #23947, #28983, #29121, .T. ) ;
#19794 = CARTESIAN_POINT ( 'NONE',  ( 0.4042633028796379646, -1.711240744074478570, 0.4220515681607872605 ) ) ;
#19795 = CARTESIAN_POINT ( 'NONE',  ( 0.6981352535869485010, -1.438782441872884732, 0.5605301977290049198 ) ) ;
#19796 = CARTESIAN_POINT ( 'NONE',  ( 0.5314857169285645000, -1.600448699198730562, -0.5913921701293719524 ) ) ;
#19797 = CARTESIAN_POINT ( 'NONE',  ( -0.8248651029816859159, -5.463695987328526437E-16, 0.000000000000000000 ) ) ;
#19798 = CARTESIAN_POINT ( 'NONE',  ( 0.6089969234689213140, -1.479027626961725295, 0.5722973471840744342 ) ) ;
#19799 = CARTESIAN_POINT ( 'NONE',  ( -1.458240315477721432E-08, -0.7217202255946222333, -0.1135441531130386150 ) ) ;
#19800 =( NAMED_UNIT ( * ) SI_UNIT ( $, .STERADIAN. ) SOLID_ANGLE_UNIT ( ) );
#19801 = CARTESIAN_POINT ( 'NONE',  ( 0.4245907089628130904, -1.708467588870119513, 0.4184861834727511276 ) ) ;
#19802 = AXIS2_PLACEMENT_3D ( 'NONE', #13901, #26474, #29147 ) ;
#19803 = CARTESIAN_POINT ( 'NONE',  ( 0.4511230681663170872, -1.093032438009407192, -0.6231826621457485782 ) ) ;
#19804 = CARTESIAN_POINT ( 'NONE',  ( -0.002083146443013340551, -0.8967360763018591419, 0.1296726476164832831 ) ) ;
#19805 = CARTESIAN_POINT ( 'NONE',  ( 0.1845475678902450123, -0.7902170579836453879, 0.1696330687313138408 ) ) ;
#19806 = PERSON_AND_ORGANIZATION ( #28500, #32463 ) ;
#19807 = EDGE_CURVE ( 'NONE', #38965, #19638, #2427, .T. ) ;
#19808 = EDGE_CURVE ( 'NONE', #40614, #8526, #40281, .T. ) ;
#19809 = AXIS2_PLACEMENT_3D ( 'NONE', #30763, #11645, #30961 ) ;
#19810 = EDGE_CURVE ( 'NONE', #24607, #36909, #16930, .T. ) ;
#19811 = CYLINDRICAL_SURFACE ( 'NONE', #1781, 0.06250000000000001388 ) ;
#19812 = CARTESIAN_POINT ( 'NONE',  ( 0.4123050674383867409, -1.729694699482061671, -0.5155029497116575543 ) ) ;
#19813 = AXIS2_PLACEMENT_3D ( 'NONE', #37948, #3185, #22140 ) ;
#19814 =( BOUNDED_SURFACE ( )  B_SPLINE_SURFACE ( 3, 2, ( 
 ( #11364, #30702, #21245 ),
 ( #21035, #39530, #30895 ),
 ( #27613, #11581, #5589 ),
 ( #2323, #24328, #40142 ),
 ( #27817, #20639, #23934 ),
 ( #27214, #1919, #24144 ),
 ( #2522, #18347, #14865 ),
 ( #21461, #17933, #24535 ),
 ( #30278, #14644, #2107 ),
 ( #12185, #8279, #20848 ),
 ( #27425, #33556, #14437 ),
 ( #40352, #5790, #24744 ),
 ( #36853, #30091, #30493 ),
 ( #33371, #18148, #5370 ),
 ( #8666, #11970, #33176 ),
 ( #4980, #5175, #37067 ),
 ( #27002, #8474, #39950 ),
 ( #2714, #11768, #17727 ) ),
 .UNSPECIFIED., .F., .F., .F. ) 
 B_SPLINE_SURFACE_WITH_KNOTS ( ( 4, 2, 2, 2, 2, 2, 2, 2, 4 ),
 ( 3, 3 ),
 ( -0.001532620576208852279, -0.0007637936630077648160, 5.033250193322538930E-06, 0.0007738601633944098938, 0.001542687076595497357, 0.002311513989796584820, 0.003080340902997672284, 0.003849167816198759747, 0.004617994729399847210 ),
 ( 0.000000000000000000, 1.000000000000000000 ),
 .UNSPECIFIED. ) 
 GEOMETRIC_REPRESENTATION_ITEM ( )  RATIONAL_B_SPLINE_SURFACE ( (
 ( 1.000000000000000000, 0.7283825911960450927, 1.000000000000000000),
 ( 1.000000000000000000, 0.7404385082114955940, 1.000000000000000000),
 ( 1.000000000000000000, 0.7521504257737200438, 1.000000000000000000),
 ( 1.000000000000000000, 0.7744497410762684053, 1.000000000000000000),
 ( 1.000000000000000000, 0.7845654757373705657, 1.000000000000000000),
 ( 1.000000000000000000, 0.8022083990892434624, 1.000000000000000000),
 ( 1.000000000000000000, 0.8094167424699041380, 1.000000000000000000),
 ( 1.000000000000000000, 0.8194491993616890291, 1.000000000000000000),
 ( 1.000000000000000000, 0.8220634900780797727, 1.000000000000000000),
 ( 1.000000000000000000, 0.8220705070823152161, 1.000000000000000000),
 ( 1.000000000000000000, 0.8194468812479983599, 1.000000000000000000),
 ( 1.000000000000000000, 0.8094220769840453356, 1.000000000000000000),
 ( 1.000000000000000000, 0.8022659121985590280, 1.000000000000000000),
 ( 1.000000000000000000, 0.7845681159035412522, 1.000000000000000000),
 ( 1.000000000000000000, 0.7744426415186608237, 1.000000000000000000),
 ( 1.000000000000000000, 0.7522890290927356505, 1.000000000000000000),
 ( 1.000000000000000000, 0.7403540167216396961, 1.000000000000000000),
 ( 1.000000000000000000, 0.7283825911960196686, 1.000000000000000000) ) ) 
 REPRESENTATION_ITEM ( '' )  SURFACE ( )  );
#19815 = AXIS2_PLACEMENT_3D ( 'NONE', #22260, #22452, #24731 ) ;
#19816 = ORIENTED_EDGE ( 'NONE', *, *, #26622, .T. ) ;
#19817 = CARTESIAN_POINT ( 'NONE',  ( 0.3999999999999787059, -2.097675824466503691, -0.7286991843995640483 ) ) ;
#19818 = CARTESIAN_POINT ( 'NONE',  ( 0.002296899787676456861, -0.5199047658870934452, 0.1480254331800099632 ) ) ;
#19819 = CIRCLE ( 'NONE', #15890, 0.5400000000000015898 ) ;
#19820 = CARTESIAN_POINT ( 'NONE',  ( 0.2764337282391428618, -1.207704344519209938, -0.5166151207188711680 ) ) ;
#19821 = VERTEX_POINT ( 'NONE', #26908 ) ;
#19822 = CARTESIAN_POINT ( 'NONE',  ( 0.2322138788700108258, -1.233113307957229177, 0.3157417262808777658 ) ) ;
#19823 = CARTESIAN_POINT ( 'NONE',  ( 0.6448460108028967186, -1.341977515531164844, 0.7437914968157772755 ) ) ;
#19825 = EDGE_LOOP ( 'NONE', ( #40200, #7099, #3832, #20425 ) ) ;
#19824 = ORIENTED_EDGE ( 'NONE', *, *, #7133, .F. ) ;
#19826 = DIRECTION ( 'NONE',  ( -3.543711097672501380E-32, -0.8983234858819668656, -0.4393346272636287630 ) ) ;
#19827 = EDGE_LOOP ( 'NONE', ( #30606, #21386, #32767, #19092 ) ) ;
#19828 = CARTESIAN_POINT ( 'NONE',  ( 0.03309058451312588828, -0.08822157290689926212, -0.5132714794726492835 ) ) ;
#19829 = DIRECTION ( 'NONE',  ( 0.000000000000000000, -0.3090169943749502823, -0.9510565162951527540 ) ) ;
#19830 = CARTESIAN_POINT ( 'NONE',  ( -0.08000000000000000167, -2.183180860297908144, -0.4937760292030871079 ) ) ;
#19831 = ORIENTED_EDGE ( 'NONE', *, *, #26502, .F. ) ;
#19832 = VECTOR ( 'NONE', #35071, 39.37007874015748143 ) ;
#19833 = CARTESIAN_POINT ( 'NONE',  ( 0.6470938791149390967, -1.584427830297316264, 0.8325270323136898520 ) ) ;
#19834 = CARTESIAN_POINT ( 'NONE',  ( 0.08886448817286804469, -0.6447356382513865780, 0.1659436972385093245 ) ) ;
#19835 = CARTESIAN_POINT ( 'NONE',  ( 0.08857948564287103366, -0.8409399715488701244, 0.8385396921228991385 ) ) ;
#19836 = CARTESIAN_POINT ( 'NONE',  ( 0.1369971865350032569, -0.7548644416457152007, 0.5821855080690007123 ) ) ;
#19838 = DIRECTION ( 'NONE',  ( 0.000000000000000000, 0.9510565162951547524, 0.3090169943749436210 ) ) ;
#19837 = CARTESIAN_POINT ( 'NONE',  ( 0.1137578413796589971, -0.5878045126424163991, -0.07386395797409718578 ) ) ;
#19839 = CARTESIAN_POINT ( 'NONE',  ( 0.2987922164586632179, -1.070374400135252646, 0.6380231227814501249 ) ) ;
#19840 = VERTEX_POINT ( 'NONE', #4873 ) ;
#19841 = ORIENTED_EDGE ( 'NONE', *, *, #23252, .T. ) ;
#19842 = AXIS2_PLACEMENT_3D ( 'NONE', #22204, #19100, #16015 ) ;
#19843 = EDGE_CURVE ( 'NONE', #7871, #10115, #24430, .T. ) ;
#19844 = B_SPLINE_CURVE_WITH_KNOTS ( 'NONE', 3,
 ( #15088, #27644, #14896, #30317, #20882, #5211 ),
 .UNSPECIFIED., .F., .F.,
 ( 4, 2, 4 ),
 ( 0.0004700531327201783335, 0.0008837629426271082726, 0.001297472752534038374 ),
 .UNSPECIFIED. ) ;
#19845 = CARTESIAN_POINT ( 'NONE',  ( 0.2161879510971927432, -1.277123080371499242, -0.3144976166544468099 ) ) ;
#19846 = B_SPLINE_CURVE_WITH_KNOTS ( 'NONE', 3,
 ( #31730, #3150, #38298, #6227, #22291, #37911, #38098, #6610, #711, #34806, #19191, #37699, #28658, #16119, #22705, #32139, #22488, #6420, #9522, #22098, #18988, #28440, #35013, #314 ),
 .UNSPECIFIED., .F., .F.,
 ( 4, 2, 2, 2, 2, 2, 2, 2, 2, 2, 2, 4 ),
 ( 0.000000000000000000, 0.0009274901291892772215, 0.001854980258378554443, 0.002782470387567831556, 0.003709960516757108886, 0.004637450645946387950, 0.005101195710541035939, 0.005564940775135683929, 0.006028685839730332785, 0.006492430904324981641, 0.006956175968919630498, 0.007419921033514278487 ),
 .UNSPECIFIED. ) ;
#19847 = CARTESIAN_POINT ( 'NONE',  ( 0.2146879954751789998, -0.5662268874561233734, 0.4488732130404408105 ) ) ;
#19848 = EDGE_CURVE ( 'NONE', #27128, #7581, #6124, .T. ) ;
#19849 = DIRECTION ( 'NONE',  ( 0.8660512985181132439, 0.4999551463232379533, 0.000000000000000000 ) ) ;
#19850 = AXIS2_PLACEMENT_3D ( 'NONE', #29253, #35230, #32730 ) ;
#19851 = TOROIDAL_SURFACE ( 'NONE', #33636, 0.05000000000000000971, 0.2000000000000000111 ) ;
#19852 = CARTESIAN_POINT ( 'NONE',  ( -0.05138886601528081660, -0.4553812863296833879, -0.1245405308888577478 ) ) ;
#19853 = AXIS2_PLACEMENT_3D ( 'NONE', #10332, #698, #16487 ) ;
#19854 = CARTESIAN_POINT ( 'NONE',  ( 0.07340065495868035306, -1.319686002187802520, 0.5021441993942140636 ) ) ;
#19855 = DIRECTION ( 'NONE',  ( -0.8660512985181131329, -0.4999551463232376758, 0.000000000000000000 ) ) ;
#19856 = CARTESIAN_POINT ( 'NONE',  ( 0.2889710164712426255, -0.7847915145120791802, 0.6224945701162477585 ) ) ;
#19857 = CARTESIAN_POINT ( 'NONE',  ( 0.5382276305428630447, -1.161165069882498013, 0.5699001961276483064 ) ) ;
#19858 = CARTESIAN_POINT ( 'NONE',  ( -0.002288348195189989116, -0.8555288688122629770, 0.1457185332388701293 ) ) ;
#19859 = CARTESIAN_POINT ( 'NONE',  ( 0.03478489236951045477, 0.5086709597375891345, -0.08927530733453492573 ) ) ;
#19860 = CARTESIAN_POINT ( 'NONE',  ( 0.3282822130750457923, -1.293256442918319538, 0.5434200829396130805 ) ) ;
#19861 = EDGE_LOOP ( 'NONE', ( #6042, #21760, #23284, #34713 ) ) ;
#19862 = CARTESIAN_POINT ( 'NONE',  ( 0.2101702454653370800, -0.9424526697851294266, 0.6590696260816275576 ) ) ;
#19863 = CARTESIAN_POINT ( 'NONE',  ( 0.01895884884825177821, -0.2428741539084897094, 0.4598572020609204558 ) ) ;
#19864 = CARTESIAN_POINT ( 'NONE',  ( 0.5105486452057178548, -1.310984060847071975, 0.6057417262808281189 ) ) ;
#19865 = VERTEX_POINT ( 'NONE', #11864 ) ;
#19866 = CARTESIAN_POINT ( 'NONE',  ( 0.4650133494175291982, -1.133480851973431847, -0.6660426939124519663 ) ) ;
#19867 = CARTESIAN_POINT ( 'NONE',  ( 0.5311646237512303026, -1.165099885119055712, 0.5038258806297195580 ) ) ;
#19868 = CIRCLE ( 'NONE', #27771, 0.01500000000000006016 ) ;
#19869 = CARTESIAN_POINT ( 'NONE',  ( 0.3514318747802386289, -1.706361087322654235, -0.4728986729284584412 ) ) ;
#19870 = CARTESIAN_POINT ( 'NONE',  ( -0.05634304521267748805, 1.092739197465705287E-15, 0.4588823192046724841 ) ) ;
#19871 = CARTESIAN_POINT ( 'NONE',  ( 0.2606834830056775076, -1.287120324457716736, 0.6747163837352363469 ) ) ;
#19872 = VERTEX_POINT ( 'NONE', #21140 ) ;
#19873 = CARTESIAN_POINT ( 'NONE',  ( -0.02869712619511965296, -0.3396447909410095223, -0.3648221446286677438 ) ) ;
#19874 = VECTOR ( 'NONE', #36379, 39.37007874015748143 ) ;
#19875 = AXIS2_PLACEMENT_3D ( 'NONE', #38820, #13335, #10447 ) ;
#19876 = DIRECTION ( 'NONE',  ( 1.000000000000000000, 0.000000000000000000, 7.515112548955565209E-16 ) ) ;
#19877 = FACE_OUTER_BOUND ( 'NONE', #9725, .T. ) ;
#19878 = DIRECTION ( 'NONE',  ( 0.000000000000000000, 0.000000000000000000, -1.000000000000000000 ) ) ;
#19879 = AXIS2_PLACEMENT_3D ( 'NONE', #3096, #2885, #11736 ) ;
#19880 = CARTESIAN_POINT ( 'NONE',  ( 0.4706509655328846575, -1.243911349059814375, 0.6624884991776383014 ) ) ;
#19882 = CARTESIAN_POINT ( 'NONE',  ( 0.4709867352971914833, -1.164672508904967652, -0.5155029497116575543 ) ) ;
#19881 = CARTESIAN_POINT ( 'NONE',  ( 0.1499999999999993561, 0.09319974324248773978, -0.5318964258758787089 ) ) ;
#19883 = CARTESIAN_POINT ( 'NONE',  ( 0.2159838750730762591, -0.9307556585230835067, 0.3864363914520806964 ) ) ;
#19884 = ORIENTED_EDGE ( 'NONE', *, *, #23552, .F. ) ;
#19885 = ITEM_DEFINED_TRANSFORMATION ( 'NONE', 'NONE', #8153,  #27819 ) ;
#19886 = FACE_OUTER_BOUND ( 'NONE', #33380, .T. ) ;
#19887 = ORIENTED_EDGE ( 'NONE', *, *, #17205, .F. ) ;
#19888 = CARTESIAN_POINT ( 'NONE',  ( 0.4162243804113466839, -1.587913871921676989, 0.6315551494585328607 ) ) ;
#19889 = AXIS2_PLACEMENT_3D ( 'NONE', #30781, #37352, #21340 ) ;
#19891 = CARTESIAN_POINT ( 'NONE',  ( 0.1113603080763501257, -0.9086058680110904451, 0.04931519565019508444 ) ) ;
#19890 = CARTESIAN_POINT ( 'NONE',  ( 0.4763501221259693330, -1.554011115824661893, -0.5166151207188711680 ) ) ;
#19892 = CARTESIAN_POINT ( 'NONE',  ( 0.1416495210772664437, -1.285147657081797012, 0.4817276165705878244 ) ) ;
#19893 = ORIENTED_EDGE ( 'NONE', *, *, #4613, .F. ) ;
#19894 = ORIENTED_EDGE ( 'NONE', *, *, #24543, .F. ) ;
#19895 = CARTESIAN_POINT ( 'NONE',  ( 0.1472892881247072627, -0.6767312212032746688, 0.4647785827719352891 ) ) ;
#19896 = ORIENTED_EDGE ( 'NONE', *, *, #14000, .T. ) ;
#19897 = CARTESIAN_POINT ( 'NONE',  ( 0.5135328215522156903, -1.640276221155167358, -0.4151541396484864088 ) ) ;
#19898 = CARTESIAN_POINT ( 'NONE',  ( 0.03301162916267580405, -0.5156255563253935303, 0.07469829950278324138 ) ) ;
#19899 = DIRECTION ( 'NONE',  ( 1.060606950627616773E-16, 6.122684696619993730E-17, 1.000000000000000000 ) ) ;
#19900 = CARTESIAN_POINT ( 'NONE',  ( 0.3019775573823714199, -1.138158212549354120, 0.5182417262812423209 ) ) ;
#19901 = AXIS2_PLACEMENT_3D ( 'NONE', #25, #3254, #40076 ) ;
#19902 = PLANE ( 'NONE',  #39093 ) ;
#19903 = CARTESIAN_POINT ( 'NONE',  ( 0.3969700875656219652, -1.750093955434198989, -0.5306525527942704823 ) ) ;
#19904 = CARTESIAN_POINT ( 'NONE',  ( 0.7110566119663160878, -1.453354452021889731, 0.7718588955819412067 ) ) ;
#19905 = CIRCLE ( 'NONE', #12006, 0.01500000000000007057 ) ;
#19906 = CARTESIAN_POINT ( 'NONE',  ( 0.3842624604883869144, -1.722789849446889177, -0.7210690300480241399 ) ) ;
#19907 = VECTOR ( 'NONE', #33005, 39.37007874015748854 ) ;
#19908 = DIRECTION ( 'NONE',  ( 2.532366176626896502E-12, 0.8090169943749470072, -0.5877852522924736922 ) ) ;
#19909 = CARTESIAN_POINT ( 'NONE',  ( 0.02869712619511872662, -0.2420104654861707505, -0.4357576342647261902 ) ) ;
#19910 = PERSON_AND_ORGANIZATION ( #28500, #32463 ) ;
#19911 = CARTESIAN_POINT ( 'NONE',  ( 0.6348086598072710807, -1.524658463883513004, -0.6128917709820664861 ) ) ;
#19912 = CARTESIAN_POINT ( 'NONE',  ( 0.2285146069045126682, -1.350404058286757136, 0.4993478297109967268 ) ) ;
#19913 = CARTESIAN_POINT ( 'NONE',  ( -0.02000000000000000042, -2.616518742763782601, -0.2555225440839158368 ) ) ;
#19914 = CARTESIAN_POINT ( 'NONE',  ( 0.4112193008909481584, -1.591609915475934889, -0.6177460231409163116 ) ) ;
#19915 = AXIS2_PLACEMENT_3D ( 'NONE', #25076, #22619, #19113 ) ;
#19916 = CARTESIAN_POINT ( 'NONE',  ( 0.1472911887417822641, -1.284155632031082517, 0.4182314466967200772 ) ) ;
#19917 = VERTEX_POINT ( 'NONE', #17444 ) ;
#19918 = CARTESIAN_POINT ( 'NONE',  ( 0.05992416651567116642, -0.8828589634183678925, 0.7642515975180658172 ) ) ;
#19919 = CARTESIAN_POINT ( 'NONE',  ( 0.5659382422188921069, -1.581708796928036342, -0.4824204755890118546 ) ) ;
#19920 = LINE ( 'NONE', #28964, #7441 ) ;
#19921 = DIRECTION ( 'NONE',  ( -1.000000000000000000, -0.000000000000000000, -0.000000000000000000 ) ) ;
#19922 = CARTESIAN_POINT ( 'NONE',  ( -0.03672309138969926529, -0.3146134659443306503, 0.3636027875696402623 ) ) ;
#19923 = ORIENTED_EDGE ( 'NONE', *, *, #6279, .F. ) ;
#19924 = ORIENTED_EDGE ( 'NONE', *, *, #26296, .F. ) ;
#19925 = CARTESIAN_POINT ( 'NONE',  ( 0.2321526281619643584, -1.233007205928619232, 0.3667417262808778111 ) ) ;
#19926 = ORIENTED_EDGE ( 'NONE', *, *, #3960, .T. ) ;
#19927 = LINE ( 'NONE', #3693, #16501 ) ;
#19928 = DIRECTION ( 'NONE',  ( 0.000000000000000000, -3.414809992080312950E-15, -1.000000000000000000 ) ) ;
#19929 = AXIS2_PLACEMENT_3D ( 'NONE', #29049, #23103, #7432 ) ;
#19930 = CARTESIAN_POINT ( 'NONE',  ( 0.4074053067644164972, -1.158105270543656085, 0.7726839899096992204 ) ) ;
#19931 = B_SPLINE_CURVE_WITH_KNOTS ( 'NONE', 3,
 ( #33267, #11066, #20939, #36957, #8775, #17636, #33891, #30183, #15361, #6489, #15573, #22359, #21739, #31210, #19060, #392, #30989, #34274 ),
 .UNSPECIFIED., .F., .F.,
 ( 4, 2, 2, 2, 2, 2, 2, 2, 4 ),
 ( 0.0003425652276237174795, 0.001007165397454229221, 0.001671765567284740853, 0.002336365737115257257, 0.003000965906945773660, 0.003665566076776290063, 0.004330166246606806033, 0.004994766416437322436, 0.005659366586267838839 ),
 .UNSPECIFIED. ) ;
#19933 = ORIENTED_EDGE ( 'NONE', *, *, #12042, .T. ) ;
#19932 = CARTESIAN_POINT ( 'NONE',  ( 0.5676041605235047083, -1.626300245317876980, 0.5026027723836924421 ) ) ;
#19934 = CARTESIAN_POINT ( 'NONE',  ( 0.3637128952805344095, -0.9645059733743139851, 0.6550525653421633843 ) ) ;
#19935 = CARTESIAN_POINT ( 'NONE',  ( 0.1499999999999994948, 0.4770632572900484480, 0.2530032579707400253 ) ) ;
#19936 = EDGE_LOOP ( 'NONE', ( #14438, #18323, #29598, #21192 ) ) ;
#19937 = CARTESIAN_POINT ( 'NONE',  ( 0.3562792623313784657, -1.606250998287605869, -0.3924671920701706118 ) ) ;
#19938 = AXIS2_PLACEMENT_3D ( 'NONE', #14958, #21740, #18652 ) ;
#19939 = AXIS2_PLACEMENT_3D ( 'NONE', #5408, #9112, #36500 ) ;
#19940 = CARTESIAN_POINT ( 'NONE',  ( 0.02322307456033168363, -0.5318894034165194684, 0.1457185332388691024 ) ) ;
#19942 = CARTESIAN_POINT ( 'NONE',  ( -0.03868649100028177801, -0.2522293598345298204, 0.4043344736883388024 ) ) ;
#19941 = CARTESIAN_POINT ( 'NONE',  ( 0.6300906668383386977, -1.574674102679878063, 0.4263063865966011945 ) ) ;
#19943 = CARTESIAN_POINT ( 'NONE',  ( 0.1435064959217801916, -1.283467536720964697, 0.5197417262808780025 ) ) ;
#19944 = CARTESIAN_POINT ( 'NONE',  ( 0.02998331132317445802, -2.054508416935759474, -0.2740450252055757763 ) ) ;
#19945 = ORIENTED_EDGE ( 'NONE', *, *, #34783, .T. ) ;
#19946 = CARTESIAN_POINT ( 'NONE',  ( 0.3999999999999787059, -2.183180860297921466, -0.4937760292030871079 ) ) ;
#19947 = CARTESIAN_POINT ( 'NONE',  ( 0.2172743585675568356, -0.8579260410846445417, 0.4051362072568608919 ) ) ;
#19948 = AXIS2_PLACEMENT_3D ( 'NONE', #36955, #11470, #21553 ) ;
#19949 = LINE ( 'NONE', #269, #33791 ) ;
#19950 = DIRECTION ( 'NONE',  ( 0.000000000000000000, 0.000000000000000000, 1.000000000000000000 ) ) ;
#19951 = CIRCLE ( 'NONE', #19315, 0.2200000000000001121 ) ;
#19952 = ADVANCED_FACE ( 'NONE', ( #1829 ), #20314, .F. ) ;
#19953 = CARTESIAN_POINT ( 'NONE',  ( 0.3583570516064159550, -1.223096128769133317, 0.6863269740785166162 ) ) ;
#19954 = CARTESIAN_POINT ( 'NONE',  ( 0.01083811821583093374, -0.5479617008785322430, 0.2379223945615984992 ) ) ;
#19955 = APPROVAL ( #21262, 'UNKNOWN' ) ;
#19956 = CARTESIAN_POINT ( 'NONE',  ( 0.4076976354719480944, -1.154888438488553826, 0.4182417262808778013 ) ) ;
#19957 = CARTESIAN_POINT ( 'NONE',  ( -0.1628177922134119437, 0.5059000297268509971, 0.3228062255482125331 ) ) ;
#19958 = CARTESIAN_POINT ( 'NONE',  ( 0.6544078563150221850, -1.544269123161552626, 0.4241055859090109292 ) ) ;
#19959 = DIRECTION ( 'NONE',  ( 0.000000000000000000, 0.000000000000000000, -1.000000000000000000 ) ) ;
#19960 = CYLINDRICAL_SURFACE ( 'NONE', #35832, 0.04249999999999995448 ) ;
#19961 = CARTESIAN_POINT ( 'NONE',  ( -0.02000000000000000042, -2.023118915020511999, -0.4686803309516410221 ) ) ;
#19962 = DIRECTION ( 'NONE',  ( 1.000000000000000000, -6.392190818188219650E-17, 4.937986043002253904E-17 ) ) ;
#19963 = CIRCLE ( 'NONE', #25216, 0.02999999999999998848 ) ;
#19964 = CARTESIAN_POINT ( 'NONE',  ( 0.02906710819876866247, -1.111300232264741172, 0.6609726249879336324 ) ) ;
#19965 = CARTESIAN_POINT ( 'NONE',  ( 0.1786313307395676619, -0.4924000933286005743, 0.1338216977563466970 ) ) ;
#19966 = CARTESIAN_POINT ( 'NONE',  ( 0.1099256020772691467, -1.419293905719575477, 0.5685549581676759834 ) ) ;
#19967 = TOROIDAL_SURFACE ( 'NONE', #30480, 0.05330708661417323663, 0.01000000000000000021 ) ;
#19968 = TOROIDAL_SURFACE ( 'NONE', #2875, 0.2200000000000000011, 0.02999999999999999889 ) ;
#19969 = CARTESIAN_POINT ( 'NONE',  ( -0.2399999999999999079, -3.755970012053913010, 0.01635628697548255697 ) ) ;
#19970 = CARTESIAN_POINT ( 'NONE',  ( 0.3571704890607551586, -1.830049479072539231, -0.6659963912414424980 ) ) ;
#19971 = CARTESIAN_POINT ( 'NONE',  ( 0.2934918387085203584, -1.644164324632618301, 0.9129472502802961076 ) ) ;
#19972 = DIRECTION ( 'NONE',  ( -1.000000000000000000, 0.000000000000000000, 0.000000000000000000 ) ) ;
#19973 = EDGE_CURVE ( 'NONE', #19021, #37901, #12999, .T. ) ;
#19974 = CONICAL_SURFACE ( 'NONE', #22641, 0.1346589359789737705, 1.047197551196598075 ) ;
#19975 = ADVANCED_FACE ( 'NONE', ( #36756 ), #12084, .F. ) ;
#19976 = ORIENTED_EDGE ( 'NONE', *, *, #29019, .F. ) ;
#19977 = CIRCLE ( 'NONE', #40350, 0.06250000000000001388 ) ;
#19978 = EDGE_LOOP ( 'NONE', ( #13557, #35128, #30712, #31509 ) ) ;
#19979 = CARTESIAN_POINT ( 'NONE',  ( 0.1828835028638483573, -0.5190310081367575101, 0.2566657934198534052 ) ) ;
#19980 = ORIENTED_EDGE ( 'NONE', *, *, #32903, .T. ) ;
#19981 = DIRECTION ( 'NONE',  ( 1.000000000000000000, -0.000000000000000000, -0.000000000000000000 ) ) ;
#19982 = ADVANCED_FACE ( 'NONE', ( #14544 ), #27111, .T. ) ;
#19983 = CARTESIAN_POINT ( 'NONE',  ( 0.4807263528268903019, -1.305708637018340834, 0.8152355762322205379 ) ) ;
#19984 = ADVANCED_FACE ( 'NONE', ( #37778 ), #39991, .T. ) ;
#19986 = VERTEX_POINT ( 'NONE', #3417 ) ;
#19985 = CARTESIAN_POINT ( 'NONE',  ( 0.5082546964191734240, -1.641980856392960098, -0.4117015674416750204 ) ) ;
#19987 = EDGE_CURVE ( 'NONE', #7962, #4385, #28473, .T. ) ;
#19989 = EDGE_LOOP ( 'NONE', ( #38843, #6722, #4822, #26814 ) ) ;
#19988 = ORIENTED_EDGE ( 'NONE', *, *, #33172, .T. ) ;
#19990 = CARTESIAN_POINT ( 'NONE',  ( 0.3088934897170949045, -1.189159158785630277, 0.5061700154489670034 ) ) ;
#19991 = ORIENTED_EDGE ( 'NONE', *, *, #39193, .F. ) ;
#19992 = CARTESIAN_POINT ( 'NONE',  ( -0.004170050296584535375, -0.6270701198925358044, 0.4329761698911018253 ) ) ;
#19993 = CARTESIAN_POINT ( 'NONE',  ( 0.1711601909574965164, -1.383443734294387939, 0.5378582171031165426 ) ) ;
#19994 = CARTESIAN_POINT ( 'NONE',  ( 0.6126863732757561465, -1.613714656222153154, -0.4894191377505581197 ) ) ;
#19995 = CONTEXT_DEPENDENT_SHAPE_REPRESENTATION ( #1930, #8154 ) ;
#19996 = AXIS2_PLACEMENT_3D ( 'NONE', #27020, #30300, #11379 ) ;
#19997 = CARTESIAN_POINT ( 'NONE',  ( -0.2746410161513782033, -2.183180860297908144, -0.9552969701112735690 ) ) ;
#19999 = VERTEX_POINT ( 'NONE', #28127 ) ;
#19998 = EDGE_LOOP ( 'NONE', ( #29498, #14968, #39708, #16984, #32859 ) ) ;
#20000 = CARTESIAN_POINT ( 'NONE',  ( 0.09474359960899157718, -0.7992767504562960923, 0.3037933874108209031 ) ) ;
#20001 = CIRCLE ( 'NONE', #2270, 0.01499999999999997689 ) ;
#20002 = CARTESIAN_POINT ( 'NONE',  ( 0.07274636059270921107, -0.5712887667331841834, 0.2713463052083351368 ) ) ;
#20003 = CIRCLE ( 'NONE', #20654, 1.991674066779348218 ) ;
#20004 = CARTESIAN_POINT ( 'NONE',  ( 0.1117061238851624477, -0.5727138467974830505, 0.2548588568801546383 ) ) ;
#20005 = CARTESIAN_POINT ( 'NONE',  ( 0.1777497266415261346, -0.4987312181850360182, 0.2142283185154747749 ) ) ;
#20006 = ADVANCED_FACE ( 'NONE', ( #25237 ), #14967, .F. ) ;
#20007 = CARTESIAN_POINT ( 'NONE',  ( 0.4739235880194173633, -1.591156355542383105, -0.4387572789578180754 ) ) ;
#20008 =( GEOMETRIC_REPRESENTATION_CONTEXT ( 3 ) GLOBAL_UNCERTAINTY_ASSIGNED_CONTEXT ( ( #24404 ) ) GLOBAL_UNIT_ASSIGNED_CONTEXT ( ( #36843, #21026, #18537 ) ) REPRESENTATION_CONTEXT ( 'NONE', 'WORKASPACE' ) );
#20009 = CARTESIAN_POINT ( 'NONE',  ( 0.1499999999999996336, -0.2306506793134066036, 0.4716198300880325434 ) ) ;
#20010 = CARTESIAN_POINT ( 'NONE',  ( 0.3329225671462469061, -1.751883312225780420, 0.5693379886238489895 ) ) ;
#20011 = CARTESIAN_POINT ( 'NONE',  ( 0.4544607142047081272, -1.663558774996698464, -0.4080516749217623640 ) ) ;
#20012 = AXIS2_PLACEMENT_3D ( 'NONE', #19194, #24773, #21491 ) ;
#20013 = CARTESIAN_POINT ( 'NONE',  ( 0.5202445037400105221, -1.603350735003311156, -0.6087954913505664312 ) ) ;
#20014 = CARTESIAN_POINT ( 'NONE',  ( 0.1890965627226634804, -1.347655541994686068, 0.5182417262812423209 ) ) ;
#20015 = CYLINDRICAL_SURFACE ( 'NONE', #14686, 0.01500000000000004108 ) ;
#20016 = AXIS2_PLACEMENT_3D ( 'NONE', #17924, #8463, #2707 ) ;
#20017 = CARTESIAN_POINT ( 'NONE',  ( -9.774798136714478227E-06, -0.8191943866653442763, -0.07958805542202744554 ) ) ;
#20018 = CARTESIAN_POINT ( 'NONE',  ( 0.4028317915878064648, -1.175318803141969681, 0.8151889077341930578 ) ) ;
#20019 = CARTESIAN_POINT ( 'NONE',  ( 0.007470885619759358443, -0.7664851069221876312, 0.008519161373831274017 ) ) ;
#20020 = DIRECTION ( 'NONE',  ( 0.4999551463232372317, -0.8660512985181134660, 0.000000000000000000 ) ) ;
#20021 = CARTESIAN_POINT ( 'NONE',  ( -0.003075981321608621880, -0.8070878537792822716, 0.1960017582677906212 ) ) ;
#20022 = CARTESIAN_POINT ( 'NONE',  ( 0.4929465528686912679, -1.082715557938388029, 0.5639242819095140469 ) ) ;
#20023 = COORDINATED_UNIVERSAL_TIME_OFFSET ( 0, 0, .AHEAD. ) ;
#20024 = B_SPLINE_CURVE_WITH_KNOTS ( 'NONE', 3,
 ( #38300, #22707, #35238, #7039, #19608, #38711, #3944, #16506, #10531, #16919 ),
 .UNSPECIFIED., .F., .F.,
 ( 4, 2, 2, 2, 4 ),
 ( 0.003098629625065144923, 0.003873295706325716355, 0.004647961787586288654, 0.005422627868846860086, 0.006197293950107432385 ),
 .UNSPECIFIED. ) ;
#20025 = AXIS2_PLACEMENT_3D ( 'NONE', #16153, #28691, #25605 ) ;
#20026 = CIRCLE ( 'NONE', #25289, 0.07999999999999996003 ) ;
#20027 = CARTESIAN_POINT ( 'NONE',  ( -0.01895884884825282252, 0.5124024296374540821, -0.08888335629180008080 ) ) ;
#20028 = CARTESIAN_POINT ( 'NONE',  ( -3.757258772823647403E-22, 0.06117178301711218014, -0.1249999999999999029 ) ) ;
#20029 = EDGE_CURVE ( 'NONE', #39766, #6871, #2356, .T. ) ;
#20030 = CIRCLE ( 'NONE', #1009, 0.5400000000000001465 ) ;
#20031 = ORIENTED_EDGE ( 'NONE', *, *, #24794, .F. ) ;
#20032 = DIRECTION ( 'NONE',  ( 2.465190328815661892E-32, 1.000000000000000000, 6.656013887802287108E-31 ) ) ;
#20033 = LOCAL_TIME ( 0, 53, 7.000000000000000000, #19704 ) ;
#20034 = CARTESIAN_POINT ( 'NONE',  ( 0.01149458178949343268, -0.5639228391815407360, 0.2834883079787945959 ) ) ;
#20035 = ADVANCED_FACE ( 'NONE', ( #27454 ), #21071, .T. ) ;
#20036 = CARTESIAN_POINT ( 'NONE',  ( 0.2106106046344508043, -1.233927216831852025, 0.4729821282189752840 ) ) ;
#20037 = VERTEX_POINT ( 'NONE', #2552 ) ;
#20038 = CARTESIAN_POINT ( 'NONE',  ( 0.3339246645468108010, -1.752618221267800536, 0.4594630238594379357 ) ) ;
#20039 = EDGE_CURVE ( 'NONE', #1740, #6763, #25750, .T. ) ;
#20040 = VECTOR ( 'NONE', #33358, 39.37007874015748143 ) ;
#20041 = CARTESIAN_POINT ( 'NONE',  ( 0.1898244942508440503, -0.5073357646527311138, 0.1864979583367220028 ) ) ;
#20043 = VERTEX_POINT ( 'NONE', #5213 ) ;
#20042 = ORIENTED_EDGE ( 'NONE', *, *, #38948, .T. ) ;
#20044 = CARTESIAN_POINT ( 'NONE',  ( 0.3336071016620586471, -1.750777463471590023, -0.4969093018047625043 ) ) ;
#20045 = ORIENTED_EDGE ( 'NONE', *, *, #3599, .F. ) ;
#20046 = DIRECTION ( 'NONE',  ( -7.771561172376107616E-16, 7.170354002788761615E-17, -1.000000000000000000 ) ) ;
#20047 = CARTESIAN_POINT ( 'NONE',  ( 0.3434800707738386305, -1.169184835483333185, 0.4282596159935695423 ) ) ;
#20048 = CARTESIAN_POINT ( 'NONE',  ( -0.02881302694829541641, 0.4889319715862935900, -0.09562644460326163998 ) ) ;
#20049 = VERTEX_POINT ( 'NONE', #20883 ) ;
#20050 = CARTESIAN_POINT ( 'NONE',  ( 0.2209899243456227846, -1.361115721219026797, 1.190013540297138572 ) ) ;
#20051 = CARTESIAN_POINT ( 'NONE',  ( 0.08767352474349697500, -0.6847778086286057109, 0.1675417422483599927 ) ) ;
#20052 = CARTESIAN_POINT ( 'NONE',  ( 0.1058629817858797312, -0.9473122495338976989, 0.9158932442105627292 ) ) ;
#20053 = CARTESIAN_POINT ( 'NONE',  ( 0.4695230613062974512, -1.557919065767196187, 0.5700130294922880481 ) ) ;
#20054 = ADVANCED_FACE ( 'NONE', ( #15089 ), #14687, .F. ) ;
#20056 = DIRECTION ( 'NONE',  ( -0.8735110198817035432, 0.000000000000000000, 0.4868043735888433754 ) ) ;
#20055 = CARTESIAN_POINT ( 'NONE',  ( 0.1153471662232078698, -0.4465907064269051263, 0.1457432652200511269 ) ) ;
#20057 = EDGE_CURVE ( 'NONE', #35002, #18607, #33729, .T. ) ;
#20058 = CARTESIAN_POINT ( 'NONE',  ( 0.3296550237143848205, -1.099205586124516909, 0.6409462830847290071 ) ) ;
#20059 = ORIENTED_EDGE ( 'NONE', *, *, #995, .T. ) ;
#20060 = EDGE_CURVE ( 'NONE', #8808, #34243, #33406, .T. ) ;
#20061 = ORIENTED_EDGE ( 'NONE', *, *, #11959, .T. ) ;
#20062 = CARTESIAN_POINT ( 'NONE',  ( 0.3177859269536487119, -1.645585450493298962, 0.5231366550910405699 ) ) ;
#20063 = EDGE_CURVE ( 'NONE', #19690, #31025, #8918, .T. ) ;
#20064 = CARTESIAN_POINT ( 'NONE',  ( 0.1185549026673793083, -0.4796779786644438937, 0.2928297671798744672 ) ) ;
#20065 = CIRCLE ( 'NONE', #33824, 0.1333070866141734812 ) ;
#20066 = DIRECTION ( 'NONE',  ( -0.5176477751948445061, -0.2988283368828927866, -0.8017121714877678551 ) ) ;
#20067 = CIRCLE ( 'NONE', #2324, 0.1700000000000000400 ) ;
#20068 = APPLIED_APPROVAL_ASSIGNMENT ( #7104, ( #37152 ) ) ;
#20069 = CARTESIAN_POINT ( 'NONE',  ( -0.02872242845530506572, -0.5252126300208028731, -0.08844866507293215607 ) ) ;
#20070 = FACE_OUTER_BOUND ( 'NONE', #38879, .T. ) ;
#20071 =( REPRESENTATION_RELATIONSHIP ('NONE','NONE', #33020, #31708 ) REPRESENTATION_RELATIONSHIP_WITH_TRANSFORMATION ( #10336 )SHAPE_REPRESENTATION_RELATIONSHIP( ) );
#20072 = VECTOR ( 'NONE', #13379, 39.37007874015748143 ) ;
#20073 = CARTESIAN_POINT ( 'NONE',  ( 0.5974340449968663647, -1.261189741147681787, 0.6853727476855657752 ) ) ;
#20074 =( BOUNDED_SURFACE ( )  B_SPLINE_SURFACE ( 3, 2, ( 
 ( #30143, #13688, #11028 ),
 ( #7721, #4609, #11421 ),
 ( #17185, #32807, #36103 ),
 ( #10602, #20288, #7512 ),
 ( #29730, #26254, #11214 ),
 ( #4429, #7907, #29529 ) ),
 .UNSPECIFIED., .F., .F., .F. ) 
 B_SPLINE_SURFACE_WITH_KNOTS ( ( 4, 2, 4 ),
 ( 3, 3 ),
 ( 0.01236296969923212849, 0.01327412252728663034, 0.01418527535534113218 ),
 ( 0.8365089563635481618, 1.000000000000000000 ),
 .UNSPECIFIED. ) 
 GEOMETRIC_REPRESENTATION_ITEM ( )  RATIONAL_B_SPLINE_SURFACE ( (
 ( 0.9196845010948848653, 0.9519936407768658793, 1.000000000000000000),
 ( 0.9196791632980176878, 0.9519904502570114557, 1.000000000000000000),
 ( 0.9196826974396685728, 0.9519925626920452411, 1.000000000000000000),
 ( 0.9196970493731875251, 0.9520011411617733676, 1.000000000000000000),
 ( 0.9197077343035476860, 0.9520075277821907767, 1.000000000000000000),
 ( 0.9197191540535247789, 0.9520143536206293611, 1.000000000000000000) ) ) 
 REPRESENTATION_ITEM ( '' )  SURFACE ( )  );
#20075 = CARTESIAN_POINT ( 'NONE',  ( 0.5409940809552228336, -1.629370368867399055, 0.4283118504128637927 ) ) ;
#20076 = CARTESIAN_POINT ( 'NONE',  ( 0.005974781723437884440, -0.8455926680098735382, 0.1913255637356532368 ) ) ;
#20077 = CARTESIAN_POINT ( 'NONE',  ( 0.05201840200954787469, 0.4415345355162785257, -0.1624690192511295816 ) ) ;
#20078 = DIRECTION ( 'NONE',  ( -1.000000000000000000, -7.857794173099924470E-32, -8.628166150854818811E-32 ) ) ;
#20079 = EDGE_LOOP ( 'NONE', ( #10722, #18173, #40412, #6662, #2229, #22227, #12595 ) ) ;
#20080 = CARTESIAN_POINT ( 'NONE',  ( 0.2399278993395743964, -0.9290780320567488815, 0.6800090796796801618 ) ) ;
#20081 = DIRECTION ( 'NONE',  ( 0.000000000000000000, 0.000000000000000000, -1.000000000000000000 ) ) ;
#20082 = FACE_OUTER_BOUND ( 'NONE', #28396, .T. ) ;
#20083 = ORIENTED_EDGE ( 'NONE', *, *, #27357, .F. ) ;
#20084 = CARTESIAN_POINT ( 'NONE',  ( 0.1499999999999994948, 0.1249999999999999029, 0.000000000000000000 ) ) ;
#20085 = ORIENTED_EDGE ( 'NONE', *, *, #33172, .F. ) ;
#20086 = CARTESIAN_POINT ( 'NONE',  ( -0.05082294681499043010, 0.04864283519431752273, -0.4711332289091950121 ) ) ;
#20087 = EDGE_CURVE ( 'NONE', #9596, #23678, #21269, .T. ) ;
#20088 = CARTESIAN_POINT ( 'NONE',  ( 0.3593346688482150775, -1.735925422213634661, -0.5010936962835139674 ) ) ;
#20089 = DIRECTION ( 'NONE',  ( 0.4999551463232372317, -0.8660512985181135770, 0.000000000000000000 ) ) ;
#20090 = CIRCLE ( 'NONE', #12182, 0.01499999999999995434 ) ;
#20091 = EDGE_CURVE ( 'NONE', #10562, #18074, #12009, .T. ) ;
#20092 = CARTESIAN_POINT ( 'NONE',  ( 0.09229806196967101084, -0.9044670966804603252, 0.5687378640879924285 ) ) ;
#20093 = VERTEX_POINT ( 'NONE', #30125 ) ;
#20094 = CARTESIAN_POINT ( 'NONE',  ( -0.04229956186878668090, -0.2825373843407160690, -0.3739591931584715367 ) ) ;
#20095 = CARTESIAN_POINT ( 'NONE',  ( 0.4219866632171650478, -1.610104465087853765, -0.3647299066799348233 ) ) ;
#20096 = APPLIED_APPROVAL_ASSIGNMENT ( #35281, ( #5625 ) ) ;
#20097 = CARTESIAN_POINT ( 'NONE',  ( 0.1223045647424210181, -1.412159682085746271, 0.4849083929475432320 ) ) ;
#20098 = DIRECTION ( 'NONE',  ( 1.060606950627616773E-16, 6.122684696619993730E-17, 1.000000000000000000 ) ) ;
#20099 = CARTESIAN_POINT ( 'NONE',  ( 0.3840497050944557955, -1.128614810062711360, 0.7138234942851187093 ) ) ;
#20101 = CARTESIAN_POINT ( 'NONE',  ( 0.3582455198832254495, -1.774135343334821924, -0.4890060775958486872 ) ) ;
#20100 = DIRECTION ( 'NONE',  ( -1.000000000000000000, 0.000000000000000000, 0.000000000000000000 ) ) ;
#20102 = CARTESIAN_POINT ( 'NONE',  ( 0.5713772049386515173, -1.545306863045628143, -0.5074489717415853196 ) ) ;
#20103 = ORIENTED_EDGE ( 'NONE', *, *, #18331, .F. ) ;
#20104 = CIRCLE ( 'NONE', #31294, 0.1033070866141734129 ) ;
#20105 = CARTESIAN_POINT ( 'NONE',  ( -0.1508044614562676355, 0.4665164580004940720, 0.3602693336111434941 ) ) ;
#20106 = ORIENTED_EDGE ( 'NONE', *, *, #28657, .T. ) ;
#20107 = CARTESIAN_POINT ( 'NONE',  ( 0.4135726104504772183, -1.589529505291096489, 0.5730501051810202862 ) ) ;
#20109 = DIRECTION ( 'NONE',  ( -0.4999551463232371207, 0.8660512985181134660, 0.000000000000000000 ) ) ;
#20108 = CARTESIAN_POINT ( 'NONE',  ( 0.08792459278225348007, -0.6496347354946547803, 0.006458355081153737201 ) ) ;
#20110 = CARTESIAN_POINT ( 'NONE',  ( 0.1841497487818726797, -1.740483164027640584, -0.3571093288873294358 ) ) ;
#20111 = EDGE_CURVE ( 'NONE', #37905, #5340, #25855, .T. ) ;
#20112 = ORIENTED_EDGE ( 'NONE', *, *, #38689, .F. ) ;
#20113 = EDGE_LOOP ( 'NONE', ( #1921, #23734, #14223, #13953 ) ) ;
#20114 = EDGE_CURVE ( 'NONE', #5909, #1137, #14428, .T. ) ;
#20115 = DIRECTION ( 'NONE',  ( 0.000000000000000000, 0.000000000000000000, -1.000000000000000000 ) ) ;
#20116 = CARTESIAN_POINT ( 'NONE',  ( 0.1192362759130453781, -0.5567294128173433387, 0.1990477325651368867 ) ) ;
#20117 = EDGE_LOOP ( 'NONE', ( #18520, #9743, #26789, #9618 ) ) ;
#20118 = CARTESIAN_POINT ( 'NONE',  ( 0.5612334960093817715, -1.620627794947044897, -0.4868944820179721966 ) ) ;
#20119 = CARTESIAN_POINT ( 'NONE',  ( 0.04760578872587564042, -0.4435171289962518970, 0.1893230556938431397 ) ) ;
#20120 = CARTESIAN_POINT ( 'NONE',  ( 0.6521185033023279010, -1.542907011849267596, 0.4182417262808777458 ) ) ;
#20121 = CARTESIAN_POINT ( 'NONE',  ( 0.2292879920235051938, -1.234689012067045066, 0.4835017060594773430 ) ) ;
#20122 = CARTESIAN_POINT ( 'NONE',  ( 0.5652024041994130332, -1.318123455396758681, -0.6186948529734399571 ) ) ;
#20123 = LINE ( 'NONE', #1818, #37143 ) ;
#20124 = AXIS2_PLACEMENT_3D ( 'NONE', #32022, #9611, #35318 ) ;
#20125 = CIRCLE ( 'NONE', #5645, 0.03000000000000010297 ) ;
#20126 = CARTESIAN_POINT ( 'NONE',  ( 0.5536297569049346556, -1.186194075236972179, 0.6057417262809815517 ) ) ;
#20127 = LINE ( 'NONE', #38215, #19459 ) ;
#20128 = FACE_OUTER_BOUND ( 'NONE', #26688, .T. ) ;
#20129 = APPROVAL_ROLE ( '' ) ;
#20130 = APPLIED_APPROVAL_ASSIGNMENT ( #30647, ( #14861 ) ) ;
#20131 = DIRECTION ( 'NONE',  ( 6.260484985480596356E-15, -0.9672079024912928480, 0.2539859707905017805 ) ) ;
#20132 = CARTESIAN_POINT ( 'NONE',  ( 0.02881195911414505262, 0.2420394953216123413, 0.4354516087588692352 ) ) ;
#20133 = CARTESIAN_POINT ( 'NONE',  ( 0.1836761679754468357, -0.5203768919390597825, 0.06931577267137481457 ) ) ;
#20134 = CARTESIAN_POINT ( 'NONE',  ( 0.2590195079428145863, -1.679471191969716060, 0.4398509372606123069 ) ) ;
#20135 = TOROIDAL_SURFACE ( 'NONE', #40499, 1.971674066779348866, 0.02999999999999999889 ) ;
#20136 = CARTESIAN_POINT ( 'NONE',  ( 0.1209954484009972825, -1.306288436253663976, 0.4272974611868050610 ) ) ;
#20137 = PERSON ( 'NAUO-PER15', 'UNSPECIFIED', 'UNSPECIFIED', ('UNSPECIFIED'), ('UNSPECIFIED'), ('UNSPECIFIED') ) ;
#20138 = CARTESIAN_POINT ( 'NONE',  ( 0.04376425988958544677, -0.9339557565548041174, 0.7112009851976159869 ) ) ;
#20139 = CARTESIAN_POINT ( 'NONE',  ( 0.5791375636586371112, -1.530547062312576534, -0.5677195341231595638 ) ) ;
#20140 = CARTESIAN_POINT ( 'NONE',  ( -2.134683096299215694E-14, -2.104523772034943452, -0.2882857580878072090 ) ) ;
#20141 = EDGE_CURVE ( 'NONE', #37512, #26023, #27202, .T. ) ;
#20142 = CARTESIAN_POINT ( 'NONE',  ( -0.1157923916715208196, -0.5295015842444287246, 0.3599999999999993205 ) ) ;
#20143 = CARTESIAN_POINT ( 'NONE',  ( -0.05634115714581377360, -0.2739512608647004521, 0.3681776108865941755 ) ) ;
#20144 = ORIENTED_EDGE ( 'NONE', *, *, #13025, .T. ) ;
#20145 = ORIENTED_EDGE ( 'NONE', *, *, #31085, .T. ) ;
#20146 = CARTESIAN_POINT ( 'NONE',  ( 0.3655542017575511005, -1.763257256764854786, -0.5881144261364762427 ) ) ;
#20147 = ORIENTED_EDGE ( 'NONE', *, *, #14559, .T. ) ;
#20148 = CARTESIAN_POINT ( 'NONE',  ( -0.1157923916715205420, -0.5295015842444287246, 0.09999999999999989453 ) ) ;
#20149 = DIRECTION ( 'NONE',  ( -0.4999551463232377313, 0.8660512985181132439, 0.000000000000000000 ) ) ;
#20150 = CARTESIAN_POINT ( 'NONE',  ( 0.4016278364854861116, -1.148462343513625639, 0.7933350346235505945 ) ) ;
#20152 = ORIENTED_EDGE ( 'NONE', *, *, #33815, .F. ) ;
#20151 = CARTESIAN_POINT ( 'NONE',  ( -0.04293317454820699819, 0.4876093284570324204, 0.08292018301452676321 ) ) ;
#20153 = CARTESIAN_POINT ( 'NONE',  ( 0.3909368226714677319, -0.9916197579736178991, 0.6726537802841677793 ) ) ;
#20154 = AXIS2_PLACEMENT_3D ( 'NONE', #39879, #30417, #2248 ) ;
#20155 = FACE_OUTER_BOUND ( 'NONE', #17158, .T. ) ;
#20156 = ORIENTED_EDGE ( 'NONE', *, *, #30297, .F. ) ;
#20157 = CARTESIAN_POINT ( 'NONE',  ( 0.3999999999999787059, -2.166079853131637645, -0.5407606602423824516 ) ) ;
#20158 = ORIENTED_EDGE ( 'NONE', *, *, #34273, .F. ) ;
#20159 = CARTESIAN_POINT ( 'NONE',  ( 0.02723342787037887069, -0.5846365886964711711, 0.3289579258136214879 ) ) ;
#20161 = DIRECTION ( 'NONE',  ( 0.4999551463232373427, -0.8660512985181134660, 0.000000000000000000 ) ) ;
#20160 = CARTESIAN_POINT ( 'NONE',  ( 0.7050266291804438978, -1.514791320213222159, 0.5680628335673595375 ) ) ;
#20162 = CARTESIAN_POINT ( 'NONE',  ( -0.05464101615137795243, -1.546789565643408526, -0.06332195561662121164 ) ) ;
#20163 = SECURITY_CLASSIFICATION ( '', '', #2075 ) ;
#20164 = CARTESIAN_POINT ( 'NONE',  ( 0.0006437153440169360308, -1.950600395569651369, -0.3015213215365759036 ) ) ;
#20165 = ORIENTED_EDGE ( 'NONE', *, *, #4920, .T. ) ;
#20166 = AXIS2_PLACEMENT_3D ( 'NONE', #9626, #37808, #4041 ) ;
#20167 = DIRECTION ( 'NONE',  ( 0.000000000000000000, 0.000000000000000000, 1.000000000000000000 ) ) ;
#20168 = CARTESIAN_POINT ( 'NONE',  ( 0.01374200611896923829, -1.689473050622495753, -0.6374908651714740193 ) ) ;
#20169 = CARTESIAN_POINT ( 'NONE',  ( 0.02869712619511921928, 0.4519224903895674994, 0.2102851490355753250 ) ) ;
#20170 = CARTESIAN_POINT ( 'NONE',  ( 0.2135156657176371930, -0.9834570136538726137, 0.6967854075931073643 ) ) ;
#20171 = CARTESIAN_POINT ( 'NONE',  ( 0.000000000000000000, -0.4700000000000001954, 0.000000000000000000 ) ) ;
#20172 = CARTESIAN_POINT ( 'NONE',  ( 0.4750664305519962105, -1.163578551645441550, 0.4182417262808777458 ) ) ;
#20173 = CARTESIAN_POINT ( 'NONE',  ( -0.1613545236348712109, 0.5011730501305514673, 0.3493272269784499229 ) ) ;
#20174 = DIRECTION ( 'NONE',  ( 0.000000000000000000, 0.3090169943749439541, -0.9510565162951547524 ) ) ;
#20175 = CARTESIAN_POINT ( 'NONE',  ( 0.07216878364870311924, 0.05141091571461162829, 0.1249999999999999029 ) ) ;
#20176 = DIRECTION ( 'NONE',  ( 0.000000000000000000, 0.000000000000000000, -1.000000000000000000 ) ) ;
#20177 = DIRECTION ( 'NONE',  ( 7.771561172376107616E-16, -7.170354002788761615E-17, 1.000000000000000000 ) ) ;
#20178 = CALENDAR_DATE ( 2026, 13, 10 ) ;
#20179 = B_SPLINE_CURVE_WITH_KNOTS ( 'NONE', 3,
 ( #5424, #12026, #18388, #31544, #22515, #34642, #22312, #10551 ),
 .UNSPECIFIED., .F., .F.,
 ( 4, 2, 2, 4 ),
 ( 0.000000000000000000, 0.0002979882110954391503, 0.0005959764221908783006, 0.001191952844381744675 ),
 .UNSPECIFIED. ) ;
#20180 = CARTESIAN_POINT ( 'NONE',  ( 0.3812246895800440738, -1.141621232065750391, 0.4312472505867336325 ) ) ;
#20181 = CARTESIAN_POINT ( 'NONE',  ( 0.1799323859991091290, -0.4957562479442227388, 0.1245508302704903536 ) ) ;
#20182 = DIRECTION ( 'NONE',  ( -0.4999551463232371762, 0.8660512985181134660, -0.000000000000000000 ) ) ;
#20183 = LINE ( 'NONE', #38486, #34355 ) ;
#20184 = CARTESIAN_POINT ( 'NONE',  ( 0.3923243630925510872, -1.966611948492501316, -0.4968729097670202544 ) ) ;
#20185 = CARTESIAN_POINT ( 'NONE',  ( 0.2969171742742482412, -1.658742054446402658, 0.8971516434728256106 ) ) ;
#20186 = CARTESIAN_POINT ( 'NONE',  ( 0.04154009738085454734, -0.01731731106881185395, -0.4700109389422704731 ) ) ;
#20187 = ORIENTED_EDGE ( 'NONE', *, *, #28866, .T. ) ;
#20188 = VERTEX_POINT ( 'NONE', #25388 ) ;
#20189 =( BOUNDED_SURFACE ( )  B_SPLINE_SURFACE ( 3, 2, ( 
 ( #31581, #13272, #10389 ),
 ( #25437, #28293, #9582 ),
 ( #34673, #9777, #6480 ),
 ( #19461, #31995, #37969 ),
 ( #22349, #22764, #6678 ),
 ( #19255, #31796, #3613 ),
 ( #3807, #27039, #10581 ),
 ( #4592, #17162, #32383 ),
 ( #7702, #39570, #11403 ),
 ( #13670, #32598, #10800 ),
 ( #4411, #26658, #23971 ),
 ( #29714, #23760, #36502 ),
 ( #29932, #4800, #1774 ),
 ( #36087, #23157, #20676 ),
 ( #1558, #19852, #11013 ),
 ( #33212, #29323, #4208 ),
 ( #23569, #16774, #1168 ),
 ( #7486, #39187, #14284 ),
 ( #7889, #14078, #30126 ),
 ( #17584, #26233, #5017 ),
 ( #20461, #32993, #35688 ),
 ( #38754, #20069, #17374 ) ),
 .UNSPECIFIED., .F., .F., .T. ) 
 B_SPLINE_SURFACE_WITH_KNOTS ( ( 4, 2, 2, 2, 2, 2, 2, 2, 2, 2, 4 ),
 ( 3, 3 ),
 ( 0.002013519961495848724, 0.002780892266055755638, 0.003548264570615662986, 0.004315636875175570333, 0.004699323027455524007, 0.005083009179735476814, 0.005466695332015429620, 0.005850381484295383294, 0.006617753788855290642, 0.007385126093415197990, 0.008152498397975105338 ),
 ( 0.000000000000000000, 1.000000000000000000 ),
 .UNSPECIFIED. ) 
 GEOMETRIC_REPRESENTATION_ITEM ( )  RATIONAL_B_SPLINE_SURFACE ( (
 ( 1.000000000000000000, 0.7283825911960385424, 1.000000000000000000),
 ( 1.000000000000000000, 0.7404375345929280483, 1.000000000000000000),
 ( 1.000000000000000000, 0.7521483142432979774, 1.000000000000000000),
 ( 1.000000000000000000, 0.7744460733779491290, 1.000000000000000000),
 ( 1.000000000000000000, 0.7845612039384242120, 1.000000000000000000),
 ( 1.000000000000000000, 0.8022035258259876400, 1.000000000000000000),
 ( 1.000000000000000000, 0.8093965293318987619, 1.000000000000000000),
 ( 1.000000000000000000, 0.8169028692726829632, 1.000000000000000000),
 ( 1.000000000000000000, 0.8188329634863246165, 1.000000000000000000),
 ( 1.000000000000000000, 0.8214004505364141950, 1.000000000000000000),
 ( 1.000000000000000000, 0.8220602406260524297, 1.000000000000000000),
 ( 1.000000000000000000, 0.8220736605436118616, 1.000000000000000000),
 ( 1.000000000000000000, 0.8214126668415132615, 1.000000000000000000),
 ( 1.000000000000000000, 0.8188520474558848017, 1.000000000000000000),
 ( 1.000000000000000000, 0.8169545908333680773, 1.000000000000000000),
 ( 1.000000000000000000, 0.8094771004221105182, 1.000000000000000000),
 ( 1.000000000000000000, 0.8022723753809029024, 1.000000000000000000),
 ( 1.000000000000000000, 0.7845733350635966108, 1.000000000000000000),
 ( 1.000000000000000000, 0.7744472902495156408, 1.000000000000000000),
 ( 1.000000000000000000, 0.7522916829161578889, 1.000000000000000000),
 ( 1.000000000000000000, 0.7403553004667213777, 1.000000000000000000),
 ( 1.000000000000000000, 0.7283825911960410959, 1.000000000000000000) ) ) 
 REPRESENTATION_ITEM ( '' )  SURFACE ( )  );
#20190 = CARTESIAN_POINT ( 'NONE',  ( 2.845524969051194536E-18, -0.2899999999999993694, 0.04249999999999928141 ) ) ;
#20191 = ORIENTED_EDGE ( 'NONE', *, *, #8886, .F. ) ;
#20192 = DIRECTION ( 'NONE',  ( 0.000000000000000000, 0.000000000000000000, 1.000000000000000000 ) ) ;
#20193 = CARTESIAN_POINT ( 'NONE',  ( 0.6027832162698157914, -1.482621114427892461, 0.5983148804162514711 ) ) ;
#20195 = VERTEX_POINT ( 'NONE', #37920 ) ;
#20194 = CARTESIAN_POINT ( 'NONE',  ( -0.0007010309512375748758, -0.7626727799179832123, -0.004770403981119245192 ) ) ;
#20197 = ORIENTED_EDGE ( 'NONE', *, *, #7273, .F. ) ;
#20196 = ORIENTED_EDGE ( 'NONE', *, *, #13996, .F. ) ;
#20198 = CARTESIAN_POINT ( 'NONE',  ( 0.5609749049919212638, -1.322492582006539852, 0.8902790116251644292 ) ) ;
#20199 = ORIENTED_EDGE ( 'NONE', *, *, #18352, .F. ) ;
#20200 = CARTESIAN_POINT ( 'NONE',  ( -0.01396963725348175298, -0.5351778444009501756, 0.2100693574405696207 ) ) ;
#20202 = CARTESIAN_POINT ( 'NONE',  ( -0.2399999999999999079, -2.845511416290244622, -0.3415338532332813926 ) ) ;
#20201 = CARTESIAN_POINT ( 'NONE',  ( 0.04285561529640833506, 0.4433460678679726485, 0.2197428102802088945 ) ) ;
#20203 = CARTESIAN_POINT ( 'NONE',  ( 0.6335899703864817933, -1.596177751663389710, -0.4443638777805609119 ) ) ;
#20204 = DATE_TIME_ROLE ( 'classification_date' ) ;
#20205 = CARTESIAN_POINT ( 'NONE',  ( 0.3139458383965972321, -1.186049307970273858, -0.5155029497116575543 ) ) ;
#20207 = EDGE_LOOP ( 'NONE', ( #36735, #20158, #19223 ) ) ;
#20206 = ORIENTED_EDGE ( 'NONE', *, *, #31218, .T. ) ;
#20208 = CARTESIAN_POINT ( 'NONE',  ( 0.1095666333324003955, -0.8145518545241268171, 0.3913258102692879770 ) ) ;
#20209 = B_SPLINE_CURVE_WITH_KNOTS ( 'NONE', 3,
 ( #6724, #16006, #19505, #10241, #13527, #38608, #25885, #10430, #28552, #19298, #32035, #13313, #19686, #26092, #22990, #6327 ),
 .UNSPECIFIED., .F., .F.,
 ( 4, 2, 2, 2, 2, 2, 2, 4 ),
 ( 0.000000000000000000, 5.224492126191339130E-05, 0.0001044898425238267826, 0.0002089796850476577665, 0.0004179593700953283266, 0.0008359187401906626163, 0.001671837480381325883, 0.003343674960762656970 ),
 .UNSPECIFIED. ) ;
#20210 = CARTESIAN_POINT ( 'NONE',  ( 0.1075258522074294676, -1.346637391717543375, 0.6997241829952332015 ) ) ;
#20211 = CARTESIAN_POINT ( 'NONE',  ( 0.09179313224142107708, -0.5838716517235741366, 0.2326204640114538647 ) ) ;
#20212 = CARTESIAN_POINT ( 'NONE',  ( 0.5027379836985736983, -1.456623547386490136, 0.7738150853535875617 ) ) ;
#20213 = CARTESIAN_POINT ( 'NONE',  ( 0.1959931128787035237, -0.5695994422963300829, 0.3097654547218591237 ) ) ;
#20214 = CARTESIAN_POINT ( 'NONE',  ( 0.4209655804235680754, -1.724695148018828839, -0.5155029497116575543 ) ) ;
#20215 = CARTESIAN_POINT ( 'NONE',  ( 0.6859986618141611370, -1.527025669111474526, 0.4781287526575291325 ) ) ;
#20216 = CARTESIAN_POINT ( 'NONE',  ( 0.3529334898677526922, -1.741231243591691014, 0.5928160496120983280 ) ) ;
#20217 = CARTESIAN_POINT ( 'NONE',  ( 0.6655612380268166595, -1.561523951251945874, 0.5631882573506850065 ) ) ;
#20218 = ADVANCED_FACE ( 'NONE', ( #12410 ), #34208, .F. ) ;
#20219 = EDGE_CURVE ( 'NONE', #39958, #18975, #27842, .T. ) ;
#20220 = AXIS2_PLACEMENT_3D ( 'NONE', #352, #23505, #12854 ) ;
#20221 = FACE_OUTER_BOUND ( 'NONE', #26360, .T. ) ;
#20222 = EDGE_CURVE ( 'NONE', #849, #3787, #34557, .T. ) ;
#20223 = FACE_OUTER_BOUND ( 'NONE', #21515, .T. ) ;
#20224 = CARTESIAN_POINT ( 'NONE',  ( -0.2746410161513779258, -2.845511416290244622, -0.3415338532332813926 ) ) ;
#20225 = CARTESIAN_POINT ( 'NONE',  ( -0.0001519008987895401682, -0.8203875425039895974, -0.06507672622562246656 ) ) ;
#20226 = CARTESIAN_POINT ( 'NONE',  ( 0.5836794880485997039, -1.483121240051231471, 0.6621808355073148800 ) ) ;
#20227 = EDGE_CURVE ( 'NONE', #22283, #2874, #32584, .T. ) ;
#20228 = CARTESIAN_POINT ( 'NONE',  ( 0.4971920908461615607, -1.080069027881642052, 0.4687417262808780127 ) ) ;
#20229 = DIRECTION ( 'NONE',  ( -1.000000000000000000, -0.000000000000000000, -0.000000000000000000 ) ) ;
#20230 = EDGE_CURVE ( 'NONE', #38543, #39260, #8803, .T. ) ;
#20231 = CARTESIAN_POINT ( 'NONE',  ( 0.1230419690069037980, -1.441173760443279050, 0.5802947806848592904 ) ) ;
#20232 = CARTESIAN_POINT ( 'NONE',  ( 0.4373890596466497582, -1.046786911024660593, 0.6537231983888873721 ) ) ;
#20233 = PERSON_AND_ORGANIZATION_ROLE ( 'creator' ) ;
#20234 = CARTESIAN_POINT ( 'NONE',  ( 0.2888622377148890585, -0.7373900025806978675, 0.6684008680139050806 ) ) ;
#20235 = DIRECTION ( 'NONE',  ( -0.4999551463232372317, 0.8660512985181135770, -0.000000000000000000 ) ) ;
#20236 = FACE_OUTER_BOUND ( 'NONE', #8330, .T. ) ;
#20237 = EDGE_CURVE ( 'NONE', #22886, #20248, #6621, .T. ) ;
#20238 = ORIENTED_EDGE ( 'NONE', *, *, #37133, .F. ) ;
#20239 = DIRECTION ( 'NONE',  ( 1.000000000000000000, 0.000000000000000000, 0.000000000000000000 ) ) ;
#20240 = PRODUCT_RELATED_PRODUCT_CATEGORY ( 'detail', '', ( #19635 ) ) ;
#20241 = CARTESIAN_POINT ( 'NONE',  ( 0.003262416371409640210, -0.5547458529584512466, 0.2870733929886844504 ) ) ;
#20242 = CARTESIAN_POINT ( 'NONE',  ( 0.6445923553667830541, -1.422221564968557894, -0.6250000000000000000 ) ) ;
#20243 = EDGE_LOOP ( 'NONE', ( #705, #34178, #15923, #8895 ) ) ;
#20244 = CARTESIAN_POINT ( 'NONE',  ( 0.08402031424619307853, 0.05739311687334415490, -0.1044725468576913618 ) ) ;
#20245 = AXIS2_PLACEMENT_3D ( 'NONE', #17616, #14121, #8141 ) ;
#20246 = CARTESIAN_POINT ( 'NONE',  ( 0.4241633753480167357, -0.9987333192354345135, 0.7764642562231158784 ) ) ;
#20248 = VERTEX_POINT ( 'NONE', #13219 ) ;
#20247 = VERTEX_POINT ( 'NONE', #15903 ) ;
#20249 = CARTESIAN_POINT ( 'NONE',  ( 0.03182674568678287019, -1.845213679978619403, -0.6754919065654066967 ) ) ;
#20250 = EDGE_LOOP ( 'NONE', ( #7347, #2568, #23293, #19393 ) ) ;
#20251 = CARTESIAN_POINT ( 'NONE',  ( 0.1991480113865206902, -2.054949600705703983, -0.6841806413415666421 ) ) ;
#20252 = CARTESIAN_POINT ( 'NONE',  ( 0.1876095839365584383, -1.270310460104812744, 0.4182417262808780234 ) ) ;
#20253 = CARTESIAN_POINT ( 'NONE',  ( -0.05616044724337389965, 0.4336395721329084907, -0.1516614036261209608 ) ) ;
#20254 = B_SPLINE_CURVE_WITH_KNOTS ( 'NONE', 3,
 ( #16941, #32353, #14049, #26818, #20036, #1925, #17135, #4770, #32568, #39347, #26627, #10366, #13834, #23542, #11168, #22928, #4384, #26408, #29482, #7858, #17344, #29901 ),
 .UNSPECIFIED., .F., .F.,
 ( 4, 2, 2, 2, 2, 2, 2, 2, 2, 2, 4 ),
 ( 0.001187924609274661029, 0.001905614920410501206, 0.002623305231546341383, 0.003340995542682181560, 0.004058685853818020869, 0.004776376164953861914, 0.005494066476089702090, 0.005852911631657626082, 0.006211756787225550074, 0.006570601942793475800, 0.006929447098361399791 ),
 .UNSPECIFIED. ) ;
#20255 = VERTEX_POINT ( 'NONE', #3155 ) ;
#20256 = CARTESIAN_POINT ( 'NONE',  ( 0.1045998439320173501, -1.275504460590098033, 0.5978142315846559640 ) ) ;
#20257 = CARTESIAN_POINT ( 'NONE',  ( 0.1167100500347143938, -0.7341236526051606592, 0.4239359085789457526 ) ) ;
#20258 = CARTESIAN_POINT ( 'NONE',  ( 0.2362853573231588344, -1.416426150276697937, 1.031910927484303020 ) ) ;
#20259 = CARTESIAN_POINT ( 'NONE',  ( 0.08712330498557509240, -0.5673539409833764369, 0.2525723869550539069 ) ) ;
#20261 = DIRECTION ( 'NONE',  ( 0.4999551463232372317, -0.8660512985181135770, 0.000000000000000000 ) ) ;
#20260 = DIRECTION ( 'NONE',  ( 0.000000000000000000, 0.8834504764629500517, 0.4685245517978610108 ) ) ;
#20262 = CARTESIAN_POINT ( 'NONE',  ( 0.2055788005570233501, -0.9799573814450284193, 0.5334445023266595198 ) ) ;
#20263 = ORIENTED_EDGE ( 'NONE', *, *, #5244, .F. ) ;
#20264 = EDGE_LOOP ( 'NONE', ( #26972, #36621, #4938, #30814, #37941, #33400, #1324 ) ) ;
#20265 = CARTESIAN_POINT ( 'NONE',  ( 0.6386829715298258936, -1.585896454429429392, -0.5957020523142678714 ) ) ;
#20266 = CARTESIAN_POINT ( 'NONE',  ( 0.2013267960816771396, -0.5279965997290305690, 0.3764562652743823623 ) ) ;
#20267 = CARTESIAN_POINT ( 'NONE',  ( -0.01896968469603060869, 0.2428673116372761231, -0.4598334287537079179 ) ) ;
#20268 = EDGE_CURVE ( 'NONE', #2590, #20994, #13385, .T. ) ;
#20269 = CARTESIAN_POINT ( 'NONE',  ( -0.08408070219615630669, -0.09959325338431362917, 0.3749999999999960587 ) ) ;
#20270 = EDGE_CURVE ( 'NONE', #9403, #16208, #6824, .T. ) ;
#20271 = CARTESIAN_POINT ( 'NONE',  ( -0.1999999999999999833, 0.5182417262804744906, 0.08500000000000017264 ) ) ;
#20272 = ADVANCED_FACE ( 'NONE', ( #15697 ), #14292, .T. ) ;
#20273 = FACE_BOUND ( 'NONE', #2390, .T. ) ;
#20274 = CARTESIAN_POINT ( 'NONE',  ( 0.6182635900321699074, -1.298039841913932513, 0.5932631914600888789 ) ) ;
#20275 = DIRECTION ( 'NONE',  ( -8.881784197001246407E-16, 2.361472542561082612E-16, -1.000000000000000000 ) ) ;
#20276 = CARTESIAN_POINT ( 'NONE',  ( 0.04870459694554082897, -1.634362537833374818, -0.3424663835692939307 ) ) ;
#20277 = CARTESIAN_POINT ( 'NONE',  ( 0.5605867575437347705, -1.621001144914625991, -0.5473203437262896820 ) ) ;
#20278 = ORIENTED_EDGE ( 'NONE', *, *, #177, .T. ) ;
#20279 = CARTESIAN_POINT ( 'NONE',  ( 0.2576571872773831262, -0.9936220594909095372, 0.7090459653281796504 ) ) ;
#20280 = CARTESIAN_POINT ( 'NONE',  ( 0.3244517107433588787, -1.756899521929603081, 0.5670097850713597953 ) ) ;
#20281 = CARTESIAN_POINT ( 'NONE',  ( -0.05269191099235946696, -0.2790572191958481385, -0.3764802596566364512 ) ) ;
#20282 = EDGE_CURVE ( 'NONE', #13057, #33645, #21422, .T. ) ;
#20283 = VERTEX_POINT ( 'NONE', #27773 ) ;
#20284 = CARTESIAN_POINT ( 'NONE',  ( 0.4956832342913312650, -1.106712120975469782, 0.6967973883462599272 ) ) ;
#20285 = CARTESIAN_POINT ( 'NONE',  ( -0.03650577977170588184, 0.08362514765351788948, -0.5048437183011776908 ) ) ;
#20286 = CARTESIAN_POINT ( 'NONE',  ( 0.3555724811773333660, -1.722873613718818975, -0.4858523300028667613 ) ) ;
#20287 = B_SPLINE_CURVE_WITH_KNOTS ( 'NONE', 3,
 ( #34817, #3346, #32148, #3562 ),
 .UNSPECIFIED., .F., .F.,
 ( 4, 4 ),
 ( 1.891967273893909975E-16, 0.0005779611142783052345 ),
 .UNSPECIFIED. ) ;
#20288 = CARTESIAN_POINT ( 'NONE',  ( 0.4112729528620188146, -1.130284805869275599, 0.4964726040806888840 ) ) ;
#20289 = CARTESIAN_POINT ( 'NONE',  ( 0.03345570897536777333, -0.8438603944194037476, 0.2510648449414971117 ) ) ;
#20290 = EDGE_LOOP ( 'NONE', ( #12534, #27470, #16490, #40162 ) ) ;
#20291 = CARTESIAN_POINT ( 'NONE',  ( 0.04582713223189485013, 0.3361263728083095370, 0.3523178389613185746 ) ) ;
#20292 = CARTESIAN_POINT ( 'NONE',  ( -1.019575837292303166, -0.04310840302197994911, 0.3599999999999993205 ) ) ;
#20293 = CARTESIAN_POINT ( 'NONE',  ( 0.2038749045098602886, -1.364881829950852721, 0.4182417262808790226 ) ) ;
#20294 = DIRECTION ( 'NONE',  ( 0.9378410757839552581, -0.1072489841977715685, -0.3300784330442382841 ) ) ;
#20295 = CARTESIAN_POINT ( 'NONE',  ( 0.4793885211484971709, -1.257667511030738927, 0.5965085062872911292 ) ) ;
#20297 = CARTESIAN_POINT ( 'NONE',  ( 0.3545325911476117642, -1.827139849489873402, -0.4887235082572288780 ) ) ;
#20296 = DIRECTION ( 'NONE',  ( 4.930380657631323784E-32, 0.7472307839325098566, 0.6645646360916346307 ) ) ;
#20298 = CARTESIAN_POINT ( 'NONE',  ( 0.3142644354089449421, -0.9846788231241262457, 0.5762604841115940291 ) ) ;
#20299 = VERTEX_POINT ( 'NONE', #18313 ) ;
#20300 = CARTESIAN_POINT ( 'NONE',  ( 0.1909286924077255032, -1.257064795538239022, -0.4125659523519144001 ) ) ;
#20301 = ORIENTED_EDGE ( 'NONE', *, *, #12667, .F. ) ;
#20302 = CARTESIAN_POINT ( 'NONE',  ( 0.1882219672280248668, -0.6407273034312881421, -0.08446770797961487831 ) ) ;
#20303 = CARTESIAN_POINT ( 'NONE',  ( 0.1929482915730646453, -1.044195424190118571, 0.8266095843266986209 ) ) ;
#20305 = CARTESIAN_POINT ( 'NONE',  ( 0.08510361377861434817, -0.8106636051554854117, 0.1454306519311501233 ) ) ;
#20304 = CARTESIAN_POINT ( 'NONE',  ( 0.08759942705067334801, -0.6779500844790127267, 0.001722161171260314571 ) ) ;
#20306 = DIRECTION ( 'NONE',  ( 0.8660512985181134660, 0.4999551463232372317, 0.000000000000000000 ) ) ;
#20307 = VERTEX_POINT ( 'NONE', #2677 ) ;
#20308 = CARTESIAN_POINT ( 'NONE',  ( 0.4559719632891929830, -1.698713290701216350, -0.5155029497116575543 ) ) ;
#20309 = CARTESIAN_POINT ( 'NONE',  ( 0.5743670735733531485, -1.499265677782189332, 0.5819334991045758132 ) ) ;
#20310 = VERTEX_POINT ( 'NONE', #2484 ) ;
#20311 = CYLINDRICAL_SURFACE ( 'NONE', #9271, 0.1000000000000000194 ) ;
#20312 = CARTESIAN_POINT ( 'NONE',  ( 0.05076679145662038595, -0.4330939261214921121, 0.1921033382362652697 ) ) ;
#20313 = ADVANCED_FACE ( 'NONE', ( #18509 ), #3093, .T. ) ;
#20314 =( BOUNDED_SURFACE ( )  B_SPLINE_SURFACE ( 3, 2, ( 
 ( #5483, #2619, #27713 ),
 ( #7958, #17640, #14763 ),
 ( #33274, #8782, #24233 ),
 ( #24044, #27326, #39857 ) ),
 .UNSPECIFIED., .F., .F., .F. ) 
 B_SPLINE_SURFACE_WITH_KNOTS ( ( 4, 4 ),
 ( 3, 3 ),
 ( 0.001772558173964181201, 0.002238911299073404176 ),
 ( 0.000000000000000000, 1.000000000000000000 ),
 .UNSPECIFIED. ) 
 GEOMETRIC_REPRESENTATION_ITEM ( )  RATIONAL_B_SPLINE_SURFACE ( (
 ( 1.000000000000000000, 0.4461867090274512226, 1.000000000000000000),
 ( 1.000000000000000000, 0.4650446221766792454, 1.000000000000000000),
 ( 1.000000000000000000, 0.4838440862043267288, 1.000000000000000000),
 ( 1.000000000000000000, 0.5022121722253944931, 1.000000000000000000) ) ) 
 REPRESENTATION_ITEM ( '' )  SURFACE ( )  );
#20315 = CARTESIAN_POINT ( 'NONE',  ( 0.3873689179426565432, -1.755636530304691689, -0.4507512901387274451 ) ) ;
#20316 = PRODUCT_DEFINITION_SHAPE ( 'NONE', 'NONE',  #40663 ) ;
#20317 = CARTESIAN_POINT ( 'NONE',  ( 0.2153918940804837590, -1.242713953115129666, 0.4559406856927734619 ) ) ;
#20318 = EDGE_CURVE ( 'NONE', #27170, #23955, #12142, .T. ) ;
#20319 = CARTESIAN_POINT ( 'NONE',  ( -0.1707605070207437459, 0.4977265752128576248, 0.1434892898517915460 ) ) ;
#20320 = CARTESIAN_POINT ( 'NONE',  ( 0.05083674528491973627, -0.04859289555129253646, 0.4711018118971379010 ) ) ;
#20321 = CARTESIAN_POINT ( 'NONE',  ( 0.2978499211271074532, -0.7548715063715667473, 0.6844903506759184575 ) ) ;
#20322 = DIRECTION ( 'NONE',  ( 0.8660512985181135770, 0.4999551463232370652, 0.000000000000000000 ) ) ;
#20323 = DIRECTION ( 'NONE',  ( 1.000000000000000000, 0.000000000000000000, 0.000000000000000000 ) ) ;
#20324 = ADVANCED_FACE ( 'NONE', ( #18109, #37630 ), #21615, .F. ) ;
#20325 = B_SPLINE_CURVE_WITH_KNOTS ( 'NONE', 3,
 ( #40532, #15838, #34755, #472, #21431, #4302, #10074, #28798, #32476, #38655, #35776, #32084, #17056, #10293, #4086, #23250, #13957, #29409 ),
 .UNSPECIFIED., .F., .F.,
 ( 4, 2, 2, 2, 2, 2, 2, 2, 4 ),
 ( -0.002633528389679827900, -0.001975271857855798781, -0.001317015326031769880, -0.0006587587942077409789, -5.022623837118607437E-07, 0.0006577542694403172574, 0.001316010801264345942, 0.001974267333088375494, 0.002632523864912404178 ),
 .UNSPECIFIED. ) ;
#20326 = CARTESIAN_POINT ( 'NONE',  ( 0.6163751027920442160, -1.623333184780543448, -0.5127481645887516093 ) ) ;
#20327 = CARTESIAN_POINT ( 'NONE',  ( 0.000000000000000000, 0.000000000000000000, 0.000000000000000000 ) ) ;
#20328 = CARTESIAN_POINT ( 'NONE',  ( 1.171686751960861702E-18, 6.434085166993908708E-18, 0.01750000000000000513 ) ) ;
#20329 = CARTESIAN_POINT ( 'NONE',  ( 0.6960330676580404052, -1.427191473012519918, 0.4398509372606123069 ) ) ;
#20330 = B_SPLINE_CURVE_WITH_KNOTS ( 'NONE', 3,
 ( #27250, #5403, #39780, #36496 ),
 .UNSPECIFIED., .F., .F.,
 ( 4, 4 ),
 ( 3.469446951953614189E-18, 0.0007111050983136056993 ),
 .UNSPECIFIED. ) ;
#20331 = CARTESIAN_POINT ( 'NONE',  ( -0.3000000000000000999, -2.183180860297908144, -0.2991170932241127844 ) ) ;
#20332 = DIRECTION ( 'NONE',  ( -0.9574652249354426159, 0.000000000000000000, -0.2885486840020622390 ) ) ;
#20333 = CARTESIAN_POINT ( 'NONE',  ( 0.5616368264987144920, -1.585529113978794591, -0.5096405943624068291 ) ) ;
#20334 = EDGE_CURVE ( 'NONE', #5233, #1162, #9451, .T. ) ;
#20335 = DIRECTION ( 'NONE',  ( 0.000000000000000000, 0.000000000000000000, -1.000000000000000000 ) ) ;
#20336 = DIRECTION ( 'NONE',  ( -2.682900528199988315E-31, 0.9510565162951527540, -0.3090169943749503378 ) ) ;
#20337 = CARTESIAN_POINT ( 'NONE',  ( -0.03642997641689297433, -0.3645929376994312965, 0.3593586258117719145 ) ) ;
#20338 = EDGE_CURVE ( 'NONE', #6171, #28384, #11964, .T. ) ;
#20339 = VERTEX_POINT ( 'NONE', #37426 ) ;
#20340 = VERTEX_POINT ( 'NONE', #18934 ) ;
#20341 = CARTESIAN_POINT ( 'NONE',  ( 0.07043814880410684265, -1.334972480813831242, 0.5056242588139928662 ) ) ;
#20342 = CARTESIAN_POINT ( 'NONE',  ( 0.3740153396470256575, -1.763885720033750992, -0.5728934586661176276 ) ) ;
#20343 = EDGE_LOOP ( 'NONE', ( #37841, #27571, #35223, #37898, #5662, #31870 ) ) ;
#20344 = DIRECTION ( 'NONE',  ( 1.000000000000000000, 1.445897915516965072E-15, -8.881784197001242463E-16 ) ) ;
#20345 = CARTESIAN_POINT ( 'NONE',  ( -0.02000000000000000042, -1.622350287959229087, -0.08960079202753243321 ) ) ;
#20346 = B_SPLINE_CURVE_WITH_KNOTS ( 'NONE', 3,
 ( #39437, #36351, #7764, #4870 ),
 .UNSPECIFIED., .F., .F.,
 ( 4, 4 ),
 ( -2.702335329567562820E-05, 0.0001957598036966991110 ),
 .UNSPECIFIED. ) ;
#20347 = CARTESIAN_POINT ( 'NONE',  ( 0.5380213988856127338, -1.358208888136053005, 0.7378845647473735170 ) ) ;
#20349 = EDGE_LOOP ( 'NONE', ( #9895, #4529, #38380 ) ) ;
#20348 = CARTESIAN_POINT ( 'NONE',  ( -0.1588702854552149490, 0.4932535771925480872, 0.1179163363090275640 ) ) ;
#20350 = CARTESIAN_POINT ( 'NONE',  ( 0.1874843899254543811, -0.7932266022496337055, 0.2338244398510780642 ) ) ;
#20351 = CARTESIAN_POINT ( 'NONE',  ( 0.02953079040095687308, 0.5250338024619264354, -0.07436286310882528339 ) ) ;
#20352 = ORIENTED_EDGE ( 'NONE', *, *, #12927, .T. ) ;
#20353 = DIRECTION ( 'NONE',  ( 0.8660512985181135770, 0.4999551463232370652, 0.000000000000000000 ) ) ;
#20354 = CARTESIAN_POINT ( 'NONE',  ( 0.3266909551894673913, -1.639055458000120868, 0.5694230527446741963 ) ) ;
#20356 = CARTESIAN_POINT ( 'NONE',  ( 0.1873251789708756665, -0.5721470344398987828, 0.02377237672441944241 ) ) ;
#20355 = CARTESIAN_POINT ( 'NONE',  ( 0.7015756474355604455, -1.490181709399133858, 0.5009006423618302950 ) ) ;
#20357 = CARTESIAN_POINT ( 'NONE',  ( 0.05563540667800927902, -1.335270441939011121, 0.5197417262808780025 ) ) ;
#20358 = CARTESIAN_POINT ( 'NONE',  ( 0.1519263329367288584, -1.326104206834778143, -0.3123460348997796343 ) ) ;
#20359 = ORIENTED_EDGE ( 'NONE', *, *, #14752, .T. ) ;
#20360 = DIRECTION ( 'NONE',  ( 0.000000000000000000, 0.000000000000000000, -1.000000000000000000 ) ) ;
#20361 = CARTESIAN_POINT ( 'NONE',  ( 0.005199229819682637393, -1.801804716922572602, -0.6418151134160050564 ) ) ;
#20362 = DIRECTION ( 'NONE',  ( 0.8660512985181132439, 0.4999551463232376758, 0.000000000000000000 ) ) ;
#20363 = CARTESIAN_POINT ( 'NONE',  ( 0.4366195600600660254, -1.227215273123700712, 0.6046990178492395174 ) ) ;
#20364 = LINE ( 'NONE', #33491, #855 ) ;
#20365 = EDGE_CURVE ( 'NONE', #17036, #37027, #15355, .T. ) ;
#20366 = CARTESIAN_POINT ( 'NONE',  ( -0.1653405084325548779, 0.5136906775330246644, 0.3358539725464951275 ) ) ;
#20367 = EDGE_CURVE ( 'NONE', #37987, #19134, #36374, .T. ) ;
#20368 = DIRECTION ( 'NONE',  ( -7.771561172376107616E-16, 7.170354002788761615E-17, -1.000000000000000000 ) ) ;
#20369 = LINE ( 'NONE', #26153, #16053 ) ;
#20370 = DIRECTION ( 'NONE',  ( 1.000000000000000000, 2.341930812374887555E-31, -1.664003471950578127E-31 ) ) ;
#20371 = CARTESIAN_POINT ( 'NONE',  ( -0.2399999999999999079, -2.183180860297908144, -0.4937760292030871079 ) ) ;
#20372 = DIRECTION ( 'NONE',  ( 0.4999999999999997224, -0.3085698060533127451, -0.8091876635195454082 ) ) ;
#20373 = DATE_AND_TIME ( #20178, #31839 ) ;
#20374 = CARTESIAN_POINT ( 'NONE',  ( 0.03449693227200471141, -1.144353617540043722, 0.6732275831407835698 ) ) ;
#20375 = CARTESIAN_POINT ( 'NONE',  ( 0.1804100887215605853, -0.4972044085177187989, 0.1208670693178307276 ) ) ;
#20376 = DIRECTION ( 'NONE',  ( -1.387778780781449423E-15, 6.545052484820649979E-16, -1.000000000000000000 ) ) ;
#20377 = CARTESIAN_POINT ( 'NONE',  ( 0.1499999999999994948, 0.3688619771572980710, 0.3775276577326925898 ) ) ;
#20378 = CARTESIAN_POINT ( 'NONE',  ( 0.4044319497911501027, -1.745786362538516823, -0.5913871057305363221 ) ) ;
#20379 = DIRECTION ( 'NONE',  ( 0.000000000000000000, -0.9510565162951634122, -0.3090169943749168646 ) ) ;
#20380 = CIRCLE ( 'NONE', #10585, 0.02999999999999998154 ) ;
#20381 = DIRECTION ( 'NONE',  ( -0.3468893892380660038, -0.7770416411310684390, -0.5252371270030113948 ) ) ;
#20382 = ORIENTED_EDGE ( 'NONE', *, *, #1175, .T. ) ;
#20383 = VERTEX_POINT ( 'NONE', #10065 ) ;
#20384 = AXIS2_PLACEMENT_3D ( 'NONE', #29435, #32508, #16477 ) ;
#20385 = CARTESIAN_POINT ( 'NONE',  ( 0.1882052571625662252, -0.5110766197885958650, 0.09799269069308937097 ) ) ;
#20386 = VERTEX_POINT ( 'NONE', #7354 ) ;
#20387 = FACE_OUTER_BOUND ( 'NONE', #21519, .T. ) ;
#20388 = CARTESIAN_POINT ( 'NONE',  ( 0.6019577307062530247, -1.483131278876760550, 0.5728282478110194864 ) ) ;
#20390 = VERTEX_POINT ( 'NONE', #28593 ) ;
#20389 = CARTESIAN_POINT ( 'NONE',  ( -0.0001062047391421509833, -0.6980687014391792067, -0.01370441279489919249 ) ) ;
#20391 = ORIENTED_EDGE ( 'NONE', *, *, #10693, .F. ) ;
#20392 = CARTESIAN_POINT ( 'NONE',  ( 0.3100641407756268286, -1.188533344716862006, 0.5383015422848057563 ) ) ;
#20393 = EDGE_LOOP ( 'NONE', ( #21275, #5150, #39003, #12550 ) ) ;
#20394 = CARTESIAN_POINT ( 'NONE',  ( -0.01398755374478900804, -0.5253281656772126329, 0.1457185332388696575 ) ) ;
#20396 = CARTESIAN_POINT ( 'NONE',  ( -0.02000000000000000042, -2.320036485105098301, -0.2941690811493925528 ) ) ;
#20395 = CARTESIAN_POINT ( 'NONE',  ( -0.03868649100028175719, -0.4624880946332493026, -0.1149381524902386292 ) ) ;
#20397 = CARTESIAN_POINT ( 'NONE',  ( 0.000000000000000000, 0.1428018198284763673, -0.2638325989215043466 ) ) ;
#20398 = PERSON_AND_ORGANIZATION_ROLE ( 'classification_officer' ) ;
#20399 = CARTESIAN_POINT ( 'NONE',  ( -0.001266333596127353555, -0.7404579356088998310, -0.06462206035643762447 ) ) ;
#20401 = ORIENTED_EDGE ( 'NONE', *, *, #39307, .F. ) ;
#20400 = ORIENTED_EDGE ( 'NONE', *, *, #35353, .F. ) ;
#20402 = CARTESIAN_POINT ( 'NONE',  ( 0.08704056524540265682, -0.8139669836441042472, 0.2169878034514332588 ) ) ;
#20403 = CARTESIAN_POINT ( 'NONE',  ( 0.1188311809963038257, -1.413182374742705028, 0.5829798790863079949 ) ) ;
#20404 = CARTESIAN_POINT ( 'NONE',  ( 0.09049813587943421334, -0.5721903250205445657, 0.1963611786150708527 ) ) ;
#20405 = CARTESIAN_POINT ( 'NONE',  ( 0.5530767995133970549, -1.511202523187898272, 0.5748300795346157344 ) ) ;
#20406 = CARTESIAN_POINT ( 'NONE',  ( 0.02528307276850410429, -1.032232763260760411, 0.5721851376505144859 ) ) ;
#20407 = CARTESIAN_POINT ( 'NONE',  ( -0.02000000000000000042, -2.183180860297908144, -0.4937760292030871079 ) ) ;
#20408 = LINE ( 'NONE', #4746, #30319 ) ;
#20409 = CIRCLE ( 'NONE', #36132, 0.1749999999999999889 ) ;
#20410 = CARTESIAN_POINT ( 'NONE',  ( 0.7428087118830455360, -1.516422422578568074, 0.5574800764447178647 ) ) ;
#20411 = DIRECTION ( 'NONE',  ( 0.9998941247116546194, -0.01455087607601020239, 0.0001066420868422379362 ) ) ;
#20412 = DIRECTION ( 'NONE',  ( -0.8660254037844402619, -0.4607757839015039769, -0.1941279912067088165 ) ) ;
#20413 = VECTOR ( 'NONE', #15215, 39.37007874015748143 ) ;
#20414 = CARTESIAN_POINT ( 'NONE',  ( 0.3999999999999788169, -2.042495778117167315, -0.2760839614659731378 ) ) ;
#20415 = CARTESIAN_POINT ( 'NONE',  ( -0.0003284294498005900943, -0.9127994026214639733, 0.03813321986937860675 ) ) ;
#20416 = CARTESIAN_POINT ( 'NONE',  ( 0.4529039210267923887, -1.253808424768705354, 0.8185038725021189787 ) ) ;
#20417 = CONICAL_SURFACE ( 'NONE', #23711, 0.07499999999999991396, 0.6931599075767558293 ) ;
#20418 = CARTESIAN_POINT ( 'NONE',  ( -0.02953079040095693900, -0.4684706630666107263, -0.2484463060367401721 ) ) ;
#20419 = CARTESIAN_POINT ( 'NONE',  ( -0.002083146443013342720, -0.8967360763018593639, 0.1136267619940960899 ) ) ;
#20420 = CARTESIAN_POINT ( 'NONE',  ( 0.4793721953524077151, -1.080656662118478328, 0.6419491832934718367 ) ) ;
#20421 = PERSON_AND_ORGANIZATION ( #28500, #32463 ) ;
#20422 = CARTESIAN_POINT ( 'NONE',  ( 0.1983812210006687116, -0.5262237738225362671, 0.3723155052761787376 ) ) ;
#20423 = CARTESIAN_POINT ( 'NONE',  ( 0.02423924040295065072, 0.06026721965051347329, -0.1249999999999999029 ) ) ;
#20424 = CARTESIAN_POINT ( 'NONE',  ( 0.3110598971219385445, -1.761560204844608624, 0.5688280639540626016 ) ) ;
#20425 = ORIENTED_EDGE ( 'NONE', *, *, #39919, .F. ) ;
#20426 = CARTESIAN_POINT ( 'NONE',  ( -2.112273405726188513E-14, -2.097675824466503691, -0.7286991843995640483 ) ) ;
#20427 = CARTESIAN_POINT ( 'NONE',  ( 0.05790745537833989764, -0.8938553282252756915, 0.7578938048666139515 ) ) ;
#20428 = AXIS2_PLACEMENT_3D ( 'NONE', #30952, #24384, #30755 ) ;
#20429 = CARTESIAN_POINT ( 'NONE',  ( 0.5494268846431774600, -1.650536850169864067, -0.5155029497116575543 ) ) ;
#20431 = ORIENTED_EDGE ( 'NONE', *, *, #4694, .T. ) ;
#20430 = DIRECTION ( 'NONE',  ( -8.881784197001245421E-16, 2.361472542561082612E-16, -1.000000000000000000 ) ) ;
#20432 = CARTESIAN_POINT ( 'NONE',  ( 0.3204139389452045905, -1.755336229099436318, 0.4849083929475462296 ) ) ;
#20433 = CARTESIAN_POINT ( 'NONE',  ( 0.1895831464430141056, -0.5047047246472137205, 0.1457185332388698518 ) ) ;
#20435 = ORIENTED_EDGE ( 'NONE', *, *, #28868, .F. ) ;
#20434 = ORIENTED_EDGE ( 'NONE', *, *, #10505, .T. ) ;
#20436 = CARTESIAN_POINT ( 'NONE',  ( -2.114758357748986011E-14, -2.063353092206445805, -0.6849817048858417579 ) ) ;
#20437 = VECTOR ( 'NONE', #37374, 39.37007874015748854 ) ;
#20438 = EDGE_LOOP ( 'NONE', ( #32972, #3130, #32122, #22897 ) ) ;
#20439 = CARTESIAN_POINT ( 'NONE',  ( 0.1996617404659777606, -2.072851997774555421, -0.6888320016018293357 ) ) ;
#20440 = AXIS2_PLACEMENT_3D ( 'NONE', #6092, #31419, #3220 ) ;
#20441 = CARTESIAN_POINT ( 'NONE',  ( 0.02953079040095687308, -0.3810518745593889922, -0.3687679460475752902 ) ) ;
#20442 = CIRCLE ( 'NONE', #3363, 0.01499999999999997689 ) ;
#20443 = CARTESIAN_POINT ( 'NONE',  ( -0.04947837552028831049, 0.4418396724781329943, -0.1804413675088953339 ) ) ;
#20444 = ORIENTED_EDGE ( 'NONE', *, *, #9477, .T. ) ;
#20445 = DIRECTION ( 'NONE',  ( -1.000000000000000000, -0.000000000000000000, -0.000000000000000000 ) ) ;
#20446 = ADVANCED_FACE ( 'NONE', ( #6554 ), #12747, .F. ) ;
#20447 = CARTESIAN_POINT ( 'NONE',  ( 0.1045684668339736112, -0.6803636310989321645, 0.3644625957350271506 ) ) ;
#20448 = CARTESIAN_POINT ( 'NONE',  ( 0.2160733736694307461, -1.306826138754803912, 1.030613714223332256 ) ) ;
#20449 = CARTESIAN_POINT ( 'NONE',  ( 0.4974923246832697599, -1.542513320629801843, 0.5739867662333766329 ) ) ;
#20451 = DIRECTION ( 'NONE',  ( -0.9998941247116546194, 0.01455087607601020239, -0.0001066420868422379362 ) ) ;
#20450 = CARTESIAN_POINT ( 'NONE',  ( 0.2465969332363348310, -1.554578480253843153, 0.8932696627654338473 ) ) ;
#20452 = CARTESIAN_POINT ( 'NONE',  ( 0.07874391045642013809, -1.016202677645668073, 0.5597170535595098473 ) ) ;
#20453 = VERTEX_POINT ( 'NONE', #16858 ) ;
#20454 = ORIENTED_EDGE ( 'NONE', *, *, #22503, .T. ) ;
#20455 = CARTESIAN_POINT ( 'NONE',  ( 0.6449069409503503936, -1.569348338378467211, -0.6050967068392708592 ) ) ;
#20456 = VECTOR ( 'NONE', #15602, 39.37007874015748854 ) ;
#20457 = CARTESIAN_POINT ( 'NONE',  ( 0.1155307545216270604, -0.4504370356409115317, 0.1913358126256027025 ) ) ;
#20458 = DIRECTION ( 'NONE',  ( -1.000000000000000000, 0.000000000000000000, 0.000000000000000000 ) ) ;
#20459 = ADVANCED_FACE ( 'NONE', ( #9854 ), #35368, .T. ) ;
#20460 = APPLIED_PERSON_AND_ORGANIZATION_ASSIGNMENT ( #12785, #9614, ( #11907 ) ) ;
#20461 = CARTESIAN_POINT ( 'NONE',  ( -0.01896968469603809576, -0.5123777055006339953, -0.08888419526111762670 ) ) ;
#20462 = CARTESIAN_POINT ( 'NONE',  ( -0.1795773455677915076, 0.4580325878418424201, 0.3606502365332835414 ) ) ;
#20463 = AXIS2_PLACEMENT_3D ( 'NONE', #15610, #9631, #6937 ) ;
#20464 = CARTESIAN_POINT ( 'NONE',  ( 0.1042976598065218086, -1.410862685333503563, 0.5472972531283946118 ) ) ;
#20465 = CARTESIAN_POINT ( 'NONE',  ( 0.6053747664524671279, -1.274130884506152084, 0.6672623879134867986 ) ) ;
#20466 = AXIS2_PLACEMENT_3D ( 'NONE', #5845, #21103, #8344 ) ;
#20467 = DIRECTION ( 'NONE',  ( 0.8917998487739612345, 0.000000000000000000, 0.4524301379514188426 ) ) ;
#20468 = AXIS2_PLACEMENT_3D ( 'NONE', #640, #12736, #6751 ) ;
#20469 = CIRCLE ( 'NONE', #10625, 0.08000000000000000167 ) ;
#20470 = CARTESIAN_POINT ( 'NONE',  ( 0.1511623735954494840, -1.326999691097843659, -0.3126952349615497728 ) ) ;
#20471 = CYLINDRICAL_SURFACE ( 'NONE', #8122, 0.07499999999999977518 ) ;
#20472 = CARTESIAN_POINT ( 'NONE',  ( 0.4351562478787889821, -1.231973398409348830, 0.5773826741853494982 ) ) ;
#20473 = CARTESIAN_POINT ( 'NONE',  ( -0.03654368633476851730, -0.08356155710620498389, -0.5047517311408978857 ) ) ;
#20474 = CARTESIAN_POINT ( 'NONE',  ( -0.03174036153404024424, -0.2437184149031433322, -0.4645026301777863686 ) ) ;
#20475 = B_SPLINE_CURVE_WITH_KNOTS ( 'NONE', 3,
 ( #14425, #5168, #26806, #29887, #30267, #14243, #17719, #26393, #26608, #26994, #39523, #33167, #38923, #8267, #4972, #20839 ),
 .UNSPECIFIED., .F., .F.,
 ( 4, 2, 2, 2, 2, 2, 2, 4 ),
 ( 6.254634441385511532E-18, 0.0005051770138873787602, 0.001010354027774751232, 0.001515531041662123487, 0.002020708055549495959, 0.003031062083324246106, 0.003536239097211621180, 0.004041416111098996254 ),
 .UNSPECIFIED. ) ;
#20476 = ORIENTED_EDGE ( 'NONE', *, *, #37872, .T. ) ;
#20477 = CARTESIAN_POINT ( 'NONE',  ( 0.4309721705498754107, -1.026644649581611279, 0.7159381971572771342 ) ) ;
#20478 = CARTESIAN_POINT ( 'NONE',  ( -0.1399999999999997358, 8.414405049830459540E-17, 0.2526340763130724976 ) ) ;
#20479 = DIRECTION ( 'NONE',  ( -1.000000000000000000, -0.000000000000000000, -0.000000000000000000 ) ) ;
#20480 = EDGE_CURVE ( 'NONE', #8954, #16786, #22827, .T. ) ;
#20481 = CARTESIAN_POINT ( 'NONE',  ( 0.04328149986045663061, -0.8653222245068001861, 0.4300052425544355073 ) ) ;
#20482 = ORIENTED_EDGE ( 'NONE', *, *, #38809, .F. ) ;
#20483 = EDGE_CURVE ( 'NONE', #4385, #7962, #5503, .T. ) ;
#20484 = CARTESIAN_POINT ( 'NONE',  ( -0.03158843595483518119, 0.3316344853930314196, 0.3635668653053512056 ) ) ;
#20485 = FACE_OUTER_BOUND ( 'NONE', #27474, .T. ) ;
#20486 = CARTESIAN_POINT ( 'NONE',  ( 0.02872242845530443775, -0.5252126300208032061, -0.08844866507293194791 ) ) ;
#20487 = LINE ( 'NONE', #39597, #39038 ) ;
#20488 = EDGE_CURVE ( 'NONE', #10985, #32215, #3882, .T. ) ;
#20489 = CARTESIAN_POINT ( 'NONE',  ( 0.4623201946560837050, -1.229771743025807051, 0.6528049022507957933 ) ) ;
#20490 = CIRCLE ( 'NONE', #38857, 0.01000000000000002970 ) ;
#20492 = DIRECTION ( 'NONE',  ( 1.000000000000000000, 2.280301054154495132E-31, -1.664003471950577689E-31 ) ) ;
#20491 = DIRECTION ( 'NONE',  ( 0.000000000000000000, 0.000000000000000000, -1.000000000000000000 ) ) ;
#20493 = EDGE_CURVE ( 'NONE', #25362, #755, #29164, .T. ) ;
#20494 = CARTESIAN_POINT ( 'NONE',  ( 0.1875000000000000833, -0.9151275355372969766, 0.1556228124470683261 ) ) ;
#20495 = ORIENTED_EDGE ( 'NONE', *, *, #23573, .T. ) ;
#20496 = EDGE_CURVE ( 'NONE', #8015, #7026, #16047, .T. ) ;
#20497 = DIRECTION ( 'NONE',  ( 0.000000000000000000, 0.000000000000000000, 1.000000000000000000 ) ) ;
#20498 = EDGE_LOOP ( 'NONE', ( #11039, #131, #28850, #40363 ) ) ;
#20499 = CIRCLE ( 'NONE', #6676, 0.05000000000000000971 ) ;
#20500 = CARTESIAN_POINT ( 'NONE',  ( -0.1443922129835730761, -0.5166151207188712791, 0.3749999999999999445 ) ) ;
#20501 = AXIS2_PLACEMENT_3D ( 'NONE', #1171, #16973, #4594 ) ;
#20502 = CARTESIAN_POINT ( 'NONE',  ( 0.4157541982092135546, -1.583937682242001044, 0.6612602235990290289 ) ) ;
#20504 = FACE_OUTER_BOUND ( 'NONE', #38607, .T. ) ;
#20503 = CARTESIAN_POINT ( 'NONE',  ( 0.06924492911542678986, -0.5400501729053300837, 0.1493934372158857438 ) ) ;
#20505 = DIRECTION ( 'NONE',  ( 0.000000000000000000, 0.000000000000000000, -1.000000000000000000 ) ) ;
#20506 = ORIENTED_EDGE ( 'NONE', *, *, #31392, .F. ) ;
#20507 = AXIS2_PLACEMENT_3D ( 'NONE', #36524, #5430, #1792 ) ;
#20508 = FACE_OUTER_BOUND ( 'NONE', #8134, .T. ) ;
#20509 = CARTESIAN_POINT ( 'NONE',  ( 0.5059976415411798767, -1.396705590786084361, 0.7971529581759053684 ) ) ;
#20510 = ORIENTED_EDGE ( 'NONE', *, *, #31331, .T. ) ;
#20511 = CARTESIAN_POINT ( 'NONE',  ( 0.3259879919981947261, -1.767950897709274605, 0.5312986935551964329 ) ) ;
#20512 = CARTESIAN_POINT ( 'NONE',  ( 0.04285427992853797080, -0.4878399728613565522, 0.08281491827192886956 ) ) ;
#20513 = ADVANCED_FACE ( 'NONE', ( #25705 ), #13139, .F. ) ;
#20514 = CARTESIAN_POINT ( 'NONE',  ( 0.3715710887045398647, -1.757287345216594909, -0.4310581837286736606 ) ) ;
#20515 = PRODUCT_DEFINITION ( 'UNKNOWN', '', #22018, #12057 ) ;
#20516 = CARTESIAN_POINT ( 'NONE',  ( 0.2201243784102229206, -1.228421504212272142, 0.5037550799415064784 ) ) ;
#20517 = CARTESIAN_POINT ( 'NONE',  ( -0.1710642718812885599, 0.4986889572247748537, 0.1481991563822706026 ) ) ;
#20518 = CARTESIAN_POINT ( 'NONE',  ( 0.03654368633476876016, -0.08356155710620387367, 0.5047517311408953322 ) ) ;
#20519 = CARTESIAN_POINT ( 'NONE',  ( 0.4361655066743588827, -1.002659119010890665, 0.8380844301937150354 ) ) ;
#20520 = CARTESIAN_POINT ( 'NONE',  ( 0.4584973792621093169, -1.056415778228135149, -0.5155029497116575543 ) ) ;
#20521 = CARTESIAN_POINT ( 'NONE',  ( 0.03662792686184355301, -0.3149733899719675545, -0.3635662525351508467 ) ) ;
#20522 = AXIS2_PLACEMENT_3D ( 'NONE', #25274, #38411, #34924 ) ;
#20523 = CARTESIAN_POINT ( 'NONE',  ( 0.6300615908075114513, -1.604447140824846185, -0.5783957320051906770 ) ) ;
#20524 = CARTESIAN_POINT ( 'NONE',  ( 0.03170874437002998286, 0.3312776501328030809, 0.3635338427919215798 ) ) ;
#20525 = CARTESIAN_POINT ( 'NONE',  ( 0.6475726312330142287, -1.570798523461287122, 0.6204058447896725337 ) ) ;
#20526 = DIRECTION ( 'NONE',  ( 1.000000000000000000, 0.000000000000000000, 0.000000000000000000 ) ) ;
#20527 = CARTESIAN_POINT ( 'NONE',  ( 0.09884054835556708996, -1.311923263315395882, 0.4413102268934767647 ) ) ;
#20528 = CIRCLE ( 'NONE', #25795, 0.01500000000000006016 ) ;
#20529 = AXIS2_PLACEMENT_3D ( 'NONE', #11015, #23571, #39378 ) ;
#20530 = CARTESIAN_POINT ( 'NONE',  ( 0.2556072607908594918, -1.486118078215695082, 1.019147448260280475 ) ) ;
#20531 = CARTESIAN_POINT ( 'NONE',  ( 0.5851536363839501265, -1.491939059043950522, -0.5963745793978136867 ) ) ;
#20532 = AXIS2_PLACEMENT_3D ( 'NONE', #2985, #24982, #3179 ) ;
#20533 = CARTESIAN_POINT ( 'NONE',  ( 0.1301343169317701887, -1.291588712062315070, 0.5482363898924115242 ) ) ;
#20534 = CARTESIAN_POINT ( 'NONE',  ( 0.3047917819195049005, -1.756872408949714082, 0.5682440848926118004 ) ) ;
#20535 = CARTESIAN_POINT ( 'NONE',  ( -0.05252049209742361280, -0.2830365943384500205, 0.3740706778132465993 ) ) ;
#20536 = ORIENTED_EDGE ( 'NONE', *, *, #36363, .T. ) ;
#20538 = EDGE_LOOP ( 'NONE', ( #7350, #21711, #35175, #22484 ) ) ;
#20537 = B_SPLINE_SURFACE_WITH_KNOTS ( 'NONE', 3, 3, ( 
 ( #37720, #34826, #28458, #6634 ),
 ( #27656, #9544, #28074, #6248 ),
 ( #334, #22122, #2973, #25399 ),
 ( #37931, #15311, #34639, #6436 ),
 ( #15708, #37312, #9122, #31157 ),
 ( #2763, #28255, #12839, #3167 ),
 ( #18818, #30741, #118, #21508 ) ),
 .UNSPECIFIED., .F., .F., .F.,
 ( 4, 3, 4 ),
 ( 4, 4 ),
 ( -0.3148221902048737308, 1.762024255024811303, 3.838870700254496171 ),
 ( -2.028463316011129169, -1.118706456288100393 ),
 .UNSPECIFIED. ) ;
#20539 = EDGE_CURVE ( 'NONE', #4767, #40606, #21297, .T. ) ;
#20540 = FACE_OUTER_BOUND ( 'NONE', #20349, .T. ) ;
#20541 = CARTESIAN_POINT ( 'NONE',  ( 0.1499999999999993561, -2.632527843410151989E-17, -0.1250000000000000000 ) ) ;
#20542 = ORIENTED_EDGE ( 'NONE', *, *, #16933, .F. ) ;
#20543 = CARTESIAN_POINT ( 'NONE',  ( 0.05999999999999990757, -0.1960639381401260983, -0.03948331496955496261 ) ) ;
#20544 = DIRECTION ( 'NONE',  ( -1.000000000000000000, -2.280301054154495132E-31, 1.664003471950577689E-31 ) ) ;
#20545 = EDGE_CURVE ( 'NONE', #30939, #22862, #19334, .T. ) ;
#20546 = CARTESIAN_POINT ( 'NONE',  ( 0.4650199496164343360, -1.240973784595583052, 0.7347874889090585393 ) ) ;
#20548 = EDGE_LOOP ( 'NONE', ( #13653, #7199, #1287, #18372 ) ) ;
#20547 = CARTESIAN_POINT ( 'NONE',  ( 0.05634304521267755744, 1.092739197465705287E-15, 0.4588823192046724841 ) ) ;
#20549 = CARTESIAN_POINT ( 'NONE',  ( 0.5132401252193277141, -1.118795806750195077, 0.5530176081283582068 ) ) ;
#20550 = EDGE_CURVE ( 'NONE', #7698, #30237, #6761, .T. ) ;
#20551 = DIRECTION ( 'NONE',  ( -2.465190328815661892E-32, -1.000000000000000000, -6.656013887802287108E-31 ) ) ;
#20552 = ORIENTED_EDGE ( 'NONE', *, *, #26768, .T. ) ;
#20553 = CARTESIAN_POINT ( 'NONE',  ( 0.4203826191881492313, -1.700944664958275343, -0.4172566670736511107 ) ) ;
#20554 = ORIENTED_EDGE ( 'NONE', *, *, #40365, .T. ) ;
#20555 = CARTESIAN_POINT ( 'NONE',  ( 0.3269969022841393569, -1.639178607059557757, 0.5737397447481697998 ) ) ;
#20557 = CARTESIAN_POINT ( 'NONE',  ( 0.1766991223480313400, -0.5033111013864854932, 0.007072260541898520332 ) ) ;
#20556 = CARTESIAN_POINT ( 'NONE',  ( 0.6699226625680384517, -1.527762541135565311, 0.4380289821314772292 ) ) ;
#20558 = CARTESIAN_POINT ( 'NONE',  ( 0.4970758107849645446, -1.079867600816170059, 0.3667417262808778666 ) ) ;
#20559 = VECTOR ( 'NONE', #4550, 39.37007874015748143 ) ;
#20560 = FACE_BOUND ( 'NONE', #2061, .T. ) ;
#20561 = ORIENTED_EDGE ( 'NONE', *, *, #4666, .F. ) ;
#20562 = CYLINDRICAL_SURFACE ( 'NONE', #3556, 0.1000000000000000194 ) ;
#20563 = B_SPLINE_CURVE_WITH_KNOTS ( 'NONE', 3,
 ( #17119, #5355, #8873, #2701, #15050, #6185 ),
 .UNSPECIFIED., .F., .F.,
 ( 4, 2, 4 ),
 ( -1.278175275817475656E-05, 0.001487059793246534858, 0.002986901339251244424 ),
 .UNSPECIFIED. ) ;
#20564 = CARTESIAN_POINT ( 'NONE',  ( 0.1615127891059936760, -1.277671110434810631, -0.7015317095148801974 ) ) ;
#20565 = CARTESIAN_POINT ( 'NONE',  ( -0.2746410161513776482, -4.121841830394775030, -0.5449218438908057793 ) ) ;
#20566 = AXIS2_PLACEMENT_3D ( 'NONE', #29233, #17080, #22883 ) ;
#20567 = EDGE_CURVE ( 'NONE', #9543, #19186, #25892, .T. ) ;
#20568 = CARTESIAN_POINT ( 'NONE',  ( 0.3294235031038280637, -1.286857108956994233, 0.6092337535398641979 ) ) ;
#20569 = DIRECTION ( 'NONE',  ( 1.000000000000000000, 0.000000000000000000, 0.000000000000000000 ) ) ;
#20570 = EDGE_CURVE ( 'NONE', #1749, #17210, #3548, .T. ) ;
#20571 = CARTESIAN_POINT ( 'NONE',  ( 0.01548846960707524721, -0.3772621329472692908, -0.3651003739303438911 ) ) ;
#20572 = EDGE_CURVE ( 'NONE', #39409, #15916, #16254, .T. ) ;
#20573 = CARTESIAN_POINT ( 'NONE',  ( 0.3533729702181945265, -1.079803932887578588, 0.6392005906009133875 ) ) ;
#20574 = DIRECTION ( 'NONE',  ( 0.000000000000000000, 0.000000000000000000, -1.000000000000000000 ) ) ;
#20575 = EDGE_CURVE ( 'NONE', #7215, #17240, #26555, .T. ) ;
#20576 = CIRCLE ( 'NONE', #21902, 0.4615209409081865166 ) ;
#20577 = FACE_OUTER_BOUND ( 'NONE', #32423, .T. ) ;
#20578 = DIRECTION ( 'NONE',  ( -1.000000000000000000, -2.280301054154495132E-31, 1.664003471950577689E-31 ) ) ;
#20579 = CALENDAR_DATE ( 2026, 13, 10 ) ;
#20580 = CARTESIAN_POINT ( 'NONE',  ( 0.3511079287476752686, -1.164805985122750132, 0.4335040596137048619 ) ) ;
#20581 = CARTESIAN_POINT ( 'NONE',  ( 0.02235124290213141851, -0.5044963136724011088, 0.09030809412321962049 ) ) ;
#20582 = DIRECTION ( 'NONE',  ( 0.000000000000000000, 0.000000000000000000, 1.000000000000000000 ) ) ;
#20583 = CARTESIAN_POINT ( 'NONE',  ( 0.0004301618663383071674, -0.4396629486604707315, 0.1172979280922971101 ) ) ;
#20584 = CARTESIAN_POINT ( 'NONE',  ( 0.3827280947354409490, -1.758315590366831049, -0.5716786788641499140 ) ) ;
#20585 = CIRCLE ( 'NONE', #12660, 0.2000000000000000666 ) ;
#20586 = CARTESIAN_POINT ( 'NONE',  ( 0.1499999999999994671, 0.5198120922912046193, 0.07362328916749273644 ) ) ;
#20587 = CARTESIAN_POINT ( 'NONE',  ( 0.02235124290213196321, 0.07000983313419809062, -0.5077112423787067952 ) ) ;
#20588 = EDGE_LOOP ( 'NONE', ( #38844, #13303, #18396, #8385 ) ) ;
#20589 = CIRCLE ( 'NONE', #9419, 0.01000000000000002970 ) ;
#20590 = ORIENTED_EDGE ( 'NONE', *, *, #37343, .T. ) ;
#20591 = AXIS2_PLACEMENT_3D ( 'NONE', #33819, #24359, #27645 ) ;
#20592 = CARTESIAN_POINT ( 'NONE',  ( 0.1727619635060002046, -0.5231396776924384096, 0.1880568578134374502 ) ) ;
#20593 = VERTEX_POINT ( 'NONE', #29799 ) ;
#20594 = CARTESIAN_POINT ( 'NONE',  ( -0.1509132741912886377, 0.4664843738648666305, 0.09813923389061204872 ) ) ;
#20595 = EDGE_CURVE ( 'NONE', #14366, #14410, #758, .T. ) ;
#20597 = EDGE_LOOP ( 'NONE', ( #17692, #7459, #21156, #39049 ) ) ;
#20596 = CARTESIAN_POINT ( 'NONE',  ( 0.1344311301205933229, -0.5616928836434232908, 0.2071304835220897644 ) ) ;
#20599 = ORIENTED_EDGE ( 'NONE', *, *, #5903, .F. ) ;
#20598 = CARTESIAN_POINT ( 'NONE',  ( -0.0005234781679937302191, -0.7395155989349303516, -0.005349842773564665935 ) ) ;
#20600 = EDGE_CURVE ( 'NONE', #12135, #5011, #30483, .T. ) ;
#20601 = AXIS2_PLACEMENT_3D ( 'NONE', #9931, #22502, #19420 ) ;
#20602 = EDGE_LOOP ( 'NONE', ( #11842, #26833, #1993, #36887 ) ) ;
#20603 = CARTESIAN_POINT ( 'NONE',  ( 0.3461980321613498668, -1.167639817428515858, 0.4367330521527788556 ) ) ;
#20604 = EDGE_LOOP ( 'NONE', ( #20199, #11269, #19354, #9790 ) ) ;
#20605 = CARTESIAN_POINT ( 'NONE',  ( -0.01173968894115999702, -0.5704551753217745880, 0.3127573418170750408 ) ) ;
#20607 = CARTESIAN_POINT ( 'NONE',  ( 0.1861578656809604604, -1.253385901324051144, 0.5940953843551290969 ) ) ;
#20606 = CARTESIAN_POINT ( 'NONE',  ( -0.03664605387828129973, -0.4684681574363449563, -0.1090337349855014654 ) ) ;
#20608 = CARTESIAN_POINT ( 'NONE',  ( 0.5965761245944036784, -1.493465029535157029, 0.5182417262812423209 ) ) ;
#20609 = DATE_TIME_ROLE ( 'classification_date' ) ;
#20610 = CARTESIAN_POINT ( 'NONE',  ( 5.487288226601811250E-16, -0.2899999999999993694, -0.04250000000000066225 ) ) ;
#20612 = ORIENTED_EDGE ( 'NONE', *, *, #36182, .T. ) ;
#20611 = ORIENTED_EDGE ( 'NONE', *, *, #16072, .F. ) ;
#20613 = CARTESIAN_POINT ( 'NONE',  ( 0.01131643751578586751, -0.9461934511605994969, 0.1286063635815848094 ) ) ;
#20614 = CARTESIAN_POINT ( 'NONE',  ( 0.1105467269751546355, -1.363254696163590518, 0.6837916529716010494 ) ) ;
#20615 = CARTESIAN_POINT ( 'NONE',  ( 0.09483622992911115712, -0.6024812608924786650, 0.2828265107361390696 ) ) ;
#20616 = CARTESIAN_POINT ( 'NONE',  ( 0.5524544392347628952, -1.511033082563104424, 0.5634634827593720807 ) ) ;
#20617 = DIRECTION ( 'NONE',  ( 0.000000000000000000, -5.463695987328525648E-15, -1.000000000000000000 ) ) ;
#20618 = CARTESIAN_POINT ( 'NONE',  ( 0.4778170654558047126, -1.668016138613298560, 0.5682417262808788783 ) ) ;
#20619 = CARTESIAN_POINT ( 'NONE',  ( 0.1999999999999794720, -2.097675824466503247, -0.2588528740066096678 ) ) ;
#20620 = CONICAL_SURFACE ( 'NONE', #37045, 0.1400000000000005684, 1.047197551196600518 ) ;
#20621 = CARTESIAN_POINT ( 'NONE',  ( 0.3990506063816511295, -1.683314032604188437, -0.4045594003095706048 ) ) ;
#20622 = CARTESIAN_POINT ( 'NONE',  ( 0.3981089169560373398, -1.724261708826889228, 0.4259583991113702339 ) ) ;
#20623 = EDGE_CURVE ( 'NONE', #20310, #15679, #37697, .T. ) ;
#20624 = CARTESIAN_POINT ( 'NONE',  ( 0.3478153622845648885, -1.628211818192446536, -0.6007519914469682254 ) ) ;
#20625 = CIRCLE ( 'NONE', #23275, 0.01500000000000005496 ) ;
#20626 = DIRECTION ( 'NONE',  ( 0.000000000000000000, 0.000000000000000000, -1.000000000000000000 ) ) ;
#20627 = CARTESIAN_POINT ( 'NONE',  ( 0.1999999999999789724, -2.097675824466503247, -0.2588528740066097233 ) ) ;
#20628 = VECTOR ( 'NONE', #4292, 39.37007874015748854 ) ;
#20629 = CARTESIAN_POINT ( 'NONE',  ( -0.0004024309093390212992, -0.9356036818533377541, 0.1173018208859672590 ) ) ;
#20630 = CARTESIAN_POINT ( 'NONE',  ( 0.4353877174700542807, -1.231365710109779910, 0.5832408271660066701 ) ) ;
#20631 = DIRECTION ( 'NONE',  ( 1.000000000000000000, 0.000000000000000000, 0.000000000000000000 ) ) ;
#20632 = CARTESIAN_POINT ( 'NONE',  ( 0.06257380981966247091, -1.147456929947968884, 0.7547943717889301629 ) ) ;
#20633 = CIRCLE ( 'NONE', #2883, 0.1000000000000000194 ) ;
#20634 = CARTESIAN_POINT ( 'NONE',  ( 0.3711835952353229051, -0.9982156264046870842, 0.6339317236198600547 ) ) ;
#20635 = APPROVAL_DATE_TIME ( #17332, #2114 ) ;
#20636 = CARTESIAN_POINT ( 'NONE',  ( 0.2506904587504640847, -0.6594178163634784040, 0.5852584525479398447 ) ) ;
#20637 = CONICAL_SURFACE ( 'NONE', #33098, 0.5156329413417598539, 1.047197551196601184 ) ;
#20638 = DIRECTION ( 'NONE',  ( 0.4999551463232372317, -0.8660512985181135770, 0.000000000000000000 ) ) ;
#20639 = CARTESIAN_POINT ( 'NONE',  ( 0.04308558661661680139, -0.05688326490871156715, -0.4910261092774084180 ) ) ;
#20640 = ORIENTED_EDGE ( 'NONE', *, *, #37112, .F. ) ;
#20641 = CARTESIAN_POINT ( 'NONE',  ( 0.09999999999998190892, -1.871552131921257578, -0.6463968910507320587 ) ) ;
#20642 = CARTESIAN_POINT ( 'NONE',  ( 0.08275655485679608847, -0.9821269456125771846, 0.8324652710739945949 ) ) ;
#20643 = CIRCLE ( 'NONE', #2905, 0.01499999999999995781 ) ;
#20644 = CARTESIAN_POINT ( 'NONE',  ( 0.2169591561341989161, -1.302156274398155622, -0.6184399470714007085 ) ) ;
#20646 = ORIENTED_EDGE ( 'NONE', *, *, #14754, .T. ) ;
#20645 = CARTESIAN_POINT ( 'NONE',  ( 0.3008812400416732702, -1.193811035676025645, 0.5682417262808779901 ) ) ;
#20647 = CARTESIAN_POINT ( 'NONE',  ( 0.5029538533377585496, -1.673443447161921727, -0.4264433612092255466 ) ) ;
#20648 = CARTESIAN_POINT ( 'NONE',  ( 0.6053747664524671279, -1.274130884506152084, 0.6672623879134867986 ) ) ;
#20650 = VERTEX_POINT ( 'NONE', #20547 ) ;
#20649 = ORIENTED_EDGE ( 'NONE', *, *, #24266, .F. ) ;
#20651 = CARTESIAN_POINT ( 'NONE',  ( 0.1379511725373750997, -1.300921670157717758, -0.6912193855582036139 ) ) ;
#20652 = VECTOR ( 'NONE', #28314, 39.37007874015748143 ) ;
#20653 = VERTEX_POINT ( 'NONE', #1245 ) ;
#20654 = AXIS2_PLACEMENT_3D ( 'NONE', #29137, #25249, #9803 ) ;
#20655 = FACE_OUTER_BOUND ( 'NONE', #30945, .T. ) ;
#20656 = AXIS2_PLACEMENT_3D ( 'NONE', #8461, #21230, #27602 ) ;
#20657 = PRODUCT_DEFINITION_SHAPE ( 'NONE', 'NONE',  #40661 ) ;
#20658 = DIRECTION ( 'NONE',  ( -0.4999999999999946709, 0.3297230132044422501, 0.8008013077932555346 ) ) ;
#20659 = CALENDAR_DATE ( 2026, 13, 10 ) ;
#20660 = FACE_OUTER_BOUND ( 'NONE', #12924, .T. ) ;
#20661 = ORIENTED_EDGE ( 'NONE', *, *, #35593, .T. ) ;
#20662 = CARTESIAN_POINT ( 'NONE',  ( 0.1999999922267132468, -2.089163595796008188, -0.2938764050442146392 ) ) ;
#20663 = CARTESIAN_POINT ( 'NONE',  ( 0.2067711592739439608, -0.8738170338164513717, 0.6440652579052440485 ) ) ;
#20664 = AXIS2_PLACEMENT_3D ( 'NONE', #27493, #33644, #32693 ) ;
#20665 = CARTESIAN_POINT ( 'NONE',  ( 0.2950888954987143098, -1.594460040844208226, 0.9601565580101251163 ) ) ;
#20666 = CARTESIAN_POINT ( 'NONE',  ( 0.1013562098727056604, -0.5836111280376300448, 0.2907278789027847310 ) ) ;
#20667 = AXIS2_PLACEMENT_3D ( 'NONE', #815, #6532, #26 ) ;
#20669 = CARTESIAN_POINT ( 'NONE',  ( -0.1873388932668320905, 0.5325605939836577374, 0.3749999999999996669 ) ) ;
#20668 = CARTESIAN_POINT ( 'NONE',  ( 0.2698039524218523999, -1.685703698922064842, 0.6459807199062099770 ) ) ;
#20670 = CARTESIAN_POINT ( 'NONE',  ( 0.05563666494323122463, -0.9593727281709375498, 0.3928659522660303272 ) ) ;
#20671 = ORIENTED_EDGE ( 'NONE', *, *, #6784, .T. ) ;
#20672 = VERTEX_POINT ( 'NONE', #33474 ) ;
#20673 = DIRECTION ( 'NONE',  ( -1.000000000000000000, -0.000000000000000000, -0.000000000000000000 ) ) ;
#20674 = CARTESIAN_POINT ( 'NONE',  ( 0.1948345289757165422, -0.5719942820726408028, 0.2877997954568007333 ) ) ;
#20675 = CARTESIAN_POINT ( 'NONE',  ( 0.4484726360943441792, -1.685722521223443904, -0.5155029497116575543 ) ) ;
#20676 = CARTESIAN_POINT ( 'NONE',  ( -0.05544444631433743942, -0.4445724550912839579, -0.1231054764780145916 ) ) ;
#20677 = VECTOR ( 'NONE', #5193, 39.37007874015748143 ) ;
#20678 = CARTESIAN_POINT ( 'NONE',  ( 0.07196704047461272014, -1.314327500870678733, 0.4956894008401456220 ) ) ;
#20679 = AXIS2_PLACEMENT_3D ( 'NONE', #37812, #10031, #22202 ) ;
#20680 = CARTESIAN_POINT ( 'NONE',  ( 0.4299129845042397591, -1.697471419175033747, -0.5152995808109321896 ) ) ;
#20681 = DIRECTION ( 'NONE',  ( -6.162975822039154730E-33, 0.000000000000000000, -1.000000000000000000 ) ) ;
#20682 = CARTESIAN_POINT ( 'NONE',  ( 0.3136710858027207949, -0.8676775186001693951, 0.6334163436129683911 ) ) ;
#20683 = VECTOR ( 'NONE', #7802, 39.37007874015748143 ) ;
#20684 = VECTOR ( 'NONE', #19027, 39.37007874015748143 ) ;
#20685 = CARTESIAN_POINT ( 'NONE',  ( 0.01548846960707511190, 0.5198120922912057296, 0.07362328916748590857 ) ) ;
#20686 = APPLIED_APPROVAL_ASSIGNMENT ( #31795, ( #10846 ) ) ;
#20687 = CARTESIAN_POINT ( 'NONE',  ( 0.09620807403327706619, -1.426205906121508882, -0.3356627542665827635 ) ) ;
#20688 = DIRECTION ( 'NONE',  ( -1.000000000000000000, -2.280301054154495132E-31, 1.664003471950577689E-31 ) ) ;
#20689 = ORIENTED_EDGE ( 'NONE', *, *, #36086, .T. ) ;
#20690 = CARTESIAN_POINT ( 'NONE',  ( 0.4113447267721775380, -1.199437961476878867, 0.6795061555269068521 ) ) ;
#20691 = CARTESIAN_POINT ( 'NONE',  ( 0.4534978277988769846, -1.047755265242954037, -0.5155029497116575543 ) ) ;
#20692 = VECTOR ( 'NONE', #17527, 39.37007874015748854 ) ;
#20693 = CARTESIAN_POINT ( 'NONE',  ( -0.05187277790672436412, -0.2910352029727574785, -0.3700865090056942308 ) ) ;
#20694 = ORIENTED_EDGE ( 'NONE', *, *, #26761, .F. ) ;
#20695 = CARTESIAN_POINT ( 'NONE',  ( 0.2819449068958458371, -0.8989038099100304935, 0.5575401372502252206 ) ) ;
#20696 = B_SPLINE_CURVE_WITH_KNOTS ( 'NONE', 1,
 ( #11041, #20300, #39408, #23414 ),
 .UNSPECIFIED., .F., .F.,
 ( 2, 1, 1, 2 ),
 ( -0.0007619999999999984642, 2.276824562219559311E-18, 0.0007620000000000012831, 0.001523999999999997145 ),
 .UNSPECIFIED. ) ;
#20697 = DIRECTION ( 'NONE',  ( 1.000000000000000000, 0.000000000000000000, 0.000000000000000000 ) ) ;
#20698 = CARTESIAN_POINT ( 'NONE',  ( 0.1710813352435040513, -1.228829274190828880, 0.7416658143285672633 ) ) ;
#20699 = ORIENTED_EDGE ( 'NONE', *, *, #8922, .T. ) ;
#20700 = DIRECTION ( 'NONE',  ( -6.217248937900885304E-15, 2.158931604386568927E-14, 1.000000000000000000 ) ) ;
#20701 = CARTESIAN_POINT ( 'NONE',  ( 0.04229974373173313318, 0.008638059335311996934, 0.4686103131113881770 ) ) ;
#20702 = DIRECTION ( 'NONE',  ( -7.771561172376107616E-16, 7.170354002788761615E-17, -1.000000000000000000 ) ) ;
#20703 = DIRECTION ( 'NONE',  ( 7.771561172376107616E-16, -7.170354002788761615E-17, 1.000000000000000000 ) ) ;
#20704 = VECTOR ( 'NONE', #13150, 39.37007874015748143 ) ;
#20705 = CARTESIAN_POINT ( 'NONE',  ( 0.4384245533723877819, -1.193668192789114402, 0.6617654306343142556 ) ) ;
#20707 = CARTESIAN_POINT ( 'NONE',  ( 0.3546785580517292646, -1.844992007381027976, -0.4891695103279160572 ) ) ;
#20706 = CARTESIAN_POINT ( 'NONE',  ( -0.1574377185082707353, 0.4885537809602777948, 0.09999999999999989453 ) ) ;
#20708 = CARTESIAN_POINT ( 'NONE',  ( 0.5744812595043889969, -1.541517170152952643, -0.5460780551203860966 ) ) ;
#20709 = VERTEX_POINT ( 'NONE', #26730 ) ;
#20710 = AXIS2_PLACEMENT_3D ( 'NONE', #8702, #24571, #1954 ) ;
#20711 = CARTESIAN_POINT ( 'NONE',  ( -0.01548846960707477016, 0.4638115001430995199, -0.2459753896937812156 ) ) ;
#20712 = ORIENTED_EDGE ( 'NONE', *, *, #29774, .T. ) ;
#20713 = CIRCLE ( 'NONE', #1041, 0.1000000000000000194 ) ;
#20714 = DIRECTION ( 'NONE',  ( -1.510243460696182204E-15, 0.000000000000000000, -1.000000000000000000 ) ) ;
#20715 = CARTESIAN_POINT ( 'NONE',  ( 0.09248278889685218607, -0.7035006267299489524, 0.5252844283285661442 ) ) ;
#20717 = FACE_BOUND ( 'NONE', #1950, .T. ) ;
#20716 = CARTESIAN_POINT ( 'NONE',  ( 0.7071069014570956490, -1.521634513519168452, 0.5617257377400114438 ) ) ;
#20718 = FACE_OUTER_BOUND ( 'NONE', #1985, .T. ) ;
#20719 = LOCAL_TIME ( 0, 53, 7.000000000000000000, #31097 ) ;
#20720 = ORIENTED_EDGE ( 'NONE', *, *, #38971, .F. ) ;
#20721 = CARTESIAN_POINT ( 'NONE',  ( 0.5602799925893692246, -1.505597493397644149, 0.5182417262812344383 ) ) ;
#20722 = CARTESIAN_POINT ( 'NONE',  ( 0.5734050883652083153, -1.499117349616238881, 0.5634239076586705641 ) ) ;
#20723 = EDGE_LOOP ( 'NONE', ( #24874, #2525, #12583, #26119, #9176 ) ) ;
#20724 = CIRCLE ( 'NONE', #22701, 0.1000000000000000194 ) ;
#20725 = CARTESIAN_POINT ( 'NONE',  ( 0.3221170355888270387, -1.758120817819334158, 0.5423541406307321733 ) ) ;
#20726 = CARTESIAN_POINT ( 'NONE',  ( 0.05279905671745279555, -0.4561941007107766510, 0.1063003320160282317 ) ) ;
#20727 = ADVANCED_FACE ( 'NONE', ( #8384 ), #11658, .T. ) ;
#20728 = LINE ( 'NONE', #18421, #22499 ) ;
#20729 = CARTESIAN_POINT ( 'NONE',  ( 0.2219243583429411082, -1.238942616970301280, 0.4663869545833551622 ) ) ;
#20730 = CARTESIAN_POINT ( 'NONE',  ( 0.3967637807842907538, -1.750213052463736485, -0.4985867268025130916 ) ) ;
#20731 = CARTESIAN_POINT ( 'NONE',  ( 0.05283719472145074342, -0.03966590960886508255, 0.4666299489511763210 ) ) ;
#20732 = EDGE_CURVE ( 'NONE', #22699, #27179, #24241, .T. ) ;
#20733 = CARTESIAN_POINT ( 'NONE',  ( 0.7224934542336318710, -1.479659627397842403, 0.5766931279523788145 ) ) ;
#20734 = ADVANCED_FACE ( 'NONE', ( #14775 ), #9006, .F. ) ;
#20735 = CARTESIAN_POINT ( 'NONE',  ( 0.3674370130824703429, -1.724856795990272973, -0.6064096210563775236 ) ) ;
#20736 = CARTESIAN_POINT ( 'NONE',  ( 0.01895494625228179644, -0.2428766181966280080, -0.4598657641708848720 ) ) ;
#20737 = AXIS2_PLACEMENT_3D ( 'NONE', #20776, #10483, #20362 ) ;
#20738 = EDGE_CURVE ( 'NONE', #37734, #1197, #4185, .T. ) ;
#20739 = ADVANCED_FACE ( 'NONE', ( #17845 ), #19968, .T. ) ;
#20740 = CARTESIAN_POINT ( 'NONE',  ( 0.5771669516282522672, -1.610595408416737540, -0.5496873730034127492 ) ) ;
#20741 = CIRCLE ( 'NONE', #8883, 0.1000000000000000194 ) ;
#20742 = CARTESIAN_POINT ( 'NONE',  ( 0.1306785186278567601, -1.354088256797956191, -0.7085892327543563685 ) ) ;
#20743 = FACE_OUTER_BOUND ( 'NONE', #38946, .T. ) ;
#20744 = EDGE_CURVE ( 'NONE', #26629, #24814, #2244, .T. ) ;
#20745 = CARTESIAN_POINT ( 'NONE',  ( 0.6693573925625662113, -1.453639881720312443, 0.4440174721139349967 ) ) ;
#20746 = CARTESIAN_POINT ( 'NONE',  ( -0.04293317454820692880, 0.4432234940308288906, -0.2195257349118421575 ) ) ;
#20747 = ORIENTED_EDGE ( 'NONE', *, *, #32509, .F. ) ;
#20748 = APPROVAL_PERSON_ORGANIZATION ( #2710, #29513, #36850 ) ;
#20749 = CARTESIAN_POINT ( 'NONE',  ( 0.1180550382625277506, -1.031362315377588157, 0.9291368297579983837 ) ) ;
#20750 = CARTESIAN_POINT ( 'NONE',  ( 0.5728032096484048097, -1.543894942757779720, -0.5357990152665924599 ) ) ;
#20751 = CARTESIAN_POINT ( 'NONE',  ( 0.1825913591765910837, -1.261380122499173639, 0.5231355524944251156 ) ) ;
#20752 = FACE_OUTER_BOUND ( 'NONE', #21380, .T. ) ;
#20753 = VERTEX_POINT ( 'NONE', #15165 ) ;
#20754 = LINE ( 'NONE', #26913, #21090 ) ;
#20755 = EDGE_CURVE ( 'NONE', #24008, #7319, #21153, .T. ) ;
#20756 = CARTESIAN_POINT ( 'NONE',  ( 0.1438070510857625550, -1.283988175806205723, 0.3667417262808778111 ) ) ;
#20757 = APPROVAL ( #2559, 'UNSPECIFIED' ) ;
#20758 = DIRECTION ( 'NONE',  ( -5.879757087931980518E-34, -0.5877852522924756906, -0.8090169943749455639 ) ) ;
#20759 = CARTESIAN_POINT ( 'NONE',  ( 0.3480912466186250054, -1.075785438362978574, 0.7514184427825739698 ) ) ;
#20761 = VERTEX_POINT ( 'NONE', #2235 ) ;
#20760 = CARTESIAN_POINT ( 'NONE',  ( -0.1688425296110669938, 0.4915895952456239004, 0.1316117873487830936 ) ) ;
#20762 = CARTESIAN_POINT ( 'NONE',  ( 0.5240142186908230970, -1.141661684775556296, 0.6661746706671649587 ) ) ;
#20763 = CARTESIAN_POINT ( 'NONE',  ( 0.05562144613422641271, 0.4441896308501004365, -0.1229845283801405259 ) ) ;
#20764 = ORIENTED_EDGE ( 'NONE', *, *, #34872, .F. ) ;
#20765 = CARTESIAN_POINT ( 'NONE',  ( 0.4287117948289022595, -1.695887552032223411, -0.4140898068348377037 ) ) ;
#20766 = CARTESIAN_POINT ( 'NONE',  ( 0.1571208352139699116, -1.056369343299222052, 0.8465988816176888143 ) ) ;
#20768 = CARTESIAN_POINT ( 'NONE',  ( 0.1874708175093220963, -0.5603066453311646988, 0.03565836971681755896 ) ) ;
#20767 = CARTESIAN_POINT ( 'NONE',  ( 0.7052075302012132951, -1.496959223845125697, 0.5106402777884315736 ) ) ;
#20769 = CARTESIAN_POINT ( 'NONE',  ( 0.000000000000000000, 0.7171888913565960255, -0.2950238883388468514 ) ) ;
#20770 = DIRECTION ( 'NONE',  ( 0.000000000000000000, 0.000000000000000000, -1.000000000000000000 ) ) ;
#20771 = VERTEX_POINT ( 'NONE', #5494 ) ;
#20772 = AXIS2_PLACEMENT_3D ( 'NONE', #31825, #34899, #19077 ) ;
#20773 = CIRCLE ( 'NONE', #24069, 0.1033070866141732325 ) ;
#20774 = VERTEX_POINT ( 'NONE', #27337 ) ;
#20775 = CARTESIAN_POINT ( 'NONE',  ( 0.7053410326410682885, -1.513865973459305625, 0.5669051209305092653 ) ) ;
#20776 = CARTESIAN_POINT ( 'NONE',  ( 0.4159916692016358830, -1.069406866067976081, -0.5155029497116575543 ) ) ;
#20777 = CARTESIAN_POINT ( 'NONE',  ( 0.3127911584666093203, -1.259356820209954320, 0.6734448273910310645 ) ) ;
#20778 = LOCAL_TIME ( 0, 53, 7.000000000000000000, #25253 ) ;
#20779 = DIRECTION ( 'NONE',  ( 0.000000000000000000, -0.8438867430782092116, -0.5365213554527465956 ) ) ;
#20780 = B_SPLINE_CURVE_WITH_KNOTS ( 'NONE', 3,
 ( #4681, #36586, #4295, #16862, #35770, #29404 ),
 .UNSPECIFIED., .F., .F.,
 ( 4, 2, 4 ),
 ( 0.3856337156884760975, 0.6928168578442379655, 1.000000000000000000 ),
 .UNSPECIFIED. ) ;
#20781 = DIRECTION ( 'NONE',  ( 0.000000000000000000, 0.000000000000000000, -1.000000000000000000 ) ) ;
#20782 = CIRCLE ( 'NONE', #1737, 0.01500000000000005322 ) ;
#20783 = CARTESIAN_POINT ( 'NONE',  ( 0.3590089656256109651, -1.084402299286110205, 0.6388604778428618181 ) ) ;
#20784 = EDGE_CURVE ( 'NONE', #40011, #38034, #21568, .T. ) ;
#20785 = DIRECTION ( 'NONE',  ( -0.4999999999999991118, -0.1289820025937478687, -0.8563665354314745626 ) ) ;
#20786 = CARTESIAN_POINT ( 'NONE',  ( 0.05634307799789382842, 0.2614070397638486587, -0.3772863199289389069 ) ) ;
#20787 = CARTESIAN_POINT ( 'NONE',  ( -0.2299999999999999267, 0.5182417262804744906, 0.3599999999999993205 ) ) ;
#20788 = CARTESIAN_POINT ( 'NONE',  ( 4.835832620238532854E-16, 0.2900000000000004241, 0.06434668806854040857 ) ) ;
#20789 = SHAPE_DEFINITION_REPRESENTATION ( #20890, #7794 ) ;
#20790 = B_SPLINE_CURVE_WITH_KNOTS ( 'NONE', 3,
 ( #22967, #28526, #19481, #185, #22367, #25239, #35102, #19666, #15979, #7292, #25647, #25861, #37986, #32203 ),
 .UNSPECIFIED., .F., .F.,
 ( 4, 2, 2, 2, 2, 2, 4 ),
 ( 0.000000000000000000, 0.0003496075178145187368, 0.0006992150356290374735, 0.001398430071258081019, 0.002097645106887124564, 0.002447252624701651974, 0.002796860142516178951 ),
 .UNSPECIFIED. ) ;
#20791 = EDGE_CURVE ( 'NONE', #34047, #26723, #17987, .T. ) ;
#20792 = EDGE_CURVE ( 'NONE', #24668, #37734, #28508, .T. ) ;
#20793 = EDGE_CURVE ( 'NONE', #20761, #14767, #8794, .T. ) ;
#20794 = CARTESIAN_POINT ( 'NONE',  ( 0.4610664102433212341, -1.239956099693821923, 0.6057417262809809966 ) ) ;
#20795 = CARTESIAN_POINT ( 'NONE',  ( 0.7079468961844166408, -1.501371341494817990, 0.5260067408216857476 ) ) ;
#20796 = CARTESIAN_POINT ( 'NONE',  ( 0.01205697956425911578, -0.4614203675330614818, 0.01888062949785454178 ) ) ;
#20797 = CARTESIAN_POINT ( 'NONE',  ( 0.3964872829018378786, -1.750372669497358258, -0.5853913325796881173 ) ) ;
#20798 = CARTESIAN_POINT ( 'NONE',  ( 0.004450193950484558972, -0.5028013914547208030, 0.3755358887046206795 ) ) ;
#20799 = CIRCLE ( 'NONE', #6975, 0.06250000000000001388 ) ;
#20800 = DIRECTION ( 'NONE',  ( 1.000000000000000000, 0.000000000000000000, 0.000000000000000000 ) ) ;
#20801 = ORIENTED_EDGE ( 'NONE', *, *, #7983, .T. ) ;
#20802 = ORIENTED_EDGE ( 'NONE', *, *, #13480, .T. ) ;
#20803 = EDGE_CURVE ( 'NONE', #39055, #13520, #8831, .T. ) ;
#20804 = CARTESIAN_POINT ( 'NONE',  ( 0.1869757914927797082, -0.5054508214312307679, 0.1434178755068601097 ) ) ;
#20805 = ORIENTED_EDGE ( 'NONE', *, *, #37409, .F. ) ;
#20806 = LINE ( 'NONE', #12470, #22664 ) ;
#20807 = DIRECTION ( 'NONE',  ( 1.000000000000000000, 0.000000000000000000, 0.000000000000000000 ) ) ;
#20808 = ADVANCED_FACE ( 'NONE', ( #27724 ), #38363, .T. ) ;
#20809 = CARTESIAN_POINT ( 'NONE',  ( -0.2399999999999999079, -4.350369088120884520, -0.8413950570247814564 ) ) ;
#20811 = ORIENTED_EDGE ( 'NONE', *, *, #628, .F. ) ;
#20810 = CARTESIAN_POINT ( 'NONE',  ( 0.0004931007904724790366, -0.6328789585674243767, -0.01332374601334393796 ) ) ;
#20812 = ORIENTED_EDGE ( 'NONE', *, *, #22464, .T. ) ;
#20813 = CARTESIAN_POINT ( 'NONE',  ( 0.1153471662232078698, -0.4465907064269051263, 0.1457432652200511269 ) ) ;
#20814 = ORIENTED_EDGE ( 'NONE', *, *, #26110, .F. ) ;
#20815 = CARTESIAN_POINT ( 'NONE',  ( -0.01401648950443899755, -0.5294816969626192638, 0.1867042317857136313 ) ) ;
#20817 = CARTESIAN_POINT ( 'NONE',  ( 0.1397034525758832912, -1.246271773685439843, 0.6054699798243167175 ) ) ;
#20816 = CARTESIAN_POINT ( 'NONE',  ( -0.04229956186878638252, -0.4483852441756287499, -0.1364680347311819086 ) ) ;
#20818 = CARTESIAN_POINT ( 'NONE',  ( 0.3999999999999787059, -2.097675824466503691, -0.2588528740066097233 ) ) ;
#20819 = CALENDAR_DATE ( 2026, 13, 10 ) ;
#20820 = CARTESIAN_POINT ( 'NONE',  ( -0.07999999999999998779, -1.984114763688379579, -0.7731012124309359912 ) ) ;
#20822 = ORIENTED_EDGE ( 'NONE', *, *, #4412, .T. ) ;
#20821 = EDGE_LOOP ( 'NONE', ( #2284, #21575, #22653, #15815 ) ) ;
#20823 = CARTESIAN_POINT ( 'NONE',  ( 0.01149267591286579245, -0.8822181097163754870, -0.02549007114653972436 ) ) ;
#20824 = CARTESIAN_POINT ( 'NONE',  ( 0.02668311692182204556, -0.9302189178724024066, 0.5981466358412875772 ) ) ;
#20825 = CARTESIAN_POINT ( 'NONE',  ( 0.1577241720307761830, -0.7737101317851643456, 0.5597104839991265957 ) ) ;
#20826 = CARTESIAN_POINT ( 'NONE',  ( 0.1855202466758043289, -0.8222115594753283130, 0.1007574222658992741 ) ) ;
#20827 = DIRECTION ( 'NONE',  ( 1.000000000000000000, 0.000000000000000000, 0.000000000000000000 ) ) ;
#20828 = CARTESIAN_POINT ( 'NONE',  ( 0.06022125200248988619, -1.332505749032950604, 0.5527776638144757948 ) ) ;
#20829 = CARTESIAN_POINT ( 'NONE',  ( 0.4111244031346745209, -1.715100544966072116, -0.4234454618225184652 ) ) ;
#20830 = CARTESIAN_POINT ( 'NONE',  ( 0.6784119790018648954, -1.437364601474310222, -0.5155029497116575543 ) ) ;
#20831 = VECTOR ( 'NONE', #16524, 39.37007874015748854 ) ;
#20832 = DIRECTION ( 'NONE',  ( 0.000000000000000000, -0.8063205929144885431, 0.5914787413272156735 ) ) ;
#20833 = FACE_BOUND ( 'NONE', #21189, .T. ) ;
#20834 = DIRECTION ( 'NONE',  ( 0.000000000000000000, 0.000000000000000000, -1.000000000000000000 ) ) ;
#20835 = CARTESIAN_POINT ( 'NONE',  ( 0.3985140155258163341, -1.105590023491421769, 0.6028892103598463281 ) ) ;
#20836 = DIRECTION ( 'NONE',  ( 0.4999551463232373427, -0.8660512985181134660, 0.000000000000000000 ) ) ;
#20837 = LOCAL_TIME ( 0, 53, 7.000000000000000000, #5146 ) ;
#20838 = ADVANCED_FACE ( 'NONE', ( #25038 ), #10807, .T. ) ;
#20839 = CARTESIAN_POINT ( 'NONE',  ( 0.6335899703865320864, -1.596177751663357736, -0.4443638777805991591 ) ) ;
#20840 = VECTOR ( 'NONE', #10627, 39.37007874015748143 ) ;
#20841 = CARTESIAN_POINT ( 'NONE',  ( 0.2565019309081923438, -1.535068652515254151, 0.9594965307338887417 ) ) ;
#20842 = CARTESIAN_POINT ( 'NONE',  ( 0.4929465528686918230, -1.082715557938388029, 0.5668025781570900090 ) ) ;
#20843 = CARTESIAN_POINT ( 'NONE',  ( -0.002208084152283221538, -0.8485876746239671142, 0.2367784268410296489 ) ) ;
#20844 = DATE_AND_TIME ( #4759, #40437 ) ;
#20845 = CARTESIAN_POINT ( 'NONE',  ( 0.1876258513389257310, -0.4649338269308297966, 0.1998821562507554217 ) ) ;
#20846 = EDGE_CURVE ( 'NONE', #33794, #39166, #31160, .T. ) ;
#20847 = CARTESIAN_POINT ( 'NONE',  ( 0.5264113014007820723, -1.640729993778254014, 0.5682417262808777680 ) ) ;
#20848 = CARTESIAN_POINT ( 'NONE',  ( 0.05634402396114692596, 0.01030784378588770096, -0.4588801752140551082 ) ) ;
#20849 = ORIENTED_EDGE ( 'NONE', *, *, #14451, .T. ) ;
#20850 = CARTESIAN_POINT ( 'NONE',  ( 0.3526790567758040229, -1.721859164019411637, -0.5374078869160439087 ) ) ;
#20851 = CARTESIAN_POINT ( 'NONE',  ( 0.02401934354094946433, -0.7133339170399575213, 0.5802934023308400358 ) ) ;
#20852 = EDGE_CURVE ( 'NONE', #26173, #7024, #28137, .T. ) ;
#20853 = B_SPLINE_CURVE_WITH_KNOTS ( 'NONE', 3,
 ( #35363, #3271, #31464, #29187, #22843, #31665, #15825, #838, #22634, #13345, #19539, #22027, #3877, #28376, #12742, #9848, #13559, #34548 ),
 .UNSPECIFIED., .F., .F.,
 ( 4, 2, 2, 2, 2, 2, 2, 2, 4 ),
 ( -0.003133633995111201158, -0.002350221109836720442, -0.001566808224562239726, -0.0007833953392877642148, 1.754598671129675713E-08, 0.0007834304312611872420, 0.001566843316535663187, 0.002350256201810138265, 0.003133669087084614210 ),
 .UNSPECIFIED. ) ;
#20854 = CARTESIAN_POINT ( 'NONE',  ( 0.5873107854097197045, -1.491061893667417371, 0.5610701424334307852 ) ) ;
#20855 = CARTESIAN_POINT ( 'NONE',  ( 0.3695052819757338458, -1.758428263776098843, -0.4278193900811941286 ) ) ;
#20857 = ORIENTED_EDGE ( 'NONE', *, *, #40301, .T. ) ;
#20856 = CARTESIAN_POINT ( 'NONE',  ( 0.3941594819206604150, -1.750901474553208548, -0.4851235437278881846 ) ) ;
#20858 = CIRCLE ( 'NONE', #21506, 0.01500000000000000638 ) ;
#20859 = EDGE_CURVE ( 'NONE', #39668, #9404, #999, .T. ) ;
#20860 = CARTESIAN_POINT ( 'NONE',  ( -0.01548846960707538425, 0.09061086148575919763, -0.5171215251571033011 ) ) ;
#20861 = CARTESIAN_POINT ( 'NONE',  ( 0.1989132775362471572, -0.6135140644431382739, 0.3133236772439795259 ) ) ;
#20863 = ORIENTED_EDGE ( 'NONE', *, *, #37288, .F. ) ;
#20862 = ORIENTED_EDGE ( 'NONE', *, *, #13141, .T. ) ;
#20864 = CARTESIAN_POINT ( 'NONE',  ( 0.1323247281835593092, -1.307327334972417265, -0.7167432404901448173 ) ) ;
#20865 = VERTEX_POINT ( 'NONE', #25872 ) ;
#20866 = LINE ( 'NONE', #1937, #32896 ) ;
#20867 = CARTESIAN_POINT ( 'NONE',  ( 0.1826134026666640653, -1.261648033191452134, 0.4282186462236581836 ) ) ;
#20868 = APPROVAL_STATUS ( 'not_yet_approved' ) ;
#20869 = CARTESIAN_POINT ( 'NONE',  ( 0.01548846960707306146, 0.3772621329473473950, -0.3651003739302714490 ) ) ;
#20870 = ORIENTED_EDGE ( 'NONE', *, *, #3207, .F. ) ;
#20871 = CARTESIAN_POINT ( 'NONE',  ( 0.2066366444374464761, -1.235973243786347542, 0.5699631943058273142 ) ) ;
#20872 = CARTESIAN_POINT ( 'NONE',  ( 0.09426521933953035948, -0.7368835468627613627, 0.2937654492271515871 ) ) ;
#20873 = CARTESIAN_POINT ( 'NONE',  ( 0.2183274780194145726, -1.352241882189698652, 1.036399751412596437 ) ) ;
#20874 = CARTESIAN_POINT ( 'NONE',  ( 0.2927782761540232426, -1.083998813092891700, 0.8148780714178450735 ) ) ;
#20876 = CARTESIAN_POINT ( 'NONE',  ( 0.03113248654051816583, -0.3829990175980249600, -0.3390339253215535198 ) ) ;
#20875 = CARTESIAN_POINT ( 'NONE',  ( 0.3410005206520395626, -1.758673451842764246, 0.4621779736240644310 ) ) ;
#20877 = CARTESIAN_POINT ( 'NONE',  ( 0.09805242145838190260, -1.310054031134215036, 0.5682417262808774350 ) ) ;
#20878 = ORIENTED_EDGE ( 'NONE', *, *, #13555, .T. ) ;
#20879 = ORIENTED_EDGE ( 'NONE', *, *, #13765, .F. ) ;
#20880 = CARTESIAN_POINT ( 'NONE',  ( 0.03650581953630565452, -0.5059763899182380120, -0.07647306779615689609 ) ) ;
#20881 = CARTESIAN_POINT ( 'NONE',  ( 0.3158993119317616283, -0.7784124716426810142, 0.7037675960530900277 ) ) ;
#20882 = CARTESIAN_POINT ( 'NONE',  ( 0.4125610653371456493, -1.705653404133229634, -0.6104586881356433015 ) ) ;
#20883 = CARTESIAN_POINT ( 'NONE',  ( 0.3757471142192211344, -1.766731021160330428, -0.5680748514784754732 ) ) ;
#20884 = FACE_OUTER_BOUND ( 'NONE', #24843, .T. ) ;
#20885 = EDGE_CURVE ( 'NONE', #25917, #12964, #13414, .T. ) ;
#20886 = CARTESIAN_POINT ( 'NONE',  ( 0.3931095016817222065, -1.150926721643386497, 0.4182417262808778569 ) ) ;
#20887 = CARTESIAN_POINT ( 'NONE',  ( 0.2842326993136112812, -1.549395603922541831, -0.7208999815284790058 ) ) ;
#20888 = CARTESIAN_POINT ( 'NONE',  ( 0.3149931741451680312, -1.174162082499039084, 0.5426465745000428331 ) ) ;
#20889 = CARTESIAN_POINT ( 'NONE',  ( 0.4727414870697744798, -1.078201156678013639, 0.7478468640933467748 ) ) ;
#20890 = PRODUCT_DEFINITION_SHAPE ( 'NONE', 'NONE',  #20515 ) ;
#20891 = COORDINATED_UNIVERSAL_TIME_OFFSET ( 0, 0, .AHEAD. ) ;
#20892 = DIRECTION ( 'NONE',  ( 0.4999999999999976685, 0.000000000000000000, -0.8660254037844400399 ) ) ;
#20893 = LINE ( 'NONE', #33414, #16002 ) ;
#20894 = CARTESIAN_POINT ( 'NONE',  ( 0.4615400415883951779, -1.655602614066592260, -0.3952887662183799389 ) ) ;
#20895 = ORIENTED_EDGE ( 'NONE', *, *, #40100, .F. ) ;
#20896 = CARTESIAN_POINT ( 'NONE',  ( -0.2399999999999999079, -3.941790907013290823, -0.4084369376873030477 ) ) ;
#20897 = DIRECTION ( 'NONE',  ( 0.8660512985181124668, 0.4999551463232388415, 0.000000000000000000 ) ) ;
#20898 = AXIS2_PLACEMENT_3D ( 'NONE', #31071, #25101, #258 ) ;
#20899 = CARTESIAN_POINT ( 'NONE',  ( -0.03478556507500340372, -0.3590471004907262453, -0.3712136264428358423 ) ) ;
#20900 = ORIENTED_EDGE ( 'NONE', *, *, #28279, .T. ) ;
#20901 = DIRECTION ( 'NONE',  ( 0.000000000000000000, 0.000000000000000000, 1.000000000000000000 ) ) ;
#20902 = CARTESIAN_POINT ( 'NONE',  ( 0.3984114568195522010, -1.599003643269838904, -0.5155029497116575543 ) ) ;
#20903 = CARTESIAN_POINT ( 'NONE',  ( 0.2171196146447029740, -1.332674774804728290, 0.6488356689647567510 ) ) ;
#20904 = ORIENTED_EDGE ( 'NONE', *, *, #24114, .T. ) ;
#20905 = CARTESIAN_POINT ( 'NONE',  ( 0.2572301429339545198, -1.333641270216179286, 0.5682417262808723279 ) ) ;
#20906 = CARTESIAN_POINT ( 'NONE',  ( 0.02881195911414760266, -0.06013796869037528470, 0.4945549975361901440 ) ) ;
#20907 = CARTESIAN_POINT ( 'NONE',  ( 0.3812071769896587803, -1.763750790280042002, -0.4536492913031247021 ) ) ;
#20908 = DIRECTION ( 'NONE',  ( 0.000000000000000000, 0.000000000000000000, -1.000000000000000000 ) ) ;
#20909 = CARTESIAN_POINT ( 'NONE',  ( 0.4690544269859369675, -1.240261309394489642, 0.5870667310821602314 ) ) ;
#20910 = ADVANCED_FACE ( 'NONE', ( #10416 ), #29186, .T. ) ;
#20912 = CARTESIAN_POINT ( 'NONE',  ( 0.3999999999999787059, -2.097675824466503691, -0.5196396315034578217 ) ) ;
#20911 = CARTESIAN_POINT ( 'NONE',  ( 0.05279185365593443841, 0.4562178057547968679, 0.1062796545749007671 ) ) ;
#20913 = DIRECTION ( 'NONE',  ( 1.000000000000000000, -0.000000000000000000, -0.000000000000000000 ) ) ;
#20914 = ORIENTED_EDGE ( 'NONE', *, *, #29852, .T. ) ;
#20915 = ORIENTED_EDGE ( 'NONE', *, *, #19499, .T. ) ;
#20916 = CARTESIAN_POINT ( 'NONE',  ( 0.3948505749141573151, -1.157343825514034918, 0.4182417262808776903 ) ) ;
#20917 = VERTEX_POINT ( 'NONE', #22977 ) ;
#20918 =( BOUNDED_SURFACE ( )  B_SPLINE_SURFACE ( 3, 2, ( 
 ( #13375, #38668, #19956 ),
 ( #4314, #16272, #1077 ),
 ( #16667, #31903, #7178 ),
 ( #32488, #38476, #28812 ),
 ( #7380, #16878, #7598 ),
 ( #13162, #3905, #32283 ),
 ( #38062, #20172, #32698 ),
 ( #16071, #486, #9874 ),
 ( #4102, #10486, #1266 ),
 ( #25949, #26333, #10307 ) ),
 .UNSPECIFIED., .F., .F., .T. ) 
 B_SPLINE_SURFACE_WITH_KNOTS ( ( 4, 2, 2, 2, 4 ),
 ( 3, 3 ),
 ( 0.001615335599980216629, 0.002812013140722832618, 0.003111182525908486561, 0.003410351911094140938, 0.004008690681465448824 ),
 ( 0.000000000000000000, 1.000000000000000000 ),
 .UNSPECIFIED. ) 
 GEOMETRIC_REPRESENTATION_ITEM ( )  RATIONAL_B_SPLINE_SURFACE ( (
 ( 1.000000000000000000, 0.8170441014559525206, 1.000000000000000000),
 ( 1.000000000000000000, 0.8398996753289208472, 1.000000000000000000),
 ( 1.000000000000000000, 0.8580894509173602192, 1.000000000000000000),
 ( 1.000000000000000000, 0.8737185627151831113, 1.000000000000000000),
 ( 1.000000000000000000, 0.8764984143296298269, 1.000000000000000000),
 ( 1.000000000000000000, 0.8812237365503433617, 1.000000000000000000),
 ( 1.000000000000000000, 0.8832013687233702948, 1.000000000000000000),
 ( 1.000000000000000000, 0.8880237859985680160, 1.000000000000000000),
 ( 1.000000000000000000, 0.8897420245345738499, 1.000000000000000000),
 ( 1.000000000000000000, 0.8897565210025812910, 1.000000000000000000) ) ) 
 REPRESENTATION_ITEM ( '' )  SURFACE ( )  );
#20919 = CARTESIAN_POINT ( 'NONE',  ( 0.1917248655069789809, -0.6407273034312881421, 0.1015045423513593059 ) ) ;
#20920 = CARTESIAN_POINT ( 'NONE',  ( 0.4438802985545475810, -1.570449409196589041, 0.6444032079186845507 ) ) ;
#20922 = FACE_OUTER_BOUND ( 'NONE', #20290, .T. ) ;
#20921 = CARTESIAN_POINT ( 'NONE',  ( 0.06831379255928186900, -0.5749909519026226157, 0.04969217839999666431 ) ) ;
#20923 = CARTESIAN_POINT ( 'NONE',  ( 0.4838398748940612726, -1.167039897535582682, 0.4225238715116874655 ) ) ;
#20924 = ORIENTED_EDGE ( 'NONE', *, *, #9941, .T. ) ;
#20925 = CARTESIAN_POINT ( 'NONE',  ( 0.3883123751121188572, -1.905506865536376493, -0.5089180440232635716 ) ) ;
#20926 = CARTESIAN_POINT ( 'NONE',  ( 0.1240259653398129713, -0.5782917783936175615, 0.2638625179588850456 ) ) ;
#20927 = FACE_OUTER_BOUND ( 'NONE', #1836, .T. ) ;
#20928 = DIRECTION ( 'NONE',  ( 1.000000000000000000, 0.000000000000000000, 0.000000000000000000 ) ) ;
#20929 = CARTESIAN_POINT ( 'NONE',  ( 0.6350751079694297863, -1.569022301146391962, 0.4218919778450955782 ) ) ;
#20930 = CARTESIAN_POINT ( 'NONE',  ( 0.1372793408763309797, -1.276325292378077236, 0.4310377198975363089 ) ) ;
#20931 = CARTESIAN_POINT ( 'NONE',  ( 0.003157924493107725546, -0.5245024639201223415, 0.1457192838223093367 ) ) ;
#20932 = CARTESIAN_POINT ( 'NONE',  ( 0.08861584565946885317, -0.6039893155899630495, 0.02242969405406716743 ) ) ;
#20933 = CARTESIAN_POINT ( 'NONE',  ( 0.1878356035704684124, -0.4698003021450733452, 0.2206963598966235063 ) ) ;
#20934 = CARTESIAN_POINT ( 'NONE',  ( 0.08222542156927244161, -1.327483614382554800, 0.4683366274854123823 ) ) ;
#20935 = CARTESIAN_POINT ( 'NONE',  ( 0.01128729522791821309, -0.9461985897322298111, 0.1806064185212560014 ) ) ;
#20936 = CARTESIAN_POINT ( 'NONE',  ( 0.5762373068470778570, -1.611384107284732137, -0.4870925628601384672 ) ) ;
#20937 = DIRECTION ( 'NONE',  ( 0.5113178712883763577, 0.8593916653663353777, -8.996534555025795202E-14 ) ) ;
#20938 = CARTESIAN_POINT ( 'NONE',  ( 0.5675929565786681508, -1.617839747320475086, 0.5725551038798919468 ) ) ;
#20939 = CARTESIAN_POINT ( 'NONE',  ( 0.02235124290213221648, 0.3550643254722137820, -0.3695962758878520993 ) ) ;
#20940 = CARTESIAN_POINT ( 'NONE',  ( 0.5991966895601555931, -1.596821569857824752, 0.4287152735839648843 ) ) ;
#20941 = CARTESIAN_POINT ( 'NONE',  ( 0.05109603825399443300, -0.7331182637548316894, 0.7465514741729609716 ) ) ;
#20942 = DIRECTION ( 'NONE',  ( -0.4999551463232372317, 0.8660512985181135770, -0.000000000000000000 ) ) ;
#20943 = DIRECTION ( 'NONE',  ( -2.465190328815661892E-32, -1.000000000000000000, -6.656013887802287108E-31 ) ) ;
#20944 = CARTESIAN_POINT ( 'NONE',  ( 0.4332356878749745177, -1.705790429466398583, 0.6052722225822104729 ) ) ;
#20945 = CONICAL_SURFACE ( 'NONE', #28814, 0.1762268159172233339, 0.7853981633974500554 ) ;
#20946 = VERTEX_POINT ( 'NONE', #32210 ) ;
#20947 = LINE ( 'NONE', #24236, #10591 ) ;
#20948 = CARTESIAN_POINT ( 'NONE',  ( 0.3918182118607618225, -1.107073211027153725, 0.6042946153017961786 ) ) ;
#20949 = CARTESIAN_POINT ( 'NONE',  ( -0.1743922129835736579, -0.5166151207188712791, 0.3599999999999997091 ) ) ;
#20950 = CARTESIAN_POINT ( 'NONE',  ( -0.04293317454820687329, 0.2295413494973353175, -0.4381202835071930091 ) ) ;
#20951 = CARTESIAN_POINT ( 'NONE',  ( 0.4842931683238080320, -1.270018078534612904, 0.7216184661905129527 ) ) ;
#20953 = ORIENTED_EDGE ( 'NONE', *, *, #38358, .T. ) ;
#20952 = CARTESIAN_POINT ( 'NONE',  ( -0.1699617389507570020, 0.4951775333576697302, 0.1374137075621912063 ) ) ;
#20954 = CARTESIAN_POINT ( 'NONE',  ( 0.5067209442253272078, -1.108407892246341175, 0.6081930138323172752 ) ) ;
#20955 = VERTEX_POINT ( 'NONE', #3829 ) ;
#20956 = ADVANCED_FACE ( 'NONE', ( #16593 ), #22633, .T. ) ;
#20957 = EDGE_CURVE ( 'NONE', #21489, #39928, #27231, .T. ) ;
#20958 = CARTESIAN_POINT ( 'NONE',  ( -2.070754768975505034, -0.09959325338431362917, 0.3749999999999976130 ) ) ;
#20959 = VERTEX_POINT ( 'NONE', #3643 ) ;
#20960 = DIRECTION ( 'NONE',  ( -0.8660512985181132439, -0.4999551463232374537, 0.000000000000000000 ) ) ;
#20961 = ORIENTED_EDGE ( 'NONE', *, *, #7371, .T. ) ;
#20962 = CARTESIAN_POINT ( 'NONE',  ( 0.3558919305822700330, -1.622312069902127840, 0.5706928582630780289 ) ) ;
#20964 = CARTESIAN_POINT ( 'NONE',  ( 0.1773295416277048953, -0.4575625385501337350, 0.1501579634321036083 ) ) ;
#20963 = CARTESIAN_POINT ( 'NONE',  ( 0.7057303773600904773, -1.512934555508332668, 0.5564953324639242416 ) ) ;
#20965 = LINE ( 'NONE', #8588, #17496 ) ;
#20966 = EDGE_CURVE ( 'NONE', #24008, #21212, #411, .T. ) ;
#20967 = ORIENTED_EDGE ( 'NONE', *, *, #15369, .F. ) ;
#20968 = ADVANCED_FACE ( 'NONE', ( #22375 ), #792, .T. ) ;
#20969 = ORIENTED_EDGE ( 'NONE', *, *, #38693, .T. ) ;
#20970 = CARTESIAN_POINT ( 'NONE',  ( 0.1648393044702914367, -1.273995379727181021, 0.4182417262808778569 ) ) ;
#20971 = LINE ( 'NONE', #31028, #23094 ) ;
#20972 = CARTESIAN_POINT ( 'NONE',  ( 0.2054732354593832022, -1.060600144931224342, 0.7368794145240139537 ) ) ;
#20973 = CARTESIAN_POINT ( 'NONE',  ( -0.05464101615137785528, -2.180132361182266720, -0.6941833704005058170 ) ) ;
#20974 = DIRECTION ( 'NONE',  ( -0.4999551463232371762, 0.8660512985181134660, -0.000000000000000000 ) ) ;
#20975 = CARTESIAN_POINT ( 'NONE',  ( 0.1597138714205091625, -0.9558088324725364515, 0.4497724057842478751 ) ) ;
#20976 = FACE_OUTER_BOUND ( 'NONE', #39161, .T. ) ;
#20977 = CARTESIAN_POINT ( 'NONE',  ( 0.3534995746758727853, -1.163432996101295025, 0.4351399550592107701 ) ) ;
#20978 = EDGE_CURVE ( 'NONE', #15491, #26696, #17381, .T. ) ;
#20979 = CARTESIAN_POINT ( 'NONE',  ( 0.4012199348250638509, -1.136392022378372113, 0.4815844951853371358 ) ) ;
#20980 = CARTESIAN_POINT ( 'NONE',  ( 0.03852435536883173223, -1.195394391876414719, 0.6677169776219902264 ) ) ;
#20981 = COORDINATED_UNIVERSAL_TIME_OFFSET ( 0, 0, .AHEAD. ) ;
#20982 = APPLIED_PERSON_AND_ORGANIZATION_ASSIGNMENT ( #30088, #1916, ( #35536 ) ) ;
#20983 = CARTESIAN_POINT ( 'NONE',  ( 0.4437585245673965617, -1.132310435069097565, 0.4450710391304853464 ) ) ;
#20984 = CARTESIAN_POINT ( 'NONE',  ( 0.04154009738085341630, -0.4416556227939135715, 0.1617111092119885296 ) ) ;
#20985 = CARTESIAN_POINT ( 'NONE',  ( 0.7087227687136311571, -1.504650563340975022, 0.5335643800121802061 ) ) ;
#20986 = PRODUCT_DEFINITION_SHAPE ( 'NONE', 'NONE',  #25768 ) ;
#20987 = CARTESIAN_POINT ( 'NONE',  ( 0.0001866439489153905271, -0.5339630687492940009, -0.05105682221463851006 ) ) ;
#20988 = CARTESIAN_POINT ( 'NONE',  ( 0.3769667398768312694, -1.761641512302731138, -0.5722193458963301671 ) ) ;
#20989 = CARTESIAN_POINT ( 'NONE',  ( 0.03892492223551621139, -0.6940895124628043700, 0.6890254284164284426 ) ) ;
#20990 = CARTESIAN_POINT ( 'NONE',  ( -0.01548846960707545191, -0.2306506793134033284, 0.4716198300880330985 ) ) ;
#20991 = ORIENTED_EDGE ( 'NONE', *, *, #11200, .T. ) ;
#20992 = VERTEX_POINT ( 'NONE', #19674 ) ;
#20993 = CARTESIAN_POINT ( 'NONE',  ( 0.2948640431575899057, -1.208698857598578869, 0.4182417262808778013 ) ) ;
#20994 = VERTEX_POINT ( 'NONE', #25461 ) ;
#20995 = DIRECTION ( 'NONE',  ( 0.8660254037844378194, -0.3535533905932747856, 0.3535533905932747856 ) ) ;
#20996 = CARTESIAN_POINT ( 'NONE',  ( -0.1204846181304667641, -0.5035940506942969686, 0.1366987775887329726 ) ) ;
#20998 = ORIENTED_EDGE ( 'NONE', *, *, #35891, .F. ) ;
#20997 = CARTESIAN_POINT ( 'NONE',  ( 0.001011648560469348857, -0.5841484436987858242, 0.01311714344844475653 ) ) ;
#20999 = EDGE_CURVE ( 'NONE', #11394, #8287, #33114, .T. ) ;
#21000 = ORIENTED_EDGE ( 'NONE', *, *, #35990, .T. ) ;
#21001 = DIRECTION ( 'NONE',  ( -1.000000000000000000, -2.280301054154495132E-31, 1.664003471950577689E-31 ) ) ;
#21002 = EDGE_CURVE ( 'NONE', #12958, #16211, #20003, .T. ) ;
#21003 = ORIENTED_EDGE ( 'NONE', *, *, #11027, .F. ) ;
#21004 = CARTESIAN_POINT ( 'NONE',  ( 0.006823764970969815359, -0.6154038265784372852, 0.4059195148818033339 ) ) ;
#21006 = CARTESIAN_POINT ( 'NONE',  ( 0.2186880164441438179, -1.240563195108393080, 0.5774983274694442947 ) ) ;
#21005 = CARTESIAN_POINT ( 'NONE',  ( 0.1909286924077255032, -1.257064795538239022, -0.3194753470178354759 ) ) ;
#21007 = CARTESIAN_POINT ( 'NONE',  ( 0.2624674271213696675, -1.608515928549841822, -0.3523228403142553145 ) ) ;
#21008 = COORDINATED_UNIVERSAL_TIME_OFFSET ( 0, 0, .AHEAD. ) ;
#21009 = EDGE_CURVE ( 'NONE', #32432, #35619, #14085, .T. ) ;
#21010 = CARTESIAN_POINT ( 'NONE',  ( 0.2059273467974227778, -1.283046334493782359, -0.7137159211901564770 ) ) ;
#21012 = ORIENTED_EDGE ( 'NONE', *, *, #12000, .F. ) ;
#21011 = ORIENTED_EDGE ( 'NONE', *, *, #4579, .F. ) ;
#21013 = ADVANCED_FACE ( 'NONE', ( #31615 ), #19284, .T. ) ;
#21014 = CYLINDRICAL_SURFACE ( 'NONE', #8636, 0.04330708661417343591 ) ;
#21015 = CARTESIAN_POINT ( 'NONE',  ( 0.1809966328114128442, -1.222385076516254054, -0.5155029497116575543 ) ) ;
#21016 = CARTESIAN_POINT ( 'NONE',  ( 0.2705165854423337013, -0.9635601006052144646, 0.7153668490100312249 ) ) ;
#21017 = CARTESIAN_POINT ( 'NONE',  ( 0.1874317355884921321, -0.6912902591703241617, 0.04192882835670527081 ) ) ;
#21018 = CARTESIAN_POINT ( 'NONE',  ( -0.01736481776669303659, -0.5247326629091749739, 0.1457185332388703236 ) ) ;
#21019 = CARTESIAN_POINT ( 'NONE',  ( -0.01548846960707463312, 0.4638115001430995199, 0.2459753896937826034 ) ) ;
#21020 = DIRECTION ( 'NONE',  ( 0.8660512985181134660, 0.4999551463232372317, 0.000000000000000000 ) ) ;
#21021 = FACE_BOUND ( 'NONE', #8022, .T. ) ;
#21022 = FACE_OUTER_BOUND ( 'NONE', #22082, .T. ) ;
#21023 = CARTESIAN_POINT ( 'NONE',  ( 0.4584370907333497058, -1.110107490588079671, 0.5683196366401116473 ) ) ;
#21024 = EDGE_CURVE ( 'NONE', #7506, #36513, #8151, .T. ) ;
#21025 = CARTESIAN_POINT ( 'NONE',  ( 0.3884858366675985053, -1.658196668589008382, -0.4078262653169359431 ) ) ;
#21026 =( NAMED_UNIT ( * ) PLANE_ANGLE_UNIT ( ) SI_UNIT ( $, .RADIAN. ) );
#21027 = DIRECTION ( 'NONE',  ( 0.000000000000000000, 0.000000000000000000, 1.000000000000000000 ) ) ;
#21028 = CARTESIAN_POINT ( 'NONE',  ( 0.2142493868227219878, -1.379310565402303457, 1.003739045973664368 ) ) ;
#21029 = CARTESIAN_POINT ( 'NONE',  ( 0.4003901567941702822, -1.031933045472551269, 0.6312919426632347397 ) ) ;
#21030 = CARTESIAN_POINT ( 'NONE',  ( 0.03340947221881906959, -0.9865371011752580577, 0.6764581597365023624 ) ) ;
#21031 = APPROVAL_DATE_TIME ( #27422, #36280 ) ;
#21032 = CARTESIAN_POINT ( 'NONE',  ( 0.3279357908889724005, -0.8116789304350262579, 0.7312476538325396458 ) ) ;
#21033 = B_SPLINE_CURVE_WITH_KNOTS ( 'NONE', 3,
 ( #8085, #20662, #11384, #5001 ),
 .UNSPECIFIED., .F., .F.,
 ( 4, 4 ),
 ( -6.000000000270394880E-08, 0.001522235525887978384 ),
 .UNSPECIFIED. ) ;
#21034 = DIRECTION ( 'NONE',  ( -1.000000000000000000, -0.000000000000000000, -0.000000000000000000 ) ) ;
#21035 = CARTESIAN_POINT ( 'NONE',  ( 0.01899496522502568466, -0.07377983897467746410, -0.5147126279162580476 ) ) ;
#21036 = DIRECTION ( 'NONE',  ( 0.000000000000000000, -6.829619984160655877E-15, -1.000000000000000000 ) ) ;
#21037 = ORIENTED_EDGE ( 'NONE', *, *, #30818, .F. ) ;
#21038 = DIRECTION ( 'NONE',  ( 1.000000000000000000, 0.000000000000000000, 0.000000000000000000 ) ) ;
#21039 = CARTESIAN_POINT ( 'NONE',  ( 0.07380144035736982411, -0.9240663959273383021, 0.7785025519333340638 ) ) ;
#21040 = CARTESIAN_POINT ( 'NONE',  ( 0.1299497688713388832, -0.5790410954462047455, 0.2626379361186624850 ) ) ;
#21041 = CARTESIAN_POINT ( 'NONE',  ( 0.3695052819757338458, -1.758428263776098621, -0.4278193900811942396 ) ) ;
#21043 = ORIENTED_EDGE ( 'NONE', *, *, #34585, .T. ) ;
#21042 = CARTESIAN_POINT ( 'NONE',  ( 0.3839459786000343211, -1.830045642923745941, -0.5208591197437392184 ) ) ;
#21044 = CARTESIAN_POINT ( 'NONE',  ( 0.2529714763052502979, -0.7233805682233873657, 0.5452257223911994855 ) ) ;
#21046 = VERTEX_POINT ( 'NONE', #6709 ) ;
#21045 = ORIENTED_EDGE ( 'NONE', *, *, #8886, .T. ) ;
#21047 = CARTESIAN_POINT ( 'NONE',  ( 0.1512218670170321910, -1.285950302238538345, -0.7264183920055864441 ) ) ;
#21048 = EDGE_CURVE ( 'NONE', #27585, #28698, #36404, .T. ) ;
#21049 = LINE ( 'NONE', #11176, #21080 ) ;
#21050 = DIRECTION ( 'NONE',  ( 0.9766636885342061536, -0.2147743920926307448, 0.000000000000000000 ) ) ;
#21051 = SECURITY_CLASSIFICATION_LEVEL ( 'unclassified' ) ;
#21052 = EDGE_CURVE ( 'NONE', #5057, #30904, #10013, .T. ) ;
#21053 = AXIS2_PLACEMENT_3D ( 'NONE', #3041, #6501, #9798 ) ;
#21054 = DIRECTION ( 'NONE',  ( 0.000000000000000000, 0.8090169943749455639, -0.5877852522924756906 ) ) ;
#21055 = ORIENTED_EDGE ( 'NONE', *, *, #28029, .F. ) ;
#21056 = DIRECTION ( 'NONE',  ( -0.4999551463232372317, 0.8660512985181135770, -0.000000000000000000 ) ) ;
#21057 = EDGE_CURVE ( 'NONE', #11876, #20340, #9479, .T. ) ;
#21058 = CARTESIAN_POINT ( 'NONE',  ( 0.2639495433093203558, -0.9686959132792163363, 0.6974367203216930156 ) ) ;
#21059 = CARTESIAN_POINT ( 'NONE',  ( 0.2030024116509572818, -1.310890633394409033, 1.024740945452946361 ) ) ;
#21060 = CARTESIAN_POINT ( 'NONE',  ( 0.1094109803698096878, -0.6218279727836852899, 0.3761239768809111483 ) ) ;
#21062 = CARTESIAN_POINT ( 'NONE',  ( 0.0009970652039437085962, -0.5853685308490127470, 0.01218434430457844379 ) ) ;
#21061 = FACE_OUTER_BOUND ( 'NONE', #11453, .T. ) ;
#21063 = CARTESIAN_POINT ( 'NONE',  ( 0.003383243044336568025, -0.9698986547711589967, 0.4010568066359272987 ) ) ;
#21064 = ORIENTED_EDGE ( 'NONE', *, *, #33934, .F. ) ;
#21065 = EDGE_CURVE ( 'NONE', #4571, #19277, #29742, .T. ) ;
#21066 = ORIENTED_EDGE ( 'NONE', *, *, #39929, .T. ) ;
#21067 = CARTESIAN_POINT ( 'NONE',  ( 0.03654364704248769941, -0.4542255574219836722, -0.2354487068768244262 ) ) ;
#21068 = CARTESIAN_POINT ( 'NONE',  ( 0.2686022046095623006, -0.8300817956324447744, 0.7674347935952442468 ) ) ;
#21069 = CARTESIAN_POINT ( 'NONE',  ( -0.05464101615137762630, -2.183180860297908144, -0.4937760292030871079 ) ) ;
#21070 = EDGE_CURVE ( 'NONE', #21929, #5559, #23408, .T. ) ;
#21071 = SPHERICAL_SURFACE ( 'NONE', #19939, 0.01499999999999999944 ) ;
#21072 = LENGTH_MEASURE_WITH_UNIT ( LENGTH_MEASURE( 0.02539999999999999897 ), #24780 );
#21073 = EDGE_CURVE ( 'NONE', #22141, #37239, #16807, .T. ) ;
#21074 = CARTESIAN_POINT ( 'NONE',  ( -0.2399999999999999079, -3.745280840418592661, 0.04438736989695814955 ) ) ;
#21075 = EDGE_CURVE ( 'NONE', #24709, #38007, #34081, .T. ) ;
#21076 = CARTESIAN_POINT ( 'NONE',  ( 0.1363389461966361682, -1.302049561124409838, -0.6870159582249631969 ) ) ;
#21077 = CARTESIAN_POINT ( 'NONE',  ( 0.2089316498445973613, -0.7245868578893045475, 0.3779356710034222910 ) ) ;
#21078 = COORDINATED_UNIVERSAL_TIME_OFFSET ( 0, 0, .AHEAD. ) ;
#21079 = DIRECTION ( 'NONE',  ( -1.000000000000000000, -0.000000000000000000, -0.000000000000000000 ) ) ;
#21080 = VECTOR ( 'NONE', #14450, 39.37007874015748143 ) ;
#21081 = CARTESIAN_POINT ( 'NONE',  ( 0.1862037248930970834, -1.944818472745344584, -0.6629142544188069142 ) ) ;
#21082 = ORIENTED_EDGE ( 'NONE', *, *, #31086, .T. ) ;
#21083 = CARTESIAN_POINT ( 'NONE',  ( 0.05999999999999990757, 0.1428018198284763673, -0.2638325989215043466 ) ) ;
#21084 = DIRECTION ( 'NONE',  ( -0.4999551463232372317, 0.8660512985181135770, -0.000000000000000000 ) ) ;
#21085 = EDGE_CURVE ( 'NONE', #20761, #36543, #18024, .T. ) ;
#21086 = CARTESIAN_POINT ( 'NONE',  ( -0.1157923916715200702, -0.5295015842444287246, 0.3181161673586325178 ) ) ;
#21087 = VECTOR ( 'NONE', #9850, 39.37007874015748143 ) ;
#21088 = EDGE_LOOP ( 'NONE', ( #23338, #15486, #38498, #10775, #36681 ) ) ;
#21089 = DIRECTION ( 'NONE',  ( 0.8660512985181126888, 0.4999551463232385085, 0.000000000000000000 ) ) ;
#21090 = VECTOR ( 'NONE', #2020, 39.37007874015748143 ) ;
#21091 = LINE ( 'NONE', #39803, #22631 ) ;
#21092 = CARTESIAN_POINT ( 'NONE',  ( -0.04945776359514544862, 0.03517487494623269817, -0.4760216296475741071 ) ) ;
#21093 = CARTESIAN_POINT ( 'NONE',  ( 0.07311138962147617493, -0.9435636872638024641, 0.6307374715929325859 ) ) ;
#21094 = ORIENTED_EDGE ( 'NONE', *, *, #36821, .T. ) ;
#21095 = CARTESIAN_POINT ( 'NONE',  ( 0.03650581953630542553, 0.3643937567481987938, 0.3592734714612024760 ) ) ;
#21096 = DIRECTION ( 'NONE',  ( 1.188678714063518819E-15, -1.000000000000000000, 0.000000000000000000 ) ) ;
#21097 = CARTESIAN_POINT ( 'NONE',  ( 0.03672447062657951955, -0.4682441148239235851, -0.1092390724017577447 ) ) ;
#21098 = DIRECTION ( 'NONE',  ( -0.000000000000000000, 0.3090169943749569437, 0.9510565162951504226 ) ) ;
#21099 = CARTESIAN_POINT ( 'NONE',  ( 0.4381232881540311208, -1.195278502452886915, 0.6782187811958457768 ) ) ;
#21100 = EDGE_CURVE ( 'NONE', #11941, #27170, #5534, .T. ) ;
#21102 = CARTESIAN_POINT ( 'NONE',  ( 0.0003671528708184450067, -0.4356477474403453454, 0.1457185332388686860 ) ) ;
#21101 = CARTESIAN_POINT ( 'NONE',  ( -0.08402031424619242628, 0.05739311687334405082, 0.1044725468576922639 ) ) ;
#21103 = DIRECTION ( 'NONE',  ( -1.000000000000000000, -0.000000000000000000, -0.000000000000000000 ) ) ;
#21104 = ORIENTED_EDGE ( 'NONE', *, *, #23350, .F. ) ;
#21105 = ADVANCED_FACE ( 'NONE', ( #26872 ), #7522, .T. ) ;
#21106 = FACE_OUTER_BOUND ( 'NONE', #25753, .T. ) ;
#21107 = ORIENTED_EDGE ( 'NONE', *, *, #25286, .T. ) ;
#21108 = DIRECTION ( 'NONE',  ( 0.000000000000000000, 0.000000000000000000, -1.000000000000000000 ) ) ;
#21109 = CARTESIAN_POINT ( 'NONE',  ( 0.1857207782009835662, -0.9735509886838665805, 0.7778221052609431974 ) ) ;
#21111 = CARTESIAN_POINT ( 'NONE',  ( 0.1925852169268471858, -0.7535752542798960230, 0.3142616005574464522 ) ) ;
#21110 = CARTESIAN_POINT ( 'NONE',  ( -0.05561176441985712926, -0.4442366066780419342, 0.1229089882096642827 ) ) ;
#21112 = CARTESIAN_POINT ( 'NONE',  ( 0.4926894108487032131, -1.176944786191506109, 0.4224236931107097637 ) ) ;
#21113 = ORIENTED_EDGE ( 'NONE', *, *, #5421, .F. ) ;
#21114 = AXIS2_PLACEMENT_3D ( 'NONE', #40572, #846, #38649 ) ;
#21115 = B_SPLINE_CURVE_WITH_KNOTS ( 'NONE', 3,
 ( #30146, #1975, #20905, #33427 ),
 .UNSPECIFIED., .F., .F.,
 ( 4, 4 ),
 ( 0.01696221039300578257, 0.4968750736215113428 ),
 .UNSPECIFIED. ) ;
#21116 = ORIENTED_EDGE ( 'NONE', *, *, #33780, .T. ) ;
#21117 = CARTESIAN_POINT ( 'NONE',  ( 0.1994740068363775598, -2.042640899752901085, -0.2765909798240092643 ) ) ;
#21118 = AXIS2_PLACEMENT_3D ( 'NONE', #17687, #33327, #11321 ) ;
#21119 = CARTESIAN_POINT ( 'NONE',  ( 0.5735257847173089729, -1.499153090709115510, 0.5657782871807620628 ) ) ;
#21120 = CARTESIAN_POINT ( 'NONE',  ( 0.4194453228269892642, -1.699896402126472195, 0.4182417262805759317 ) ) ;
#21121 = CARTESIAN_POINT ( 'NONE',  ( -0.2399999999999999079, -2.377368549242099949, -0.4802393080720198104 ) ) ;
#21122 = CARTESIAN_POINT ( 'NONE',  ( -0.2746410161513782033, -2.003129936916423048, -0.4197911229995844873 ) ) ;
#21123 = CIRCLE ( 'NONE', #13211, 0.009999999999999995004 ) ;
#21124 = CARTESIAN_POINT ( 'NONE',  ( 0.2094458608486971796, -1.234382894204292702, 0.5645286332426232567 ) ) ;
#21125 = VECTOR ( 'NONE', #27222, 39.37007874015748143 ) ;
#21126 = FACE_OUTER_BOUND ( 'NONE', #36114, .T. ) ;
#21127 = CARTESIAN_POINT ( 'NONE',  ( 0.2161540139445707054, -1.242273860952007203, 0.4569645709156981428 ) ) ;
#21128 = CARTESIAN_POINT ( 'NONE',  ( 0.2120163453477715010, -0.5915265038663817254, 0.4276896445164236615 ) ) ;
#21129 = CARTESIAN_POINT ( 'NONE',  ( 0.07958551560962270899, -1.322831287755755758, 0.4682677590956452196 ) ) ;
#21130 = DIRECTION ( 'NONE',  ( 0.000000000000000000, 0.000000000000000000, -1.000000000000000000 ) ) ;
#21132 = AXIS2_PLACEMENT_3D ( 'NONE', #27845, #12402, #37586 ) ;
#21131 = CARTESIAN_POINT ( 'NONE',  ( 0.6103063930502474754, -1.581064649372068143, -0.5712514945930247112 ) ) ;
#21133 = CARTESIAN_POINT ( 'NONE',  ( 0.04285427992854282803, 0.2295125098185389900, 0.4383721679652319847 ) ) ;
#21134 = CARTESIAN_POINT ( 'NONE',  ( 0.6672263256166468537, -1.559577713309568292, 0.6159734170043985602 ) ) ;
#21135 = CARTESIAN_POINT ( 'NONE',  ( 0.6795582604384902137, -1.448051739356461365, 0.4670391094899577489 ) ) ;
#21136 = DIRECTION ( 'NONE',  ( -1.000000000000000000, 0.000000000000000000, 0.000000000000000000 ) ) ;
#21137 = VERTEX_POINT ( 'NONE', #39403 ) ;
#21138 = CARTESIAN_POINT ( 'NONE',  ( 0.01707166242847063184, -0.6102210326195973700, 0.5232503585198154950 ) ) ;
#21139 = CARTESIAN_POINT ( 'NONE',  ( 0.3746913172999769004, -1.707304890831578659, -0.6133074500811318552 ) ) ;
#21140 = CARTESIAN_POINT ( 'NONE',  ( 0.3999999999999787059, -2.097675824466503691, -0.4688691127277797022 ) ) ;
#21141 = AXIS2_PLACEMENT_3D ( 'NONE', #17611, #4244, #7527 ) ;
#21142 = PLANE ( 'NONE',  #33796 ) ;
#21143 = ORIENTED_EDGE ( 'NONE', *, *, #2096, .F. ) ;
#21144 = CARTESIAN_POINT ( 'NONE',  ( -0.01548846960707517956, -0.3772621329472698459, 0.3651003739303452234 ) ) ;
#21145 = AXIS2_PLACEMENT_3D ( 'NONE', #3543, #28651, #6820 ) ;
#21146 =( BOUNDED_SURFACE ( )  B_SPLINE_SURFACE ( 3, 2, ( 
 ( #17190, #4825, #39398 ),
 ( #13693, #38777, #29737 ),
 ( #10607, #23183, #23402 ),
 ( #17396, #1581, #35709 ),
 ( #14306, #30557, #37132 ),
 ( #2177, #27063, #18206 ),
 ( #5041, #36919, #5433 ),
 ( #17603, #17998, #14496 ),
 ( #20701, #14921, #33428 ),
 ( #12038, #27476, #8733 ),
 ( #24598, #24806, #33233 ),
 ( #8945, #14716, #2574 ),
 ( #24195, #27279, #21310 ),
 ( #15110, #21521, #33849 ),
 ( #20906, #5651, #2776 ),
 ( #8337, #2379, #33621 ),
 ( #40001, #5234, #30148 ),
 ( #34038, #40418, #5839 ) ),
 .UNSPECIFIED., .F., .F., .F. ) 
 B_SPLINE_SURFACE_WITH_KNOTS ( ( 4, 2, 2, 2, 2, 2, 2, 2, 4 ),
 ( 3, 3 ),
 ( -0.001532620576208851846, -0.0007637936630077643823, 5.033250193322972611E-06, 0.0007738601633944103275, 0.001542687076595497791, 0.002311513989796585254, 0.003080340902997672284, 0.003849167816198759747, 0.004617994729399847210 ),
 ( 0.000000000000000000, 1.000000000000000000 ),
 .UNSPECIFIED. ) 
 GEOMETRIC_REPRESENTATION_ITEM ( )  RATIONAL_B_SPLINE_SURFACE ( (
 ( 1.000000000000000000, 0.7283825911960444266, 1.000000000000000000),
 ( 1.000000000000000000, 0.7404385082113551508, 1.000000000000000000),
 ( 1.000000000000000000, 0.7521504257739064503, 1.000000000000000000),
 ( 1.000000000000000000, 0.7744497410760828870, 1.000000000000000000),
 ( 1.000000000000000000, 0.7845654757375588595, 1.000000000000000000),
 ( 1.000000000000000000, 0.8022083990890596095, 1.000000000000000000),
 ( 1.000000000000000000, 0.8094167424698901492, 1.000000000000000000),
 ( 1.000000000000000000, 0.8194491993617027958, 1.000000000000000000),
 ( 1.000000000000000000, 0.8220634900780797727, 1.000000000000000000),
 ( 1.000000000000000000, 0.8220705070823152161, 1.000000000000000000),
 ( 1.000000000000000000, 0.8194468812481560116, 1.000000000000000000),
 ( 1.000000000000000000, 0.8094220769838861296, 1.000000000000000000),
 ( 1.000000000000000000, 0.8022659121983863884, 1.000000000000000000),
 ( 1.000000000000000000, 0.7845681159037143360, 1.000000000000000000),
 ( 1.000000000000000000, 0.7744426415184757495, 1.000000000000000000),
 ( 1.000000000000000000, 0.7522890290929225010, 1.000000000000000000),
 ( 1.000000000000000000, 0.7403540167214970324, 1.000000000000000000),
 ( 1.000000000000000000, 0.7283825911960213340, 1.000000000000000000) ) ) 
 REPRESENTATION_ITEM ( '' )  SURFACE ( )  );
#21147 = AXIS2_PLACEMENT_3D ( 'NONE', #29627, #4327, #683 ) ;
#21148 = CARTESIAN_POINT ( 'NONE',  ( 0.3227141990867507526, -1.181380599211185212, 0.5734485983774162410 ) ) ;
#21149 = DIRECTION ( 'NONE',  ( 0.9998941247116547304, -0.01455087607601020412, 0.0001066420868422379633 ) ) ;
#21150 = CARTESIAN_POINT ( 'NONE',  ( -0.02953079040095700838, 0.2329676531120452587, -0.4763574306556336291 ) ) ;
#21151 = AXIS2_PLACEMENT_3D ( 'NONE', #34491, #6304, #594 ) ;
#21152 = CARTESIAN_POINT ( 'NONE',  ( 0.4773756200668168859, -1.258275737217217527, 0.7110155661270410876 ) ) ;
#21154 = ORIENTED_EDGE ( 'NONE', *, *, #2658, .T. ) ;
#21153 = LINE ( 'NONE', #21973, #12741 ) ;
#21155 = CARTESIAN_POINT ( 'NONE',  ( 0.4718294406633598559, -1.074170765704426822, 0.6461978756939577018 ) ) ;
#21156 = ORIENTED_EDGE ( 'NONE', *, *, #5610, .T. ) ;
#21157 = CARTESIAN_POINT ( 'NONE',  ( -0.1509132741912892484, 0.4664843738648666305, 0.09813923389061192382 ) ) ;
#21158 = ORIENTED_EDGE ( 'NONE', *, *, #25816, .T. ) ;
#21159 = DIRECTION ( 'NONE',  ( 0.000000000000000000, 0.5365213554527469286, -0.8438867430782091006 ) ) ;
#21160 = CARTESIAN_POINT ( 'NONE',  ( 0.3587861683550780389, -1.611959099284976160, 0.6979777834575303652 ) ) ;
#21162 = CARTESIAN_POINT ( 'NONE',  ( -0.03662792686184376811, -0.3149733899719669439, 0.3635662525351520125 ) ) ;
#21161 = CARTESIAN_POINT ( 'NONE',  ( 0.06536555028605087192, -0.7987193142509114718, 0.04805781248889415963 ) ) ;
#21163 = CARTESIAN_POINT ( 'NONE',  ( 0.1424029337235096226, -1.400533250147911746, -0.3244367222852112542 ) ) ;
#21164 = VERTEX_POINT ( 'NONE', #1797 ) ;
#21165 = ORIENTED_EDGE ( 'NONE', *, *, #34368, .F. ) ;
#21166 = CARTESIAN_POINT ( 'NONE',  ( 0.4492966705992636478, -1.050346012740955626, 0.6361637604917406152 ) ) ;
#21167 = ORIENTED_EDGE ( 'NONE', *, *, #36924, .T. ) ;
#21168 = DIRECTION ( 'NONE',  ( 0.000000000000000000, 0.9510565162951547524, 0.3090169943749439541 ) ) ;
#21169 = SPHERICAL_SURFACE ( 'NONE', #34904, 0.01499999999999999944 ) ;
#21170 = CARTESIAN_POINT ( 'NONE',  ( 0.1424399877835745010, -0.9312767937703616550, 0.6301790181337186825 ) ) ;
#21171 = CARTESIAN_POINT ( 'NONE',  ( -0.3000000000000000999, -1.739646749720735741, -0.3661865639197241507 ) ) ;
#21172 = CARTESIAN_POINT ( 'NONE',  ( 0.5351545789516157781, -1.658325038984146405, -0.5717893983912645250 ) ) ;
#21173 = CARTESIAN_POINT ( 'NONE',  ( -0.1642263571684414447, 0.5103503754387010982, 0.3032895567580821683 ) ) ;
#21174 = AXIS2_PLACEMENT_3D ( 'NONE', #38151, #29098, #37960 ) ;
#21175 = CARTESIAN_POINT ( 'NONE',  ( 0.7476847780466161497, -1.513986987551942498, 0.3667417262808780887 ) ) ;
#21176 = VECTOR ( 'NONE', #13590, 39.37007874015748143 ) ;
#21177 = DIRECTION ( 'NONE',  ( 1.000000000000000000, 0.000000000000000000, 0.000000000000000000 ) ) ;
#21178 = CARTESIAN_POINT ( 'NONE',  ( 0.6498387395261646660, -1.464631408770378673, 0.4182417262808778013 ) ) ;
#21179 = DIRECTION ( 'NONE',  ( 0.4999551463232372317, -0.8660512985181135770, 0.000000000000000000 ) ) ;
#21180 = COORDINATED_UNIVERSAL_TIME_OFFSET ( 0, 0, .AHEAD. ) ;
#21181 = CIRCLE ( 'NONE', #10011, 0.08000000000000000167 ) ;
#21182 = CARTESIAN_POINT ( 'NONE',  ( 0.4707877201786100918, -1.135202906000321921, 0.4619518047902346214 ) ) ;
#21183 = CARTESIAN_POINT ( 'NONE',  ( 0.4581693818450407463, -1.241628499769009020, 0.6057417262809811076 ) ) ;
#21184 = CARTESIAN_POINT ( 'NONE',  ( 0.3121393770295847747, -1.175762900167912184, 0.5260634940794319814 ) ) ;
#21185 = CARTESIAN_POINT ( 'NONE',  ( 0.01201275324683169846, -0.4797197884825873393, -0.009968709375361768654 ) ) ;
#21186 = DIRECTION ( 'NONE',  ( 0.000000000000000000, -0.7071067811865474617, -0.7071067811865474617 ) ) ;
#21187 = CARTESIAN_POINT ( 'NONE',  ( 0.05241514471239613199, -0.7522610373340221646, 0.7518993562137571418 ) ) ;
#21188 = CARTESIAN_POINT ( 'NONE',  ( 0.3224586748600002384, -1.296590453040780799, 0.4182417262808783009 ) ) ;
#21189 = EDGE_LOOP ( 'NONE', ( #10468, #12237, #1141, #38785, #38652, #17104, #9015, #25811, #23511 ) ) ;
#21190 = VERTEX_POINT ( 'NONE', #20706 ) ;
#21191 = CARTESIAN_POINT ( 'NONE',  ( -0.1127285386968538555, -0.5155187098904498999, 0.1369073159184197586 ) ) ;
#21192 = ORIENTED_EDGE ( 'NONE', *, *, #28847, .F. ) ;
#21193 = CARTESIAN_POINT ( 'NONE',  ( -0.2666757540196709186, 0.4921670437878968851, 0.1000000000000002970 ) ) ;
#21194 = CIRCLE ( 'NONE', #2809, 0.01500000000000001853 ) ;
#21195 = FACE_OUTER_BOUND ( 'NONE', #29140, .T. ) ;
#21197 = ORIENTED_EDGE ( 'NONE', *, *, #37694, .F. ) ;
#21196 = CARTESIAN_POINT ( 'NONE',  ( 0.002371010564581027980, -0.5282417084461772383, 0.1487601318397159811 ) ) ;
#21198 = EDGE_LOOP ( 'NONE', ( #21777, #21470, #29241, #21628 ) ) ;
#21199 = CYLINDRICAL_SURFACE ( 'NONE', #21865, 0.06000000000000031697 ) ;
#21200 = CIRCLE ( 'NONE', #36959, 0.1000000000000000194 ) ;
#21201 = EDGE_LOOP ( 'NONE', ( #34854, #9966, #20444, #8084 ) ) ;
#21202 = VECTOR ( 'NONE', #20526, 39.37007874015748143 ) ;
#21203 = EDGE_CURVE ( 'NONE', #17501, #26475, #32816, .T. ) ;
#21204 = CARTESIAN_POINT ( 'NONE',  ( 0.2705629139958489748, -1.674023155731529711, 0.6420758730732996078 ) ) ;
#21206 = CARTESIAN_POINT ( 'NONE',  ( 0.1128228149019921550, -1.274631681149367646, 0.6181115705952207051 ) ) ;
#21205 = FACE_OUTER_BOUND ( 'NONE', #33642, .T. ) ;
#21207 = APPLIED_PERSON_AND_ORGANIZATION_ASSIGNMENT ( #38291, #3541, ( #39812 ) ) ;
#21208 = CARTESIAN_POINT ( 'NONE',  ( -0.08000000000000000167, -2.177105168660885326, -0.2518349584362399862 ) ) ;
#21209 = AXIS2_PLACEMENT_3D ( 'NONE', #28794, #6764, #19548 ) ;
#21210 = CARTESIAN_POINT ( 'NONE',  ( 0.7112185359115762440, -1.490287028582105711, 0.5669016283713388393 ) ) ;
#21212 = VERTEX_POINT ( 'NONE', #5046 ) ;
#21211 = VERTEX_POINT ( 'NONE', #1380 ) ;
#21213 = CARTESIAN_POINT ( 'NONE',  ( 0.3225054573102290600, -1.181499395378165174, 0.5729696959891698027 ) ) ;
#21214 = CARTESIAN_POINT ( 'NONE',  ( 0.1852697703518005889, -0.8388889655799410816, 0.1423358669777717023 ) ) ;
#21215 = CARTESIAN_POINT ( 'NONE',  ( 0.01548846960707528191, -0.09319974324248665731, 0.5318964258758798191 ) ) ;
#21216 = PRODUCT ( 'Pivot body rivet', 'Pivot body rivet', '', ( #27756 ) ) ;
#21217 = CARTESIAN_POINT ( 'NONE',  ( 0.4235708306963869574, -1.181282221097477381, 0.7940044402252741662 ) ) ;
#21218 = CARTESIAN_POINT ( 'NONE',  ( 0.1868970225581818301, -0.7280982606231287679, 0.03318949868953756377 ) ) ;
#21219 = VECTOR ( 'NONE', #28901, 39.37007874015748143 ) ;
#21220 = LINE ( 'NONE', #37043, #29713 ) ;
#21221 = CARTESIAN_POINT ( 'NONE',  ( 0.1399999999999994582, 0.000000000000000000, 0.000000000000000000 ) ) ;
#21222 = CARTESIAN_POINT ( 'NONE',  ( 0.3859792353386746755, -1.738628747592057211, -0.4467605215525291551 ) ) ;
#21223 = CARTESIAN_POINT ( 'NONE',  ( 0.4067032487861790280, -1.709706946175272080, 0.4220675772687526028 ) ) ;
#21224 = DIRECTION ( 'NONE',  ( 1.000000000000000000, 0.000000000000000000, 0.000000000000000000 ) ) ;
#21225 = CARTESIAN_POINT ( 'NONE',  ( -0.02000000000000000042, -2.253856486606507836, -0.7252438489935795207 ) ) ;
#21226 = CARTESIAN_POINT ( 'NONE',  ( 0.4802217237380822512, -1.662726879635128219, 0.3667417262808781442 ) ) ;
#21227 = EDGE_CURVE ( 'NONE', #21815, #21610, #16077, .T. ) ;
#21228 = CARTESIAN_POINT ( 'NONE',  ( 0.01127691157594227882, -0.9461533502836454446, 0.1506559775778698596 ) ) ;
#21229 = FACE_OUTER_BOUND ( 'NONE', #15264, .T. ) ;
#21230 = DIRECTION ( 'NONE',  ( 8.898377636568132790E-19, -0.1709855155552008066, 0.9852735424593119795 ) ) ;
#21231 = VECTOR ( 'NONE', #38026, 39.37007874015748143 ) ;
#21232 = CARTESIAN_POINT ( 'NONE',  ( 0.03170874437002593749, -0.2433708063334450444, 0.4274019033148761526 ) ) ;
#21233 = EDGE_CURVE ( 'NONE', #22334, #26563, #32460, .T. ) ;
#21234 = CARTESIAN_POINT ( 'NONE',  ( 0.2493678129588278725, -1.619726033520551667, 0.7664167198318853069 ) ) ;
#21235 = CARTESIAN_POINT ( 'NONE',  ( 0.06977928302938717076, -1.183750997490756296, 0.7568106749872303141 ) ) ;
#21236 = ADVANCED_FACE ( 'NONE', ( #32418 ), #973, .T. ) ;
#21237 = PERSON_AND_ORGANIZATION ( #28500, #32463 ) ;
#21238 = AXIS2_PLACEMENT_3D ( 'NONE', #15814, #38629, #28366 ) ;
#21239 = CARTESIAN_POINT ( 'NONE',  ( 0.2433107440384445208, -0.6632537007949954599, 0.5455544552538778014 ) ) ;
#21240 = AXIS2_PLACEMENT_3D ( 'NONE', #30139, #17777, #39797 ) ;
#21241 = AXIS2_PLACEMENT_3D ( 'NONE', #23066, #29015, #32905 ) ;
#21242 = EDGE_CURVE ( 'NONE', #23685, #24060, #26682, .T. ) ;
#21243 = CARTESIAN_POINT ( 'NONE',  ( 0.6964549535019117776, -1.533417755710658081, 0.5924443473190263987 ) ) ;
#21244 = EDGE_CURVE ( 'NONE', #1527, #17060, #6186, .T. ) ;
#21245 = CARTESIAN_POINT ( 'NONE',  ( 0.02953079040095500304, -0.09152108205201843483, -0.5223162075576466279 ) ) ;
#21246 = AXIS2_PLACEMENT_3D ( 'NONE', #2315, #5581, #24927 ) ;
#21247 =( GEOMETRIC_REPRESENTATION_CONTEXT ( 3 ) GLOBAL_UNCERTAINTY_ASSIGNED_CONTEXT ( ( #19042 ) ) GLOBAL_UNIT_ASSIGNED_CONTEXT ( ( #12411, #5214, #15298 ) ) REPRESENTATION_CONTEXT ( 'NONE', 'WORKASPACE' ) );
#21248 = CARTESIAN_POINT ( 'NONE',  ( 0.3494216204373458701, -1.697238143783349695, -0.4672182159968431558 ) ) ;
#21249 = ORIENTED_EDGE ( 'NONE', *, *, #19783, .F. ) ;
#21250 = LINE ( 'NONE', #18772, #15862 ) ;
#21251 = CARTESIAN_POINT ( 'NONE',  ( 0.09341372340922594886, -1.037589379625932784, 0.8542603175731292575 ) ) ;
#21252 = CARTESIAN_POINT ( 'NONE',  ( 0.1856961636715741826, -0.7498557161068394317, 0.5589214599598529842 ) ) ;
#21254 = ORIENTED_EDGE ( 'NONE', *, *, #32789, .F. ) ;
#21253 = LINE ( 'NONE', #33183, #21125 ) ;
#21255 = CARTESIAN_POINT ( 'NONE',  ( 0.1906247196645203257, -0.5843772811062373229, 0.1513679272151527977 ) ) ;
#21257 = ORIENTED_EDGE ( 'NONE', *, *, #27391, .T. ) ;
#21256 = ORIENTED_EDGE ( 'NONE', *, *, #25102, .T. ) ;
#21258 = CARTESIAN_POINT ( 'NONE',  ( 0.2927257310821322900, -0.8050081238773644232, 0.6220914005605751029 ) ) ;
#21259 = PLANE ( 'NONE',  #27654 ) ;
#21260 = ADVANCED_FACE ( 'NONE', ( #35924 ), #16997, .F. ) ;
#21261 = DIRECTION ( 'NONE',  ( 1.000000000000000000, 0.000000000000000000, 0.000000000000000000 ) ) ;
#21262 = APPROVAL_STATUS ( 'not_yet_approved' ) ;
#21263 = CIRCLE ( 'NONE', #3518, 0.1000000000000000194 ) ;
#21264 = CYLINDRICAL_SURFACE ( 'NONE', #25730, 2.001674066779348227 ) ;
#21265 = ORIENTED_EDGE ( 'NONE', *, *, #2167, .T. ) ;
#21266 = CARTESIAN_POINT ( 'NONE',  ( 0.1238647415275516556, -0.7604388772436289079, 0.4528127954481608319 ) ) ;
#21267 = AXIS2_PLACEMENT_3D ( 'NONE', #33068, #4874, #27112 ) ;
#21268 = CARTESIAN_POINT ( 'NONE',  ( 0.3239698234882238959, -1.727951091942375728, 0.7867494264257975933 ) ) ;
#21269 = CIRCLE ( 'NONE', #3524, 0.01500000000000001159 ) ;
#21270 = CARTESIAN_POINT ( 'NONE',  ( 0.09764433117057039202, -0.5450118788951329174, 0.1457185332388695742 ) ) ;
#21272 = CARTESIAN_POINT ( 'NONE',  ( 0.002290818369124609372, -0.5198888459286679087, 0.1457185332388686583 ) ) ;
#21271 = DIRECTION ( 'NONE',  ( 0.5154377295227949851, -0.8569270371416612964, 0.000000000000000000 ) ) ;
#21273 = CARTESIAN_POINT ( 'NONE',  ( 0.05908521160031481728, -1.327330609165742192, 0.5935265463149500542 ) ) ;
#21274 = VERTEX_POINT ( 'NONE', #29353 ) ;
#21275 = ORIENTED_EDGE ( 'NONE', *, *, #13039, .F. ) ;
#21276 = CARTESIAN_POINT ( 'NONE',  ( -0.1681560115201664318, 0.5223552577131993502, 0.1414989390318069917 ) ) ;
#21277 = CARTESIAN_POINT ( 'NONE',  ( 0.2762174934205044452, -0.8433163854438798790, 0.7765387688752221074 ) ) ;
#21278 = CIRCLE ( 'NONE', #29816, 1.986674066779348102 ) ;
#21279 = DIRECTION ( 'NONE',  ( 0.000000000000000000, -0.9901182710308658041, -0.1402348365095101024 ) ) ;
#21280 = VECTOR ( 'NONE', #40421, 39.37007874015748143 ) ;
#21281 = DIRECTION ( 'NONE',  ( 1.000000000000000000, 0.000000000000000000, 0.000000000000000000 ) ) ;
#21282 =( LENGTH_UNIT ( ) NAMED_UNIT ( * ) SI_UNIT ( $, .METRE. ) );
#21283 = CARTESIAN_POINT ( 'NONE',  ( 0.6624296566318823576, -1.373680494012689435, 0.6057417262805894209 ) ) ;
#21284 = CARTESIAN_POINT ( 'NONE',  ( 0.2711464003948310664, -1.672220156048179751, 0.5055462609045281441 ) ) ;
#21285 = CARTESIAN_POINT ( 'NONE',  ( 0.3122204723728539411, -1.175715471473605778, 0.5253545403616187714 ) ) ;
#21286 = CARTESIAN_POINT ( 'NONE',  ( 0.1874999999999996669, -0.6872203660140437931, 0.1457185332388695742 ) ) ;
#21287 = EDGE_CURVE ( 'NONE', #33645, #1152, #26590, .T. ) ;
#21288 = DATE_AND_TIME ( #12226, #14145 ) ;
#21289 = DIRECTION ( 'NONE',  ( -1.000000000000000000, -7.857794173099924470E-32, -8.628166150854818811E-32 ) ) ;
#21290 = CIRCLE ( 'NONE', #29830, 2.001671648589471442 ) ;
#21291 = ADVANCED_FACE ( 'NONE', ( #13890, #26464, #39000, #39216 ), #36925, .T. ) ;
#21292 = CARTESIAN_POINT ( 'NONE',  ( 0.4250902526234662804, -1.669131906446581270, -0.3966677131679292034 ) ) ;
#21293 = CARTESIAN_POINT ( 'NONE',  ( 0.4466550410545370164, -1.204244029663398496, 0.6473101387276720686 ) ) ;
#21294 = ADVANCED_FACE ( 'NONE', ( #8738 ), #29870, .T. ) ;
#21295 = DIRECTION ( 'NONE',  ( -8.881784197001246407E-16, 2.361472542561082612E-16, -1.000000000000000000 ) ) ;
#21296 = AXIS2_PLACEMENT_3D ( 'NONE', #24974, #34029, #11632 ) ;
#21297 = CIRCLE ( 'NONE', #34410, 1.986674066779348102 ) ;
#21298 = EDGE_LOOP ( 'NONE', ( #19633, #34955, #22179, #19475 ) ) ;
#21299 = DIRECTION ( 'NONE',  ( -0.9739500565613357086, -0.01953031614056561713, 0.2259200169874744923 ) ) ;
#21300 = CARTESIAN_POINT ( 'NONE',  ( -0.04308745346420909256, -0.2425953941929105406, 0.4306799763758633048 ) ) ;
#21301 = CARTESIAN_POINT ( 'NONE',  ( -0.3000000000000000999, -2.861028283584748699, -0.4103205306338890690 ) ) ;
#21302 = EDGE_LOOP ( 'NONE', ( #32308, #4389, #34662, #10941 ) ) ;
#21303 = CARTESIAN_POINT ( 'NONE',  ( -0.05078493045284435126, -0.04880252970039603705, -0.4712186791567240518 ) ) ;
#21304 = CIRCLE ( 'NONE', #25929, 0.1249999999999999584 ) ;
#21305 = CARTESIAN_POINT ( 'NONE',  ( 0.008503815048826473752, -0.8451467311994962373, 0.1457185332388719889 ) ) ;
#21307 = ORIENTED_EDGE ( 'NONE', *, *, #9958, .F. ) ;
#21306 = ORIENTED_EDGE ( 'NONE', *, *, #33369, .T. ) ;
#21308 = CARTESIAN_POINT ( 'NONE',  ( -2.106244131833921715E-14, -2.101105179789023669, -0.6980525405474647949 ) ) ;
#21309 = AXIS2_PLACEMENT_3D ( 'NONE', #35390, #25953, #3515 ) ;
#21310 = CARTESIAN_POINT ( 'NONE',  ( 0.05078310099560734425, -0.04880952477023445257, 0.4712228254505129721 ) ) ;
#21311 = EDGE_CURVE ( 'NONE', #12872, #22246, #17824, .T. ) ;
#21312 = CARTESIAN_POINT ( 'NONE',  ( 0.02242828275838676735, -0.4611032487610184916, -0.2233397882698420489 ) ) ;
#21313 = EDGE_CURVE ( 'NONE', #15916, #16708, #15114, .T. ) ;
#21314 = CARTESIAN_POINT ( 'NONE',  ( 0.1965730157716580884, -2.006121492102985293, -0.3172943880574278785 ) ) ;
#21315 = CARTESIAN_POINT ( 'NONE',  ( 0.4682349133427387566, -1.238864133684273394, 0.6416901653891257107 ) ) ;
#21317 = CARTESIAN_POINT ( 'NONE',  ( 0.1536596445529307131, -1.277574755431481579, 0.4245438548657216038 ) ) ;
#21316 = DIRECTION ( 'NONE',  ( 0.4999551463232373427, -0.8660512985181134660, 0.000000000000000000 ) ) ;
#21318 = CARTESIAN_POINT ( 'NONE',  ( 0.03174060074380018193, -0.3664546090234483966, -0.3753288017716262526 ) ) ;
#21319 = EDGE_LOOP ( 'NONE', ( #14873, #29633, #11744, #32248 ) ) ;
#21320 = EDGE_CURVE ( 'NONE', #22853, #9058, #21364, .T. ) ;
#21321 = ORIENTED_EDGE ( 'NONE', *, *, #38433, .F. ) ;
#21322 = DIRECTION ( 'NONE',  ( 0.000000000000000000, 0.5781348229923771731, -0.8159412518334715481 ) ) ;
#21323 = ORIENTED_EDGE ( 'NONE', *, *, #11148, .F. ) ;
#21324 = CARTESIAN_POINT ( 'NONE',  ( 0.000000000000000000, 0.6410130462957083219, -0.4300623794142590661 ) ) ;
#21325 = CARTESIAN_POINT ( 'NONE',  ( 0.4393559444842871642, -1.556801234278946122, 0.7099263403775109005 ) ) ;
#21327 = CARTESIAN_POINT ( 'NONE',  ( 0.5642073033013602634, -1.616444467847912847, 0.4682437291146816505 ) ) ;
#21326 = DIRECTION ( 'NONE',  ( 0.000000000000000000, 0.000000000000000000, 1.000000000000000000 ) ) ;
#21328 = CARTESIAN_POINT ( 'NONE',  ( 0.4497778021248119984, -1.147640960188543113, 0.4232850839822800415 ) ) ;
#21329 = ORIENTED_EDGE ( 'NONE', *, *, #8544, .T. ) ;
#21330 = CIRCLE ( 'NONE', #36432, 0.5088493849861029927 ) ;
#21331 = DIRECTION ( 'NONE',  ( 1.000000000000000000, 3.035386659626938621E-15, 7.588466649067346553E-16 ) ) ;
#21332 = CARTESIAN_POINT ( 'NONE',  ( 0.1990989110834594789, -2.031922935036753142, -0.2796108765274104013 ) ) ;
#21333 = AXIS2_PLACEMENT_3D ( 'NONE', #32649, #17017, #4453 ) ;
#21334 = CARTESIAN_POINT ( 'NONE',  ( 0.1367182587715192466, -0.6335969605309247354, 0.3882801499301780646 ) ) ;
#21335 = CARTESIAN_POINT ( 'NONE',  ( 0.4231979350574381904, -1.697322476885489762, 0.4297746138276614114 ) ) ;
#21336 = CARTESIAN_POINT ( 'NONE',  ( 0.4517177305807006937, -1.568671020668126914, 0.6057417262804751790 ) ) ;
#21337 = AXIS2_PLACEMENT_3D ( 'NONE', #17670, #36793, #15002 ) ;
#21338 = AXIS2_PLACEMENT_3D ( 'NONE', #11036, #4437, #1194 ) ;
#21339 = CARTESIAN_POINT ( 'NONE',  ( 0.3699999999999786793, -2.097675824466503691, -0.4688691127277797022 ) ) ;
#21340 = DIRECTION ( 'NONE',  ( 0.000000000000000000, -3.885780586188049371E-16, -1.000000000000000000 ) ) ;
#21341 = PLANE ( 'NONE',  #6224 ) ;
#21342 = CARTESIAN_POINT ( 'NONE',  ( -0.01548846960688975496, 0.09061086148592420453, -0.5171215251575761451 ) ) ;
#21343 = AXIS2_PLACEMENT_3D ( 'NONE', #16556, #965, #26044 ) ;
#21344 = CARTESIAN_POINT ( 'NONE',  ( 0.5633425123490871655, -1.213831759034801561, 0.8533915188341715252 ) ) ;
#21345 = AXIS2_PLACEMENT_3D ( 'NONE', #21645, #33979, #25127 ) ;
#21346 = CARTESIAN_POINT ( 'NONE',  ( -0.03174036153404255489, 0.2437184149031580704, 0.4645026301777952504 ) ) ;
#21347 = CARTESIAN_POINT ( 'NONE',  ( 0.4768848212686895849, -1.682051206446435243, -0.4156371400837835517 ) ) ;
#21348 = ADVANCED_FACE ( 'NONE', ( #30352 ), #27285, .T. ) ;
#21349 = CARTESIAN_POINT ( 'NONE',  ( 0.6598601525370707543, -1.502959539027199254, -0.4120828692936505666 ) ) ;
#21350 = FACE_OUTER_BOUND ( 'NONE', #29693, .T. ) ;
#21351 = CARTESIAN_POINT ( 'NONE',  ( 0.5913213363384987042, -1.604640830199632662, 0.6017661975466599422 ) ) ;
#21352 = DIRECTION ( 'NONE',  ( 0.2067069058495553946, 0.1193280138680803265, 0.9710989033977963647 ) ) ;
#21353 = DIRECTION ( 'NONE',  ( 0.000000000000000000, 5.978086547377981840E-31, 1.000000000000000000 ) ) ;
#21354 = EDGE_LOOP ( 'NONE', ( #25509, #4633, #4073, #12349 ) ) ;
#21355 = CARTESIAN_POINT ( 'NONE',  ( -0.2399999999999999079, -1.835749455202394298, -0.3938319975228649072 ) ) ;
#21356 = CARTESIAN_POINT ( 'NONE',  ( 0.3992403239432279483, -1.683235622436119128, -0.6263438071736162627 ) ) ;
#21357 = VECTOR ( 'NONE', #5052, 39.37007874015748143 ) ;
#21358 = DIRECTION ( 'NONE',  ( 1.000000000000000000, -0.000000000000000000, -0.000000000000000000 ) ) ;
#21359 = FACE_OUTER_BOUND ( 'NONE', #32421, .T. ) ;
#21360 = CIRCLE ( 'NONE', #18739, 0.03000000000000006481 ) ;
#21361 = VECTOR ( 'NONE', #29525, 39.37007874015748854 ) ;
#21362 = ORIENTED_EDGE ( 'NONE', *, *, #39400, .F. ) ;
#21363 = CARTESIAN_POINT ( 'NONE',  ( 0.4714772250923787711, -1.069474201788713108, -0.6070170271373026560 ) ) ;
#21364 = CIRCLE ( 'NONE', #28578, 0.2000000000000000666 ) ;
#21365 = CARTESIAN_POINT ( 'NONE',  ( 0.3398061633079089705, -1.151650735656065461, 0.5895292019541952255 ) ) ;
#21366 = APPROVAL_PERSON_ORGANIZATION ( #7137, #11684, #20129 ) ;
#21367 = LINE ( 'NONE', #30609, #8584 ) ;
#21368 = ADVANCED_FACE ( 'NONE', ( #34043 ), #15858, .T. ) ;
#21369 = CARTESIAN_POINT ( 'NONE',  ( 0.03170874437003164126, 0.2433708063334497629, -0.4274019033148664937 ) ) ;
#21370 = CARTESIAN_POINT ( 'NONE',  ( 0.5004679210847464699, -1.293934441700709037, 0.6841144912013866763 ) ) ;
#21371 = APPLIED_PERSON_AND_ORGANIZATION_ASSIGNMENT ( #2293, #30674, ( #20163 ) ) ;
#21373 = ORIENTED_EDGE ( 'NONE', *, *, #2043, .F. ) ;
#21372 = CARTESIAN_POINT ( 'NONE',  ( -0.1707856549140114588, 0.4978063840003627005, 0.1437995925080555182 ) ) ;
#21374 = CARTESIAN_POINT ( 'NONE',  ( 0.3074110389119673048, -0.9534851582863556052, 0.5796648297427198226 ) ) ;
#21375 = ORIENTED_EDGE ( 'NONE', *, *, #30362, .F. ) ;
#21376 = EDGE_CURVE ( 'NONE', #23612, #17567, #23297, .T. ) ;
#21377 = APPROVAL_STATUS ( 'not_yet_approved' ) ;
#21378 = CIRCLE ( 'NONE', #3615, 0.03749999999977554621 ) ;
#21379 = LINE ( 'NONE', #14980, #4660 ) ;
#21380 = EDGE_LOOP ( 'NONE', ( #8619, #18272, #34967, #3288 ) ) ;
#21381 = CARTESIAN_POINT ( 'NONE',  ( -0.02231181081520755560, 0.3551561381230132208, -0.3696296485972541124 ) ) ;
#21382 = CARTESIAN_POINT ( 'NONE',  ( 0.03580802019661705193, -0.5461554526729558434, 0.2169286433324936203 ) ) ;
#21384 = CARTESIAN_POINT ( 'NONE',  ( 0.1759602538404660133, -0.6574070655985931877, -0.08278933279227815301 ) ) ;
#21383 = CARTESIAN_POINT ( 'NONE',  ( -0.1743922129835733803, -0.5166151207188712791, 0.3749999999999999445 ) ) ;
#21385 = CARTESIAN_POINT ( 'NONE',  ( 0.000000000000000000, 0.000000000000000000, 0.000000000000000000 ) ) ;
#21386 = ORIENTED_EDGE ( 'NONE', *, *, #8646, .T. ) ;
#21387 = ORIENTED_EDGE ( 'NONE', *, *, #28767, .T. ) ;
#21388 = CARTESIAN_POINT ( 'NONE',  ( 0.5327020933798468638, -1.151343754938154218, 0.6263913407894506902 ) ) ;
#21389 = CARTESIAN_POINT ( 'NONE',  ( 0.1463340742998959498, -0.7013816541812762928, 0.5029480910574282149 ) ) ;
#21390 = ORIENTED_EDGE ( 'NONE', *, *, #33893, .F. ) ;
#21391 = CARTESIAN_POINT ( 'NONE',  ( 0.1348608168514592864, -1.985670591994486367, -0.3242396390482729096 ) ) ;
#21392 = LINE ( 'NONE', #27140, #40062 ) ;
#21393 = CARTESIAN_POINT ( 'NONE',  ( -1.920933771635442211, -2.937918075995054945, 0.4182417262808775238 ) ) ;
#21394 = VECTOR ( 'NONE', #38744, 39.37007874015748143 ) ;
#21395 = CARTESIAN_POINT ( 'NONE',  ( -0.1123064544305657775, -0.5135141720357971895, 0.3236707397771451666 ) ) ;
#21396 = B_SPLINE_CURVE_WITH_KNOTS ( 'NONE', 3,
 ( #28372, #40513, #31659, #9652, #37619, #15626, #31868, #12528 ),
 .UNSPECIFIED., .F., .F.,
 ( 4, 2, 2, 4 ),
 ( 1.602656041417568188E-11, 0.001966995538234637009, 0.002950493299338675587, 0.003933991060442713732 ),
 .UNSPECIFIED. ) ;
#21397 = DIRECTION ( 'NONE',  ( -0.9998941303973200023, 0.01455087615875037474, 0.000000000000000000 ) ) ;
#21398 = CARTESIAN_POINT ( 'NONE',  ( 0.3922353094782703997, -1.714330012172307294, 0.4177417262808784115 ) ) ;
#21399 = CARTESIAN_POINT ( 'NONE',  ( 0.3518999744609554448, -1.164331320867108444, 0.4249471546789464482 ) ) ;
#21400 = CARTESIAN_POINT ( 'NONE',  ( 0.1601079512667811788, -1.855210257011521202, -0.6514173194225818531 ) ) ;
#21401 = CARTESIAN_POINT ( 'NONE',  ( 0.003421962176364201202, -0.9701471101739370662, 0.4009549150280219965 ) ) ;
#21402 = PERSON_AND_ORGANIZATION ( #28500, #32463 ) ;
#21403 = APPROVAL_PERSON_ORGANIZATION ( #35853, #2114, #36242 ) ;
#21404 = EDGE_CURVE ( 'NONE', #21164, #35448, #25954, .T. ) ;
#21405 = B_SPLINE_CURVE_WITH_KNOTS ( 'NONE', 3,
 ( #12442, #5664, #8958, #15548, #37526, #3190, #21531, #18410, #27893, #12050 ),
 .UNSPECIFIED., .F., .F.,
 ( 4, 2, 2, 2, 4 ),
 ( 0.000000000000000000, 0.0005029730322535831428, 0.001005946064507166286, 0.001508919096760749428, 0.002011892129014332571 ),
 .UNSPECIFIED. ) ;
#21406 = CARTESIAN_POINT ( 'NONE',  ( 0.4823781031358342353, -1.129173803219876149, 0.4907471721780757856 ) ) ;
#21407 = CARTESIAN_POINT ( 'NONE',  ( 0.4639634386416064404, -1.238283699618621725, 0.6057417262809811076 ) ) ;
#21408 = VECTOR ( 'NONE', #28410, 39.37007874015748143 ) ;
#21409 = DIRECTION ( 'NONE',  ( -1.664003471950577032E-31, -3.330669073875470607E-16, -1.000000000000000000 ) ) ;
#21410 =( BOUNDED_SURFACE ( )  B_SPLINE_SURFACE ( 3, 2, ( 
 ( #2428, #30997, #14965 ),
 ( #11865, #24433, #15370 ),
 ( #36965, #8784, #37179 ),
 ( #8996, #31219, #21561 ),
 ( #40467, #21750, #34080 ),
 ( #24849, #5885, #18445 ) ),
 .UNSPECIFIED., .F., .F., .F. ) 
 B_SPLINE_SURFACE_WITH_KNOTS ( ( 4, 2, 4 ),
 ( 3, 3 ),
 ( -2.168404344971008868E-19, 0.001064962965551008965, 0.002129925931102017930 ),
 ( 0.000000000000000000, 1.000000000000000000 ),
 .UNSPECIFIED. ) 
 GEOMETRIC_REPRESENTATION_ITEM ( )  RATIONAL_B_SPLINE_SURFACE ( (
 ( 1.000000000000000000, 0.8067368806807361237, 1.000000000000000000),
 ( 1.000000000000000000, 0.8240497396349234505, 1.000000000000000000),
 ( 1.000000000000000000, 0.8393628034582739650, 1.000000000000000000),
 ( 1.000000000000000000, 0.8610007399255795724, 1.000000000000000000),
 ( 1.000000000000000000, 0.8667168599303205490, 1.000000000000000000),
 ( 1.000000000000000000, 0.8659230874819840995, 1.000000000000000000) ) ) 
 REPRESENTATION_ITEM ( '' )  SURFACE ( )  );
#21411 = CARTESIAN_POINT ( 'NONE',  ( 3.839896904129604577E-06, -0.6023364376982222046, -0.1016634491690118630 ) ) ;
#21412 = DIRECTION ( 'NONE',  ( 0.000000000000000000, 0.000000000000000000, -1.000000000000000000 ) ) ;
#21413 = CARTESIAN_POINT ( 'NONE',  ( 0.4634865284762403892, -1.134362257022321518, -0.3648515278348755109 ) ) ;
#21414 = DIRECTION ( 'NONE',  ( 1.000000000000000000, 0.000000000000000000, 0.000000000000000000 ) ) ;
#21415 = B_SPLINE_CURVE_WITH_KNOTS ( 'NONE', 3,
 ( #15445, #27997, #24717, #9464, #37247, #6169, #12548, #6376 ),
 .UNSPECIFIED., .F., .F.,
 ( 4, 2, 2, 4 ),
 ( 0.000000000000000000, 0.0001840052804137891915, 0.0003680105608275783830, 0.0007360211216551754143 ),
 .UNSPECIFIED. ) ;
#21416 = EDGE_LOOP ( 'NONE', ( #13703, #28095, #14128, #15669 ) ) ;
#21417 = ORIENTED_EDGE ( 'NONE', *, *, #14000, .F. ) ;
#21418 = CARTESIAN_POINT ( 'NONE',  ( 0.03113248654051816583, 0.000000000000000000, 0.000000000000000000 ) ) ;
#21419 = ORIENTED_EDGE ( 'NONE', *, *, #25626, .T. ) ;
#21420 = CARTESIAN_POINT ( 'NONE',  ( 0.3222810527215910215, -1.758570551863011922, 0.4849083929475443422 ) ) ;
#21421 = CARTESIAN_POINT ( 'NONE',  ( -0.1123123235486658822, -0.5135423695149525791, 0.1325268268875365030 ) ) ;
#21423 = ORIENTED_EDGE ( 'NONE', *, *, #36612, .F. ) ;
#21422 = LINE ( 'NONE', #31062, #18644 ) ;
#21424 = AXIS2_PLACEMENT_3D ( 'NONE', #40051, #24443, #9398 ) ;
#21425 = CIRCLE ( 'NONE', #6294, 0.08000000000000002942 ) ;
#21426 = ORIENTED_EDGE ( 'NONE', *, *, #21604, .F. ) ;
#21427 = DIRECTION ( 'NONE',  ( -1.000000000000000000, -7.857794173099924470E-32, -8.628166150854818811E-32 ) ) ;
#21428 = ORIENTED_EDGE ( 'NONE', *, *, #27040, .F. ) ;
#21429 = CARTESIAN_POINT ( 'NONE',  ( 0.2665270026871217612, -1.675380026011078716, 0.5755890425476034578 ) ) ;
#21431 = CARTESIAN_POINT ( 'NONE',  ( -0.03158843595483366157, -0.4482533282649006634, 0.2030547983902455944 ) ) ;
#21430 = CARTESIAN_POINT ( 'NONE',  ( 0.1972680329291656987, -0.9306160649008226038, 0.6420804189482948177 ) ) ;
#21432 = LOCAL_TIME ( 0, 53, 7.000000000000000000, #35206 ) ;
#21433 = CARTESIAN_POINT ( 'NONE',  ( 0.6065454785784598624, -1.479009159021363207, 0.5747789317403434461 ) ) ;
#21434 = ITEM_DEFINED_TRANSFORMATION ( 'NONE', 'NONE', #2271,  #27819 ) ;
#21435 = EDGE_CURVE ( 'NONE', #1535, #14410, #2938, .T. ) ;
#21436 = CARTESIAN_POINT ( 'NONE',  ( -0.1339136704200478145, -0.4685718226220191851, 0.09550516381870249871 ) ) ;
#21438 = EDGE_LOOP ( 'NONE', ( #3746, #10617, #31566, #37798 ) ) ;
#21437 = ORIENTED_EDGE ( 'NONE', *, *, #11506, .T. ) ;
#21439 = CARTESIAN_POINT ( 'NONE',  ( 0.01142787841204725117, -0.9119713417645858300, 0.01598648563123014274 ) ) ;
#21440 = AXIS2_PLACEMENT_3D ( 'NONE', #1355, #38976, #17382 ) ;
#21441 = FACE_OUTER_BOUND ( 'NONE', #24914, .T. ) ;
#21442 = CARTESIAN_POINT ( 'NONE',  ( -0.05187277790672265715, -0.4419080096627363563, 0.1624279055868609323 ) ) ;
#21443 = CARTESIAN_POINT ( 'NONE',  ( 0.4624398381476410025, -1.269083403305113489, 0.8176449397995606549 ) ) ;
#21444 = CARTESIAN_POINT ( 'NONE',  ( -0.2399999999999999079, -2.183180860297908144, -0.4937760292030871079 ) ) ;
#21445 = CARTESIAN_POINT ( 'NONE',  ( 0.2599034962623482659, -1.582350648323867182, 0.8549863447754705303 ) ) ;
#21446 = CARTESIAN_POINT ( 'NONE',  ( 0.01240358949466654342, -0.4404738072168086216, 0.2329760197377778452 ) ) ;
#21447 = CARTESIAN_POINT ( 'NONE',  ( 0.4196259286637142871, -1.711435686544057644, 0.4273953198980491863 ) ) ;
#21448 = CARTESIAN_POINT ( 'NONE',  ( 0.3782034578509241851, -1.662383355070864654, -0.6252036213791186681 ) ) ;
#21449 = DIRECTION ( 'NONE',  ( 1.188678714063518227E-15, -1.000000000000000000, -3.263080277421930985E-16 ) ) ;
#21450 = CARTESIAN_POINT ( 'NONE',  ( 0.4676789493019616883, -1.559177855287317005, 0.5735223705611400824 ) ) ;
#21451 = CARTESIAN_POINT ( 'NONE',  ( -0.0003736070913198792057, -0.9292939094275918244, 0.08502934550331207875 ) ) ;
#21452 = DIRECTION ( 'NONE',  ( 0.000000000000000000, 0.000000000000000000, 1.000000000000000000 ) ) ;
#21453 = AXIS2_PLACEMENT_3D ( 'NONE', #18278, #33921, #12313 ) ;
#21454 = CARTESIAN_POINT ( 'NONE',  ( 0.1784968570797965948, -1.218054820023663831, -0.5155029497116575543 ) ) ;
#21455 = CARTESIAN_POINT ( 'NONE',  ( 0.2426062050407847281, -1.584949062848913348, 0.8214247301831154591 ) ) ;
#21456 = CARTESIAN_POINT ( 'NONE',  ( 0.04678374077078594623, -1.010183413244198469, 0.6999868061010977582 ) ) ;
#21457 = DATE_AND_TIME ( #8881, #3675 ) ;
#21458 = CARTESIAN_POINT ( 'NONE',  ( 0.4805300281521128203, -1.080349003257709439, 0.8405881438443104647 ) ) ;
#21459 = ORIENTED_EDGE ( 'NONE', *, *, #18593, .F. ) ;
#21460 = CARTESIAN_POINT ( 'NONE',  ( 0.7071864311907015699, -1.521274929146462673, 0.5612556364004261944 ) ) ;
#21461 = CARTESIAN_POINT ( 'NONE',  ( 0.04157143636675288134, -0.01703379379374815594, -0.4699528923077430087 ) ) ;
#21462 = CARTESIAN_POINT ( 'NONE',  ( 0.3437180095255871204, -1.654344192420559967, -0.4444229222738684815 ) ) ;
#21463 = ORIENTED_EDGE ( 'NONE', *, *, #25749, .F. ) ;
#21464 = CARTESIAN_POINT ( 'NONE',  ( -0.002282498291095993656, -0.8555267327002353817, 0.1457185332388701293 ) ) ;
#21465 = CARTESIAN_POINT ( 'NONE',  ( 0.2722157990050696474, -1.638612347704280658, 0.7745732599775748684 ) ) ;
#21466 = CARTESIAN_POINT ( 'NONE',  ( 0.1282641000242639162, -0.5556219276664670081, 0.1881736293549454153 ) ) ;
#21468 = EDGE_LOOP ( 'NONE', ( #34519, #14466, #39999, #1683 ) ) ;
#21467 = DIRECTION ( 'NONE',  ( -0.4999551463232372317, 0.8660512985181134660, -0.000000000000000000 ) ) ;
#21469 = CARTESIAN_POINT ( 'NONE',  ( 0.5847200959167868639, -1.241056950120674518, 0.7055318339491533086 ) ) ;
#21471 = EDGE_LOOP ( 'NONE', ( #13506, #12549, #9010, #37693, #15387, #32079, #14443, #20812, #29363 ) ) ;
#21470 = ORIENTED_EDGE ( 'NONE', *, *, #22995, .T. ) ;
#21472 = DIRECTION ( 'NONE',  ( -0.4999551463232373427, 0.8660512985181134660, -0.000000000000000000 ) ) ;
#21473 = DIRECTION ( 'NONE',  ( 1.000000000000000000, 0.000000000000000000, 0.000000000000000000 ) ) ;
#21474 = DIRECTION ( 'NONE',  ( 0.000000000000000000, 0.000000000000000000, -1.000000000000000000 ) ) ;
#21475 = CALENDAR_DATE ( 2026, 13, 10 ) ;
#21476 = SPHERICAL_SURFACE ( 'NONE', #11271, 0.01499999999999999944 ) ;
#21477 = ORIENTED_EDGE ( 'NONE', *, *, #12935, .F. ) ;
#21478 = TOROIDAL_SURFACE ( 'NONE', #26091, 0.04749999999977554815, 0.01000000000000000021 ) ;
#21479 = ADVANCED_FACE ( 'NONE', ( #29646 ), #12435, .F. ) ;
#21480 = ADVANCED_FACE ( 'NONE', ( #6264 ), #13445, .T. ) ;
#21481 = CARTESIAN_POINT ( 'NONE',  ( 0.09608046277552639847, -0.7200274365782738384, 0.3052469828618230019 ) ) ;
#21482 = EDGE_CURVE ( 'NONE', #18572, #2349, #22138, .T. ) ;
#21483 = CARTESIAN_POINT ( 'NONE',  ( 0.1909286924077255032, -1.257064795538239022, -0.7462941026102624109 ) ) ;
#21484 = CARTESIAN_POINT ( 'NONE',  ( 0.5236732281772086273, -1.517283060796150718, 0.6742510201405766956 ) ) ;
#21486 = CARTESIAN_POINT ( 'NONE',  ( -0.002282498291095993656, -0.8555267327002353817, 0.1457185332388701293 ) ) ;
#21485 = CARTESIAN_POINT ( 'NONE',  ( 0.3251375141011914049, -1.768545959953308877, 0.5240463964343101688 ) ) ;
#21487 = CARTESIAN_POINT ( 'NONE',  ( 0.0003805203522013556679, -0.9506305917533103278, 0.2426406003428543956 ) ) ;
#21488 = APPLIED_SECURITY_CLASSIFICATION_ASSIGNMENT ( #3089, ( #40659 ) ) ;
#21489 = VERTEX_POINT ( 'NONE', #35056 ) ;
#21490 = ADVANCED_FACE ( 'NONE', ( #3374 ), #36871, .T. ) ;
#21491 = DIRECTION ( 'NONE',  ( 0.9823333030490233320, -0.1871397384865000069, -5.691349986800536046E-16 ) ) ;
#21492 = CARTESIAN_POINT ( 'NONE',  ( 0.5838512187896826022, -1.247881422114380801, 0.8761440252600439793 ) ) ;
#21493 = EDGE_CURVE ( 'NONE', #4130, #9666, #36440, .T. ) ;
#21494 = AXIS2_PLACEMENT_3D ( 'NONE', #21832, #33968, #5771 ) ;
#21495 = DIRECTION ( 'NONE',  ( -1.000000000000000000, 0.000000000000000000, 0.000000000000000000 ) ) ;
#21496 = DIRECTION ( 'NONE',  ( -8.881784197001245421E-16, 2.361472542561082612E-16, -1.000000000000000000 ) ) ;
#21497 = B_SPLINE_CURVE_WITH_KNOTS ( 'NONE', 3,
 ( #31337, #37281, #36874, #5803 ),
 .UNSPECIFIED., .F., .F.,
 ( 4, 4 ),
 ( -1.150894640811756038E-05, 0.0005747792170237749076 ),
 .UNSPECIFIED. ) ;
#21498 = FACE_OUTER_BOUND ( 'NONE', #36542, .T. ) ;
#21499 = CARTESIAN_POINT ( 'NONE',  ( 0.2607589496226037640, -1.678824709164980833, 0.5052740673131734805 ) ) ;
#21500 = CARTESIAN_POINT ( 'NONE',  ( 0.3554163599750466140, -1.162345695606875173, 0.4422132562362467434 ) ) ;
#21501 = CARTESIAN_POINT ( 'NONE',  ( 0.4873263706924592098, -1.095012774062378513, 0.6880473194844076712 ) ) ;
#21502 = PERSON_AND_ORGANIZATION_ROLE ( 'creator' ) ;
#21503 = CARTESIAN_POINT ( 'NONE',  ( 0.5654596793231598806, -1.618818539163461301, 0.5682417262808788783 ) ) ;
#21504 = EDGE_CURVE ( 'NONE', #18975, #34456, #7531, .T. ) ;
#21505 = APPLIED_DATE_AND_TIME_ASSIGNMENT ( #32153, #16329, ( #2626 ) ) ;
#21506 = AXIS2_PLACEMENT_3D ( 'NONE', #22463, #7012, #34782 ) ;
#21507 = CARTESIAN_POINT ( 'NONE',  ( 0.1804782205544497031, -1.898145329168058781, -0.6575140397730463437 ) ) ;
#21508 = CARTESIAN_POINT ( 'NONE',  ( 0.6078349182483022695, -1.478587231578513572, 0.5349676189723107100 ) ) ;
#21509 = DIRECTION ( 'NONE',  ( 1.000000000000000000, 1.441651681710401470E-15, -8.132394101956109642E-16 ) ) ;
#21510 = APPLIED_APPROVAL_ASSIGNMENT ( #38939, ( #12929 ) ) ;
#21511 = ORIENTED_EDGE ( 'NONE', *, *, #37564, .F. ) ;
#21512 = CARTESIAN_POINT ( 'NONE',  ( -0.1210963378865892032, -0.5065302875297106322, 0.3108129518247104150 ) ) ;
#21513 = DIRECTION ( 'NONE',  ( 0.000000000000000000, 0.000000000000000000, 1.000000000000000000 ) ) ;
#21514 = CARTESIAN_POINT ( 'NONE',  ( -0.01548846960707517956, -0.3772621329472692908, -0.3651003739303438911 ) ) ;
#21515 = EDGE_LOOP ( 'NONE', ( #32077, #18723, #39967, #4405, #19032 ) ) ;
#21516 = CARTESIAN_POINT ( 'NONE',  ( -0.04211471441534185567, 0.008601378579329254509, -0.4689528935642813257 ) ) ;
#21517 = CARTESIAN_POINT ( 'NONE',  ( 0.01144005434401617304, -0.8535789549361010309, 0.3246971777977655793 ) ) ;
#21519 = EDGE_LOOP ( 'NONE', ( #23167, #6522, #6401, #22767 ) ) ;
#21518 = ORIENTED_EDGE ( 'NONE', *, *, #14433, .T. ) ;
#21520 = CARTESIAN_POINT ( 'NONE',  ( 0.3047936848243344432, -1.756875962071034580, 0.5682417262361116883 ) ) ;
#21521 = CARTESIAN_POINT ( 'NONE',  ( 0.04308611741967044440, -0.05688666786373557105, 0.4910246251072628021 ) ) ;
#21522 = CARTESIAN_POINT ( 'NONE',  ( 0.7390121836339409445, -1.515703229308124955, 0.4860421661703527851 ) ) ;
#21523 = CARTESIAN_POINT ( 'NONE',  ( 0.3758909033093429386, -1.726409976104785526, -0.3411215252611376481 ) ) ;
#21524 = CARTESIAN_POINT ( 'NONE',  ( 0.3416500515225935897, -1.080402072964486315, 0.7068558125486118504 ) ) ;
#21525 = CARTESIAN_POINT ( 'NONE',  ( 0.1957946853229683704, -1.369086038819396389, 0.5557458681356171049 ) ) ;
#21526 = FACE_OUTER_BOUND ( 'NONE', #29842, .T. ) ;
#21527 = ORIENTED_EDGE ( 'NONE', *, *, #32105, .F. ) ;
#21528 = CARTESIAN_POINT ( 'NONE',  ( 0.1482405220709307747, -0.7090401843242698510, 0.5530575512909489122 ) ) ;
#21529 = ORIENTED_EDGE ( 'NONE', *, *, #25390, .T. ) ;
#21530 = EDGE_CURVE ( 'NONE', #13465, #17453, #5567, .T. ) ;
#21531 = CARTESIAN_POINT ( 'NONE',  ( 0.6990116478510675080, -1.529268566928075002, 0.5876553814873258785 ) ) ;
#21532 = CARTESIAN_POINT ( 'NONE',  ( 0.06090235255802147613, -0.5536121331843190108, 0.2259376826350176226 ) ) ;
#21534 = CARTESIAN_POINT ( 'NONE',  ( 0.5538295395026971990, -1.622802647202313819, 0.5051661404396670108 ) ) ;
#21533 = LINE ( 'NONE', #30965, #3337 ) ;
#21535 = DIRECTION ( 'NONE',  ( 5.551115123125663140E-17, 3.263080277421932464E-16, -1.000000000000000000 ) ) ;
#21536 = CARTESIAN_POINT ( 'NONE',  ( 0.3699999999999783462, -2.097675824466504135, -0.5196396315034577107 ) ) ;
#21537 = ORIENTED_EDGE ( 'NONE', *, *, #4170, .T. ) ;
#21538 = ADVANCED_FACE ( 'NONE', ( #21205 ), #10841, .F. ) ;
#21539 = CARTESIAN_POINT ( 'NONE',  ( 0.5053588047760252389, -1.583603243833816565, -0.5401600205605632254 ) ) ;
#21540 = CARTESIAN_POINT ( 'NONE',  ( 0.3942985600065282425, -1.769819547351404454, -0.5278219303748407087 ) ) ;
#21541 = ADVANCED_FACE ( 'NONE', ( #14403 ), #12806, .F. ) ;
#21542 = CARTESIAN_POINT ( 'NONE',  ( 0.1221917373669615114, -0.5546197540517507907, 0.1887439894328808709 ) ) ;
#21543 = CARTESIAN_POINT ( 'NONE',  ( 0.4503526376543276477, -1.692732021471400339, 0.4426110423297867635 ) ) ;
#21544 = DIRECTION ( 'NONE',  ( -0.8660512985181135770, -0.4999551463232371207, 0.000000000000000000 ) ) ;
#21545 = CARTESIAN_POINT ( 'NONE',  ( -0.03868264068766689295, 0.4417248602032612936, 0.1788646266443642829 ) ) ;
#21546 = PLANE ( 'NONE',  #8870 ) ;
#21547 = CARTESIAN_POINT ( 'NONE',  ( 0.3663975874019590462, -1.157438136726378408, 0.4269148889825721827 ) ) ;
#21548 = CARTESIAN_POINT ( 'NONE',  ( 0.3446155261768803491, -0.8529094429884808148, 0.7348996499020890028 ) ) ;
#21549 = CARTESIAN_POINT ( 'NONE',  ( -0.04760454375021182932, 0.2475296122118653130, 0.4138634427292582352 ) ) ;
#21550 = EDGE_CURVE ( 'NONE', #13008, #36014, #40425, .T. ) ;
#21551 = CARTESIAN_POINT ( 'NONE',  ( 0.001320963519262947179, -0.9568487245275125730, 0.3190620996948075327 ) ) ;
#21552 = CARTESIAN_POINT ( 'NONE',  ( 0.6469206375993061808, -1.465334083252977093, -0.4112288931193002761 ) ) ;
#21553 = DIRECTION ( 'NONE',  ( 0.000000000000000000, 3.330669073875470114E-16, 1.000000000000000000 ) ) ;
#21554 = CARTESIAN_POINT ( 'NONE',  ( 0.1212526918783438795, -0.8711807980328569734, 0.4983147516987611048 ) ) ;
#21555 = CARTESIAN_POINT ( 'NONE',  ( 0.2672157584620782345, -1.674897712893493429, 0.5728500076325480084 ) ) ;
#21556 = CARTESIAN_POINT ( 'NONE',  ( -0.2746410161513779258, -2.377368549242099949, -0.4802393080720198104 ) ) ;
#21557 = ORIENTED_EDGE ( 'NONE', *, *, #28824, .T. ) ;
#21558 = DIRECTION ( 'NONE',  ( 0.000000000000000000, -0.7071067811865484609, 0.7071067811865465735 ) ) ;
#21559 = CARTESIAN_POINT ( 'NONE',  ( 0.3975019948776055134, -1.696135473892855572, -0.6064691975985911920 ) ) ;
#21560 = CARTESIAN_POINT ( 'NONE',  ( 0.3623221021055049729, -1.968029003640406449, -0.5215600955572180508 ) ) ;
#21561 = CARTESIAN_POINT ( 'NONE',  ( 0.4356923561510381848, -1.693540257987297792, -0.6182874616928464295 ) ) ;
#21562 = ORIENTED_EDGE ( 'NONE', *, *, #2145, .F. ) ;
#21563 = CARTESIAN_POINT ( 'NONE',  ( 0.5378106547832601780, -1.668789341594314024, -0.5701368517888846243 ) ) ;
#21564 = CARTESIAN_POINT ( 'NONE',  ( 0.3295209608565876636, -1.174482601001649362, 0.5872793224613557239 ) ) ;
#21565 = DIRECTION ( 'NONE',  ( -8.881784197001246407E-16, 2.361472542561082612E-16, -1.000000000000000000 ) ) ;
#21566 = CARTESIAN_POINT ( 'NONE',  ( 0.01548846960706656492, 0.3688619771573081185, -0.3775276577327085215 ) ) ;
#21567 = CARTESIAN_POINT ( 'NONE',  ( 0.4621666676022437859, -1.234211826098466913, 0.7071490788379034553 ) ) ;
#21569 = EDGE_LOOP ( 'NONE', ( #37565, #19126, #27137, #3059 ) ) ;
#21568 = LINE ( 'NONE', #30612, #35732 ) ;
#21570 = CARTESIAN_POINT ( 'NONE',  ( 0.4515156439561487933, -1.057718100141998407, 0.6525781907329395448 ) ) ;
#21571 = VERTEX_POINT ( 'NONE', #24296 ) ;
#21572 = APPROVAL_ROLE ( '' ) ;
#21573 = AXIS2_PLACEMENT_3D ( 'NONE', #22339, #6470, #6875 ) ;
#21574 = CARTESIAN_POINT ( 'NONE',  ( 0.1999999999999789724, -2.183180860297921466, -0.7437760292030870524 ) ) ;
#21575 = ORIENTED_EDGE ( 'NONE', *, *, #1678, .T. ) ;
#21576 = EDGE_CURVE ( 'NONE', #5500, #17083, #34525, .T. ) ;
#21577 = EDGE_LOOP ( 'NONE', ( #1068, #36356, #23448, #12670 ) ) ;
#21578 = CARTESIAN_POINT ( 'NONE',  ( 0.03743733038894521414, -0.5670480389072934946, 0.2780609670579947124 ) ) ;
#21580 = CARTESIAN_POINT ( 'NONE',  ( 0.1861909972232556609, -0.6993559402776449163, -0.02127579158555052696 ) ) ;
#21579 = CARTESIAN_POINT ( 'NONE',  ( 0.06558781334581398337, -0.7848964240899376499, 0.03428501785215255782 ) ) ;
#21581 = CARTESIAN_POINT ( 'NONE',  ( 0.4634712904840411762, -1.711704060178987241, -0.5155029497116575543 ) ) ;
#21582 = ADVANCED_FACE ( 'NONE', ( #33742 ), #18117, .T. ) ;
#21583 = EDGE_LOOP ( 'NONE', ( #2333, #19436 ) ) ;
#21584 = CARTESIAN_POINT ( 'NONE',  ( 0.3036438813139882842, -1.041601470818427799, 0.6258450271758987382 ) ) ;
#21585 = CARTESIAN_POINT ( 'NONE',  ( 0.5469705670084967775, -1.495816971338993495, 0.6906149559573403485 ) ) ;
#21586 = ORIENTED_EDGE ( 'NONE', *, *, #26761, .T. ) ;
#21587 = CARTESIAN_POINT ( 'NONE',  ( 0.1357105165892661391, -2.051761019322187796, -0.3074898295655506542 ) ) ;
#21588 = DIRECTION ( 'NONE',  ( 0.8660254037844395958, 0.2890674114961868102, -0.4079706259167349969 ) ) ;
#21589 = CARTESIAN_POINT ( 'NONE',  ( 0.01393220626005791697, -1.691440753321579615, -0.3707258672847664194 ) ) ;
#21590 = CARTESIAN_POINT ( 'NONE',  ( -0.1112012347075381491, -0.5082045352551866069, 0.3316257441459560806 ) ) ;
#21591 = PERSON ( 'NAUO-PER10', 'UNSPECIFIED', 'UNSPECIFIED', ('UNSPECIFIED'), ('UNSPECIFIED'), ('UNSPECIFIED') ) ;
#21592 = CARTESIAN_POINT ( 'NONE',  ( -0.2399999999999999079, -2.026158573466832813, -0.3155405389364159263 ) ) ;
#21593 = CARTESIAN_POINT ( 'NONE',  ( 0.5694934407712974878, -1.613350223101006620, 0.4177417262808785781 ) ) ;
#21594 = CARTESIAN_POINT ( 'NONE',  ( 0.1117288206367789555, -1.275843495540134320, 0.6175638907962521795 ) ) ;
#21595 = EDGE_CURVE ( 'NONE', #38334, #13520, #20030, .T. ) ;
#21596 = CARTESIAN_POINT ( 'NONE',  ( 0.1974716765470868052, -1.244701664176973255, -0.7187326247832954706 ) ) ;
#21597 = CARTESIAN_POINT ( 'NONE',  ( 1.365923996832131609E-16, -0.9481888444201339583, 0.1457185332388703791 ) ) ;
#21598 = PRODUCT_CONTEXT ( 'NONE', #24276, 'mechanical' ) ;
#21599 = ADVANCED_FACE ( 'NONE', ( #26576 ), #26784, .F. ) ;
#21600 = EDGE_CURVE ( 'NONE', #9596, #30066, #38397, .T. ) ;
#21601 = CARTESIAN_POINT ( 'NONE',  ( 0.4743695099260452075, -1.117357713078968695, 0.5498565627795439781 ) ) ;
#21602 = CARTESIAN_POINT ( 'NONE',  ( 0.4444931384256880502, -1.226103329170601386, 0.5856983068965044836 ) ) ;
#21603 = CARTESIAN_POINT ( 'NONE',  ( 0.3439431471759914483, -1.238012385881360533, -0.5155029497116575543 ) ) ;
#21604 = EDGE_CURVE ( 'NONE', #1766, #9912, #30061, .T. ) ;
#21605 = CARTESIAN_POINT ( 'NONE',  ( 0.05086546246741921462, -1.198860143930047473, 0.7015125153497857591 ) ) ;
#21606 = PLANE ( 'NONE',  #18624 ) ;
#21607 = CARTESIAN_POINT ( 'NONE',  ( -0.2136509456379319383, -0.4946207598421926699, 0.09999999999999989453 ) ) ;
#21608 = CARTESIAN_POINT ( 'NONE',  ( -0.1212602504878774051, -0.5073146173917496560, 0.1528658435937000626 ) ) ;
#21609 = ORIENTED_EDGE ( 'NONE', *, *, #25279, .F. ) ;
#21610 = VERTEX_POINT ( 'NONE', #15225 ) ;
#21611 = CARTESIAN_POINT ( 'NONE',  ( -0.1154362047090707333, -0.5278818619434392234, 0.1319635891399765504 ) ) ;
#21612 = VERTEX_POINT ( 'NONE', #22038 ) ;
#21613 = DIRECTION ( 'NONE',  ( -1.000000000000000000, -2.341930812374887555E-31, 1.664003471950578127E-31 ) ) ;
#21614 = CARTESIAN_POINT ( 'NONE',  ( -0.1171721259116263736, -0.4872713820691137454, 0.1209876223252377009 ) ) ;
#21616 = ORIENTED_EDGE ( 'NONE', *, *, #1771, .T. ) ;
#21615 = PLANE ( 'NONE',  #14706 ) ;
#21617 = VERTEX_POINT ( 'NONE', #27783 ) ;
#21618 = ORIENTED_EDGE ( 'NONE', *, *, #11163, .T. ) ;
#21619 = CARTESIAN_POINT ( 'NONE',  ( 0.04155248107635927529, 0.4523094957185405662, -0.1288470070525098432 ) ) ;
#21620 = EDGE_LOOP ( 'NONE', ( #7151, #17762, #20862 ) ) ;
#21621 = CARTESIAN_POINT ( 'NONE',  ( 0.01818706982255626978, -0.6782422388700252158, 0.5155022423221341521 ) ) ;
#21623 = DIRECTION ( 'NONE',  ( 0.000000000000000000, 0.000000000000000000, -1.000000000000000000 ) ) ;
#21622 = CARTESIAN_POINT ( 'NONE',  ( 0.06444297064315794576, -0.8352831487901670737, 0.1457185332388703236 ) ) ;
#21624 = CARTESIAN_POINT ( 'NONE',  ( -1.502516396515344672E-15, -0.3899999999999999578, 5.463695987328526437E-16 ) ) ;
#21625 = EDGE_CURVE ( 'NONE', #40154, #35767, #38464, .T. ) ;
#21626 = DIRECTION ( 'NONE',  ( 0.4999551463232372317, -0.8660512985181135770, 0.000000000000000000 ) ) ;
#21628 = ORIENTED_EDGE ( 'NONE', *, *, #3123, .T. ) ;
#21627 = ORIENTED_EDGE ( 'NONE', *, *, #3385, .T. ) ;
#21629 = ADVANCED_FACE ( 'NONE', ( #3098 ), #11409, .T. ) ;
#21630 = CARTESIAN_POINT ( 'NONE',  ( 0.4688459138424371786, -1.061988423737608045, -0.4248180574663140141 ) ) ;
#21631 = CARTESIAN_POINT ( 'NONE',  ( 0.2625973931889362678, -0.6796768235205253861, 0.1477649966949237115 ) ) ;
#21632 = DIRECTION ( 'NONE',  ( 1.000000000000000000, 0.000000000000000000, 0.000000000000000000 ) ) ;
#21633 = CARTESIAN_POINT ( 'NONE',  ( 0.5182059338286948424, -1.328740440620357344, 0.7997488878819424274 ) ) ;
#21634 = FACE_OUTER_BOUND ( 'NONE', #31560, .T. ) ;
#21635 = CARTESIAN_POINT ( 'NONE',  ( 0.2289168280753887674, -1.471836432603705669, 0.9194637683477111523 ) ) ;
#21636 = CARTESIAN_POINT ( 'NONE',  ( 0.1486919001366245052, -1.066606737835706253, 0.9727470820782289085 ) ) ;
#21637 = B_SPLINE_CURVE_WITH_KNOTS ( 'NONE', 3,
 ( #9390, #21967, #34496, #6308 ),
 .UNSPECIFIED., .F., .F.,
 ( 4, 4 ),
 ( 0.000000000000000000, 0.001175067160604181338 ),
 .UNSPECIFIED. ) ;
#21638 = APPLICATION_CONTEXT ( 'configuration controlled 3d designs of mechanical parts and assemblies' ) ;
#21639 = DIRECTION ( 'NONE',  ( -1.000000000000000000, -2.280301054154496446E-31, -1.355854680848613603E-31 ) ) ;
#21640 = CARTESIAN_POINT ( 'NONE',  ( 0.6589703859825570831, -1.564329074718757484, 0.3667417262808780887 ) ) ;
#21641 =( BOUNDED_SURFACE ( )  B_SPLINE_SURFACE ( 3, 2, ( 
 ( #32574, #14448, #39543 ),
 ( #20436, #10776, #35871 ),
 ( #13840, #32768, #33385 ),
 ( #7684, #17351, #39354 ),
 ( #36680, #38947, #29694 ),
 ( #11175, #17743, #20249 ),
 ( #4570, #11377, #39163 ),
 ( #23549, #33190, #30293 ),
 ( #26827, #17142, #23945 ),
 ( #36259, #14056, #30103 ),
 ( #17561, #23349, #23732 ),
 ( #1536, #8486, #1751 ),
 ( #5387, #29910, #5188 ),
 ( #26635, #17949, #2125 ),
 ( #33574, #26414, #4994 ),
 ( #36479, #36066, #14262 ),
 ( #1934, #24156, #27016 ),
 ( #10992, #7865, #14659 ),
 ( #8292, #32973, #27228 ),
 ( #1333, #4777, #8077 ),
 ( #20651, #20864, #39764 ),
 ( #11594, #21047, #27626 ),
 ( #12390, #40369, #18159 ),
 ( #22088, #11783, #9096 ) ),
 .UNSPECIFIED., .F., .F., .F. ) 
 B_SPLINE_SURFACE_WITH_KNOTS ( ( 4, 2, 2, 2, 2, 2, 2, 2, 2, 2, 2, 4 ),
 ( 3, 3 ),
 ( 0.004472361800415559571, 0.007241614148789993731, 0.01001086649716442789, 0.01278011884553886292, 0.01554937119391329794, 0.01831862354228773471, 0.02108787589066216800, 0.02247250206484938465, 0.02385712823903660129, 0.02454944132613021135, 0.02524175441322381794, 0.02662638058741103458 ),
 ( 0.000000000000000000, 1.000000000000000000 ),
 .UNSPECIFIED. ) 
 GEOMETRIC_REPRESENTATION_ITEM ( )  RATIONAL_B_SPLINE_SURFACE ( (
 ( 1.000000000000000000, 0.7071530416912251704, 1.000000000000000000),
 ( 1.000000000000000000, 0.7073709362457231142, 1.000000000000000000),
 ( 1.000000000000000000, 0.7092808763967833885, 1.000000000000000000),
 ( 1.000000000000000000, 0.7141524243381439652, 1.000000000000000000),
 ( 1.000000000000000000, 0.7171571039999593555, 1.000000000000000000),
 ( 1.000000000000000000, 0.7235522545071346734, 1.000000000000000000),
 ( 1.000000000000000000, 0.7269749645788134984, 1.000000000000000000),
 ( 1.000000000000000000, 0.7340382794361808294, 1.000000000000000000),
 ( 1.000000000000000000, 0.7376893573657878900, 1.000000000000000000),
 ( 1.000000000000000000, 0.7449955946419650754, 1.000000000000000000),
 ( 1.000000000000000000, 0.7486754894461632448, 1.000000000000000000),
 ( 1.000000000000000000, 0.7552984250705360170, 1.000000000000000000),
 ( 1.000000000000000000, 0.7583398789584828714, 1.000000000000000000),
 ( 1.000000000000000000, 0.7606811803337633071, 1.000000000000000000),
 ( 1.000000000000000000, 0.7610729208801710888, 1.000000000000000000),
 ( 1.000000000000000000, 0.7601897444684649896, 1.000000000000000000),
 ( 1.000000000000000000, 0.7589468570669724024, 1.000000000000000000),
 ( 1.000000000000000000, 0.7545561764466856003, 1.000000000000000000),
 ( 1.000000000000000000, 0.7526619229726708715, 1.000000000000000000),
 ( 1.000000000000000000, 0.7476192217998193223, 1.000000000000000000),
 ( 1.000000000000000000, 0.7444481429157411290, 1.000000000000000000),
 ( 1.000000000000000000, 0.7327145509101834486, 1.000000000000000000),
 ( 1.000000000000000000, 0.7217852786214301597, 1.000000000000000000),
 ( 1.000000000000000000, 0.7071189998922933206, 1.000000000000000000) ) ) 
 REPRESENTATION_ITEM ( '' )  SURFACE ( )  );
#21642 = PLANE ( 'NONE',  #895 ) ;
#21643 = CARTESIAN_POINT ( 'NONE',  ( 0.4634712904840415093, -1.711704060178988129, -0.5155029497116575543 ) ) ;
#21644 = B_SPLINE_CURVE_WITH_KNOTS ( 'NONE', 3,
 ( #18476, #31249, #30829, #24680, #2460, #5917, #28157, #2852, #14996, #33705, #15188, #27549, #27957, #15401, #40497, #3251 ),
 .UNSPECIFIED., .F., .F.,
 ( 4, 2, 2, 2, 2, 2, 2, 4 ),
 ( 0.000000000000000000, 0.001141425056121503443, 0.001712137584182261887, 0.002282850112243020764, 0.002853562640303779208, 0.003424275168364537651, 0.003994987696425296095, 0.004565700224486055406 ),
 .UNSPECIFIED. ) ;
#21645 = CARTESIAN_POINT ( 'NONE',  ( -0.2399999999999999079, -1.835749455202394298, -0.3938319975228649072 ) ) ;
#21646 = CARTESIAN_POINT ( 'NONE',  ( 0.003124719664520368614, -0.5686731593868924461, 0.1457185332388688526 ) ) ;
#21647 = CARTESIAN_POINT ( 'NONE',  ( 0.08392504549576879080, -1.205435068169474988, 0.7615968429824111485 ) ) ;
#21648 = PERSON_AND_ORGANIZATION ( #28500, #32463 ) ;
#21649 = CARTESIAN_POINT ( 'NONE',  ( 0.3234650319091952331, -0.8156164872106268504, 0.7066254915499745604 ) ) ;
#21650 = CARTESIAN_POINT ( 'NONE',  ( 0.6704502323737214775, -1.558777008743201353, 0.6054797769067454816 ) ) ;
#21651 = DIRECTION ( 'NONE',  ( 1.000000000000000000, 2.403560570595279103E-31, -1.725633230170969455E-31 ) ) ;
#21652 = DIRECTION ( 'NONE',  ( 0.000000000000000000, 0.000000000000000000, -1.000000000000000000 ) ) ;
#21653 = ORIENTED_EDGE ( 'NONE', *, *, #37822, .F. ) ;
#21654 = CYLINDRICAL_SURFACE ( 'NONE', #9270, 0.1849999999999994982 ) ;
#21655 = CARTESIAN_POINT ( 'NONE',  ( 0.2642540606809890558, -1.625850527579886018, 0.8231221639007153534 ) ) ;
#21656 = CARTESIAN_POINT ( 'NONE',  ( 0.1291821447933259592, -0.5731434977924334540, 0.2461200965963110388 ) ) ;
#21658 = ORIENTED_EDGE ( 'NONE', *, *, #25741, .T. ) ;
#21657 = CARTESIAN_POINT ( 'NONE',  ( 0.1133170741025229245, -1.391401617297857163, 0.5182417262812423209 ) ) ;
#21659 = CARTESIAN_POINT ( 'NONE',  ( 0.2766509774079478068, -0.8188515361471339071, 0.5743688119339978027 ) ) ;
#21661 = ORIENTED_EDGE ( 'NONE', *, *, #1902, .F. ) ;
#21660 = VERTEX_POINT ( 'NONE', #1063 ) ;
#21662 = CARTESIAN_POINT ( 'NONE',  ( 0.2628562773071145275, -0.7496856360161251454, 0.5667459045074426660 ) ) ;
#21663 = CARTESIAN_POINT ( 'NONE',  ( 0.3621938380462905172, -1.694500576257093494, -0.5862319126744306441 ) ) ;
#21664 = CARTESIAN_POINT ( 'NONE',  ( 0.5264113014007820723, -1.640729993778254014, 0.5682417262808777680 ) ) ;
#21665 = APPROVAL_STATUS ( 'not_yet_approved' ) ;
#21666 = DIRECTION ( 'NONE',  ( 0.4999551463232373427, -0.8660512985181134660, 0.000000000000000000 ) ) ;
#21667 = VERTEX_POINT ( 'NONE', #23040 ) ;
#21668 = CARTESIAN_POINT ( 'NONE',  ( 0.09800014303332876819, -0.7423468218336800595, 0.3236582407429515196 ) ) ;
#21669 = CARTESIAN_POINT ( 'NONE',  ( 0.2211959769661342168, -1.309495541150525799, -0.2869361388274796476 ) ) ;
#21670 = CARTESIAN_POINT ( 'NONE',  ( 0.1091101412475568994, -0.5932495664807553304, 0.3114501276851988631 ) ) ;
#21672 = CARTESIAN_POINT ( 'NONE',  ( 0.001904821466202900188, -0.5284344570646690720, 0.09157858422922257602 ) ) ;
#21671 = CARTESIAN_POINT ( 'NONE',  ( 0.3259879919982053287, -1.767950897709265945, 0.5312986935552727052 ) ) ;
#21673 = CARTESIAN_POINT ( 'NONE',  ( 0.04300737265183255525, -1.224161303901022180, 0.6631612324643675338 ) ) ;
#21674 = ORIENTED_EDGE ( 'NONE', *, *, #33140, .F. ) ;
#21675 = CARTESIAN_POINT ( 'NONE',  ( 0.4488584268620961493, -1.696961260237186409, 0.5959601211048285441 ) ) ;
#21676 = CARTESIAN_POINT ( 'NONE',  ( 0.6140150280136293937, -1.296280020069253469, 0.8682680789332258842 ) ) ;
#21677 = DIRECTION ( 'NONE',  ( 0.000000000000000000, 0.000000000000000000, -1.000000000000000000 ) ) ;
#21678 = CARTESIAN_POINT ( 'NONE',  ( -0.1680316146028584534, 0.5219773800263004526, 0.3170215181389828829 ) ) ;
#21679 = DIRECTION ( 'NONE',  ( 0.000000000000000000, 3.330669073875470114E-16, 1.000000000000000000 ) ) ;
#21680 = CARTESIAN_POINT ( 'NONE',  ( 0.5972608898831076596, -1.261123752139667875, 0.6057417262808246772 ) ) ;
#21681 = CARTESIAN_POINT ( 'NONE',  ( 0.001114027946886548409, -1.914171052033790899, -0.6529051036212328851 ) ) ;
#21682 = PLANE ( 'NONE',  #23182 ) ;
#21683 = CARTESIAN_POINT ( 'NONE',  ( 0.4299297405268334149, -1.031605064505895619, 0.6882246241152528698 ) ) ;
#21684 = COORDINATED_UNIVERSAL_TIME_OFFSET ( 0, 0, .AHEAD. ) ;
#21685 = CARTESIAN_POINT ( 'NONE',  ( -0.05464101615137796630, -2.183180860297908144, -0.4937760292030871079 ) ) ;
#21686 = B_SPLINE_CURVE_WITH_KNOTS ( 'NONE', 3,
 ( #21503, #15306, #3163, #5634, #21901, #12417, #31152, #39986, #11808, #6029, #34021, #18597 ),
 .UNSPECIFIED., .F., .F.,
 ( 4, 2, 2, 2, 2, 4 ),
 ( -5.999999998893646056E-08, 0.0004327397255088311447, 0.0008655394510176511996, 0.001731138902035301826, 0.002596738353052953103, 0.003462337804070603729 ),
 .UNSPECIFIED. ) ;
#21687 = CARTESIAN_POINT ( 'NONE',  ( 0.1779790066342687160, -1.874427033017872279, -0.6554133151439877070 ) ) ;
#21688 = CARTESIAN_POINT ( 'NONE',  ( 0.4000099798367696691, -1.704638381955406734, 0.4182417262808776903 ) ) ;
#21689 = CARTESIAN_POINT ( 'NONE',  ( -0.05281452789367711842, -0.3064952470001998663, -0.3541670097232285652 ) ) ;
#21690 = ORIENTED_EDGE ( 'NONE', *, *, #260, .F. ) ;
#21691 = CARTESIAN_POINT ( 'NONE',  ( 0.4670213778778394831, -1.236191465557153757, 0.6057417262809817737 ) ) ;
#21692 = DIRECTION ( 'NONE',  ( -1.188678714063518227E-15, 1.000000000000000000, 3.263080277421930985E-16 ) ) ;
#21693 = CIRCLE ( 'NONE', #73, 0.1849999999999994982 ) ;
#21694 = CARTESIAN_POINT ( 'NONE',  ( -0.2399999999999999079, -2.183180860297908144, -0.2991170932241127844 ) ) ;
#21695 = VERTEX_POINT ( 'NONE', #13573 ) ;
#21696 = CARTESIAN_POINT ( 'NONE',  ( -0.05489899477340628303, 0.02536133381296927503, -0.4620560448752992211 ) ) ;
#21697 = CARTESIAN_POINT ( 'NONE',  ( 0.06001981139707002200, -1.214044704396488594, 0.7646275528860384529 ) ) ;
#21699 = ORIENTED_EDGE ( 'NONE', *, *, #26108, .F. ) ;
#21698 = ORIENTED_EDGE ( 'NONE', *, *, #37112, .T. ) ;
#21700 = DIRECTION ( 'NONE',  ( 0.000000000000000000, 0.000000000000000000, 1.000000000000000000 ) ) ;
#21701 = CIRCLE ( 'NONE', #26382, 0.03000000000000002318 ) ;
#21702 = DIRECTION ( 'NONE',  ( 0.8056764635542885689, 0.4651018882076579097, -0.3668319365326945247 ) ) ;
#21703 = CARTESIAN_POINT ( 'NONE',  ( 0.04157078424165231573, -0.4416882993450223505, -0.1614266821413831432 ) ) ;
#21704 = CARTESIAN_POINT ( 'NONE',  ( 0.3727196660074906243, -1.733127303661048613, -0.5289265956312534378 ) ) ;
#21705 = DIRECTION ( 'NONE',  ( -0.8660512985181130219, -0.4999551463232380644, 0.000000000000000000 ) ) ;
#21707 = DIRECTION ( 'NONE',  ( -0.4999551463232372317, 0.8660512985181134660, -0.000000000000000000 ) ) ;
#21706 = CARTESIAN_POINT ( 'NONE',  ( 0.05268850283020568709, 0.4471020566665044327, 0.1404229504685621521 ) ) ;
#21708 = CARTESIAN_POINT ( 'NONE',  ( 0.04575106512774653605, -0.3363942840372673437, -0.3523417416125881885 ) ) ;
#21709 = ORIENTED_EDGE ( 'NONE', *, *, #24584, .F. ) ;
#21710 = CARTESIAN_POINT ( 'NONE',  ( 0.1090682129762271801, -0.6262447015380825377, 0.4004099436828046366 ) ) ;
#21711 = ORIENTED_EDGE ( 'NONE', *, *, #19696, .F. ) ;
#21712 = CARTESIAN_POINT ( 'NONE',  ( 0.7071069014570956490, -1.521634513519168452, 0.5617257377400114438 ) ) ;
#21713 = CARTESIAN_POINT ( 'NONE',  ( 0.2830252135639645394, -1.159611347306545470, 0.8504159276851470661 ) ) ;
#21714 = ADVANCED_FACE ( 'NONE', ( #19734 ), #10473, .T. ) ;
#21716 = CARTESIAN_POINT ( 'NONE',  ( 0.5766475765793911412, -1.620807927452676767, 0.4730587198120521641 ) ) ;
#21715 = DIRECTION ( 'NONE',  ( -0.2221717918550268900, -0.8554093761208125812, -0.4678829919419264516 ) ) ;
#21717 = CARTESIAN_POINT ( 'NONE',  ( -2.070754768975508586, -0.09959325338431662678, 0.3600000000000021516 ) ) ;
#21718 = DIRECTION ( 'NONE',  ( -8.881784197001246407E-16, 2.361472542561082612E-16, -1.000000000000000000 ) ) ;
#21719 = APPLIED_DATE_AND_TIME_ASSIGNMENT ( #34506, #31233, ( #22077 ) ) ;
#21720 = DIRECTION ( 'NONE',  ( 1.000000000000000000, 2.403560570595279103E-31, -1.725633230170969455E-31 ) ) ;
#21721 = CARTESIAN_POINT ( 'NONE',  ( 0.3997154711467377219, -2.078397263467336664, -0.4724987659684973806 ) ) ;
#21722 = CARTESIAN_POINT ( 'NONE',  ( 0.5804045214929907104, -1.495121667922066910, 0.5634096241211530298 ) ) ;
#21723 = CARTESIAN_POINT ( 'NONE',  ( 0.4343371540759652372, -1.702447133182462435, 0.4323261742870332935 ) ) ;
#21724 = DIRECTION ( 'NONE',  ( -0.4999999999999987232, 0.4254978411528142490, 0.7542887956043731190 ) ) ;
#21725 = CARTESIAN_POINT ( 'NONE',  ( -0.2399999999999999079, -1.804235510932644004, -0.1101860188971505033 ) ) ;
#21726 = AXIS2_PLACEMENT_3D ( 'NONE', #9957, #28088, #31376 ) ;
#21727 = CARTESIAN_POINT ( 'NONE',  ( 0.2101951102887192890, -1.233953443661628846, 0.5631135429232324574 ) ) ;
#21728 = CARTESIAN_POINT ( 'NONE',  ( 0.05999999999999990757, -0.3767386922704979990, -0.2665524483967541269 ) ) ;
#21729 = CARTESIAN_POINT ( 'NONE',  ( 0.6277259471038021399, -1.316916163187945799, 0.8316945246157878557 ) ) ;
#21730 = B_SPLINE_CURVE_WITH_KNOTS ( 'NONE', 3,
 ( #15706, #40600, #37308, #15519, #30739, #15095, #28252, #37498, #5823, #116, #8515, #9120 ),
 .UNSPECIFIED., .F., .F.,
 ( 4, 2, 2, 2, 2, 4 ),
 ( 0.002469872543621277027, 0.003821559213351475789, 0.005173245883081675420, 0.006524932552811874183, 0.007200775887676973130, 0.007876619222542072946 ),
 .UNSPECIFIED. ) ;
#21731 = AXIS2_PLACEMENT_3D ( 'NONE', #30852, #24486, #37020 ) ;
#21732 = EDGE_CURVE ( 'NONE', #3317, #31622, #14769, .T. ) ;
#21733 = CARTESIAN_POINT ( 'NONE',  ( -0.04945776359514872378, 0.2513414220725579407, 0.4057848608195681606 ) ) ;
#21734 = CARTESIAN_POINT ( 'NONE',  ( 0.003994112659391831251, -0.9740337013070538008, 0.4215942553239714341 ) ) ;
#21735 = CIRCLE ( 'NONE', #1404, 0.03000000000000006134 ) ;
#21736 = CARTESIAN_POINT ( 'NONE',  ( 0.5838521633088137319, -1.602265608861538793, -0.4542598492692566658 ) ) ;
#21737 = CARTESIAN_POINT ( 'NONE',  ( 0.1897018898765783779, -0.7780637555336420430, 0.2978648193278307654 ) ) ;
#21738 = FACE_OUTER_BOUND ( 'NONE', #31631, .T. ) ;
#21739 = CARTESIAN_POINT ( 'NONE',  ( 0.03662792686184422608, 0.2484399233013424024, -0.4119056456069861705 ) ) ;
#21740 = DIRECTION ( 'NONE',  ( -1.000000000000000000, -0.000000000000000000, -0.000000000000000000 ) ) ;
#21741 = EDGE_CURVE ( 'NONE', #38795, #29445, #657, .T. ) ;
#21742 = SHAPE_REPRESENTATION ( 'Cage Hanger', ( #27819 ), #33713 ) ;
#21743 = EDGE_LOOP ( 'NONE', ( #4738, #26769, #16050, #19382 ) ) ;
#21744 = CARTESIAN_POINT ( 'NONE',  ( 0.3599187094839055856, -1.738735253168089967, -0.5101712951092032267 ) ) ;
#21745 = CARTESIAN_POINT ( 'NONE',  ( 0.3819143772994754715, -1.729703839012011857, -0.5841330926933957501 ) ) ;
#21746 = ADVANCED_FACE ( 'NONE', ( #31885 ), #3611, .F. ) ;
#21747 = CARTESIAN_POINT ( 'NONE',  ( 0.6527381947427340902, -1.527960125101692768, 0.4182417262808776903 ) ) ;
#21748 = CARTESIAN_POINT ( 'NONE',  ( 0.08298671528866649605, -0.8222748340196127659, 0.1457185332388708787 ) ) ;
#21749 = EDGE_CURVE ( 'NONE', #1874, #26668, #11483, .T. ) ;
#21750 = CARTESIAN_POINT ( 'NONE',  ( 0.4179778656386031743, -1.682263187816546157, -0.6165510159742800811 ) ) ;
#21751 = ADVANCED_FACE ( 'NONE', ( #38654 ), #418, .F. ) ;
#21752 = EDGE_LOOP ( 'NONE', ( #3573, #26079, #1974, #25190 ) ) ;
#21753 = CARTESIAN_POINT ( 'NONE',  ( -0.02000000000000000042, -1.598492537578166672, -0.3371380022280838773 ) ) ;
#21754 = CARTESIAN_POINT ( 'NONE',  ( 0.3660523240620164875, -1.128919933506183471, 0.6218697989683404925 ) ) ;
#21755 = DIRECTION ( 'NONE',  ( 0.8660512985181133550, 0.4999551463232373982, 0.000000000000000000 ) ) ;
#21756 = CARTESIAN_POINT ( 'NONE',  ( 0.04308611741967133257, 0.3346393142056199310, -0.3638101219459927149 ) ) ;
#21757 = CARTESIAN_POINT ( 'NONE',  ( 0.5082032253465859073, -1.306217543967353123, 0.6299990673569597632 ) ) ;
#21758 = AXIS2_PLACEMENT_3D ( 'NONE', #31235, #36979, #8799 ) ;
#21760 = ORIENTED_EDGE ( 'NONE', *, *, #22495, .T. ) ;
#21759 = DIRECTION ( 'NONE',  ( 0.000000000000000000, 0.000000000000000000, 1.000000000000000000 ) ) ;
#21761 = CARTESIAN_POINT ( 'NONE',  ( 0.5117280326951013647, -1.115088012504228621, 0.5923667439031021775 ) ) ;
#21762 = ORIENTED_EDGE ( 'NONE', *, *, #38689, .T. ) ;
#21763 = COORDINATED_UNIVERSAL_TIME_OFFSET ( 0, 0, .AHEAD. ) ;
#21764 = CARTESIAN_POINT ( 'NONE',  ( 0.09908208500843325439, -1.366949803050675261, 0.6729494607312549448 ) ) ;
#21765 = ORIENTED_EDGE ( 'NONE', *, *, #39336, .T. ) ;
#21766 = AXIS2_PLACEMENT_3D ( 'NONE', #11683, #21149, #33679 ) ;
#21767 = CARTESIAN_POINT ( 'NONE',  ( 0.06532065983977884682, -0.7045720426608378384, 0.5366528578034658326 ) ) ;
#21768 = ADVANCED_FACE ( 'NONE', ( #6321 ), #24867, .T. ) ;
#21770 = CARTESIAN_POINT ( 'NONE',  ( 0.1118013512516233404, -0.8708971820562737554, -0.01152571254326707761 ) ) ;
#21769 = CARTESIAN_POINT ( 'NONE',  ( 0.06477686075188948678, -0.8276703782281517041, 0.09804374420191747097 ) ) ;
#21771 = CARTESIAN_POINT ( 'NONE',  ( 0.1909286924077255032, -1.257064795538239022, -0.3194753470178354759 ) ) ;
#21772 = AXIS2_PLACEMENT_3D ( 'NONE', #15159, #37372, #40253 ) ;
#21773 = APPLIED_PERSON_AND_ORGANIZATION_ASSIGNMENT ( #23480, #1672, ( #30071 ) ) ;
#21774 = ORIENTED_EDGE ( 'NONE', *, *, #11727, .T. ) ;
#21775 = AXIS2_PLACEMENT_3D ( 'NONE', #7020, #10508, #13791 ) ;
#21776 = ORIENTED_EDGE ( 'NONE', *, *, #24977, .F. ) ;
#21777 = ORIENTED_EDGE ( 'NONE', *, *, #29736, .T. ) ;
#21778 = CARTESIAN_POINT ( 'NONE',  ( 0.4760996380614069823, -1.068744558855534432, 0.6220588924540169096 ) ) ;
#21779 = CARTESIAN_POINT ( 'NONE',  ( 0.1377143472285344561, -0.6768556682296630322, 0.4686332729017968490 ) ) ;
#21780 = EDGE_LOOP ( 'NONE', ( #9101, #28913, #9508, #38450 ) ) ;
#21781 = CARTESIAN_POINT ( 'NONE',  ( 0.2060189241777141689, -2.107936428766273629, -0.2870436526301869407 ) ) ;
#21782 = DIRECTION ( 'NONE',  ( 0.000000000000000000, 0.000000000000000000, -1.000000000000000000 ) ) ;
#21783 = FACE_OUTER_BOUND ( 'NONE', #23587, .T. ) ;
#21784 = CARTESIAN_POINT ( 'NONE',  ( -0.1210148435730253880, -0.5061394519557965710, 0.3122829191278980177 ) ) ;
#21785 = TOROIDAL_SURFACE ( 'NONE', #11928, 0.2200000000000000566, 0.02999999999999999889 ) ;
#21786 = CARTESIAN_POINT ( 'NONE',  ( 0.4345963605075027769, -1.690632822822775827, 0.4263932049186950901 ) ) ;
#21787 = CARTESIAN_POINT ( 'NONE',  ( 0.07279096728935340044, -1.323295152996974977, 0.4931969685770185019 ) ) ;
#21788 = FACE_OUTER_BOUND ( 'NONE', #39010, .T. ) ;
#21789 = FACE_OUTER_BOUND ( 'NONE', #24290, .T. ) ;
#21790 = CARTESIAN_POINT ( 'NONE',  ( 0.05796715499547382133, -1.320156192035571774, 0.6033327867956804758 ) ) ;
#21791 = DATE_AND_TIME ( #34730, #29898 ) ;
#21792 = AXIS2_PLACEMENT_3D ( 'NONE', #4091, #35189, #13154 ) ;
#21793 = CARTESIAN_POINT ( 'NONE',  ( 0.3845716336272441138, -1.023253965646789831, 0.6260147105531964629 ) ) ;
#21794 = CARTESIAN_POINT ( 'NONE',  ( 0.4815930311117895823, -1.120787884457994599, 0.5308384764438787151 ) ) ;
#21795 = CARTESIAN_POINT ( 'NONE',  ( 0.5565267853031266032, -1.184521675161833043, 0.6057417262809816627 ) ) ;
#21796 = LINE ( 'NONE', #15202, #33053 ) ;
#21797 = ADVANCED_FACE ( 'NONE', ( #37387 ), #9200, .F. ) ;
#21798 = AXIS2_PLACEMENT_3D ( 'NONE', #24555, #17566, #30109 ) ;
#21799 = CARTESIAN_POINT ( 'NONE',  ( -0.002175845014896822093, -0.8193767622554530838, 0.2897257274743089139 ) ) ;
#21800 = CARTESIAN_POINT ( 'NONE',  ( -0.2399999999999999079, -4.121841830394775030, -0.5449218438908057793 ) ) ;
#21801 = AXIS2_PLACEMENT_3D ( 'NONE', #24935, #21861, #34388 ) ;
#21802 = EDGE_CURVE ( 'NONE', #31054, #21617, #15600, .T. ) ;
#21803 = CARTESIAN_POINT ( 'NONE',  ( -0.2399999999999999079, -4.176085227118957022, -0.6840180543573738392 ) ) ;
#21804 = CARTESIAN_POINT ( 'NONE',  ( 0.3417290234946780969, -1.631754028364875264, 0.4817266676845163853 ) ) ;
#21805 = EDGE_CURVE ( 'NONE', #35767, #32520, #15869, .T. ) ;
#21806 = EDGE_LOOP ( 'NONE', ( #32166, #27070, #15608, #21373 ) ) ;
#21808 = ORIENTED_EDGE ( 'NONE', *, *, #28599, .T. ) ;
#21807 = B_SPLINE_SURFACE_WITH_KNOTS ( 'NONE', 1, 3, ( 
 ( #40423, #9343, #15331, #30563 ),
 ( #18405, #39817, #2386, #15115 ),
 ( #37139, #27675, #11642, #14926 ),
 ( #33855, #2993, #30957, #2782 ) ),
 .UNSPECIFIED., .F., .F., .F.,
 ( 2, 1, 1, 2 ),
 ( 4, 4 ),
 ( -1.012000000000000233, 0.000000000000000000, 1.000000000000000000, 2.018000000000001126 ),
 ( -0.005833846140041338939, 0.005833846140041338071 ),
 .UNSPECIFIED. ) ;
#21809 = DIRECTION ( 'NONE',  ( 1.000000000000000000, -1.049121689386597152E-11, 1.416614914756796105E-11 ) ) ;
#21810 = ORIENTED_EDGE ( 'NONE', *, *, #32320, .F. ) ;
#21811 = DIRECTION ( 'NONE',  ( -1.000000000000000000, -0.000000000000000000, -0.000000000000000000 ) ) ;
#21812 = DIRECTION ( 'NONE',  ( 0.000000000000000000, 3.330669073875470114E-16, 1.000000000000000000 ) ) ;
#21813 = CARTESIAN_POINT ( 'NONE',  ( 0.5116187330526053012, -1.317947182177965804, 0.7954296552626618499 ) ) ;
#21815 = VERTEX_POINT ( 'NONE', #5904 ) ;
#21814 = DIRECTION ( 'NONE',  ( 0.3468893892380797705, -0.7770416411309306604, 0.5252371270032060169 ) ) ;
#21816 = VECTOR ( 'NONE', #3194, 39.37007874015748143 ) ;
#21817 = ORIENTED_EDGE ( 'NONE', *, *, #19987, .F. ) ;
#21818 = CARTESIAN_POINT ( 'NONE',  ( 0.02231181081520726070, 0.4612879682508960189, -0.2235517164227164566 ) ) ;
#21819 = ORIENTED_EDGE ( 'NONE', *, *, #21825, .T. ) ;
#21820 = CARTESIAN_POINT ( 'NONE',  ( 0.01251345383894142578, -0.5638626234200834197, 0.2823644336484513739 ) ) ;
#21821 = EDGE_CURVE ( 'NONE', #20386, #9762, #743, .T. ) ;
#21823 = CARTESIAN_POINT ( 'NONE',  ( 0.08016089217752186968, -1.309201107948811504, 0.5631135211526980822 ) ) ;
#21822 = CARTESIAN_POINT ( 'NONE',  ( 0.5087011370554738177, -1.685593719371816679, -0.4274642268707216641 ) ) ;
#21824 = CYLINDRICAL_SURFACE ( 'NONE', #38422, 0.1033070866141734129 ) ;
#21825 = EDGE_CURVE ( 'NONE', #10513, #30976, #32550, .T. ) ;
#21826 = VECTOR ( 'NONE', #17065, 39.37007874015748143 ) ;
#21827 = FACE_OUTER_BOUND ( 'NONE', #10504, .T. ) ;
#21829 = ORIENTED_EDGE ( 'NONE', *, *, #8061, .F. ) ;
#21828 = ORIENTED_EDGE ( 'NONE', *, *, #39339, .T. ) ;
#21830 = EDGE_CURVE ( 'NONE', #4931, #14515, #37487, .T. ) ;
#21831 = LINE ( 'NONE', #37250, #24431 ) ;
#21832 = CARTESIAN_POINT ( 'NONE',  ( -0.02000000000000000042, -1.599201040860868339, 0.1642182323853691728 ) ) ;
#21833 = CARTESIAN_POINT ( 'NONE',  ( -0.03877220711930352143, -0.4416859332762705370, 0.1784371778270249786 ) ) ;
#21834 = CARTESIAN_POINT ( 'NONE',  ( 0.4881568739066119433, -1.310886444036855947, 0.8120130285850476470 ) ) ;
#21835 = AXIS2_PLACEMENT_3D ( 'NONE', #25373, #28844, #9300 ) ;
#21836 = EDGE_CURVE ( 'NONE', #12108, #35653, #31239, .T. ) ;
#21837 = CIRCLE ( 'NONE', #8669, 0.01500000000000000812 ) ;
#21838 = CARTESIAN_POINT ( 'NONE',  ( 0.2496972935526009241, -0.9635046127537866267, 0.6859288853639479155 ) ) ;
#21839 = CARTESIAN_POINT ( 'NONE',  ( 0.2746970422698945535, -1.662148702819467694, 0.7072477570165817129 ) ) ;
#21840 = AXIS2_PLACEMENT_3D ( 'NONE', #9955, #947, #4183 ) ;
#21841 = CARTESIAN_POINT ( 'NONE',  ( 0.08540438715202058884, -0.8281466500289427213, 0.8274849438104245891 ) ) ;
#21842 = B_SPLINE_CURVE_WITH_KNOTS ( 'NONE', 3,
 ( #22881, #35396, #7190, #13596 ),
 .UNSPECIFIED., .F., .F.,
 ( 4, 4 ),
 ( 8.673617379883999842E-19, 0.0003267947208782233685 ),
 .UNSPECIFIED. ) ;
#21843 = CARTESIAN_POINT ( 'NONE',  ( 0.06843411546424661707, -1.327640554429453168, 0.5682417262808774350 ) ) ;
#21844 = CARTESIAN_POINT ( 'NONE',  ( 0.3091361241754520539, -1.774399086135407533, 0.3157417262808776548 ) ) ;
#21845 = CARTESIAN_POINT ( 'NONE',  ( 0.4414599527244874033, -1.202236957499543069, 0.6968917936656464640 ) ) ;
#21846 = DIRECTION ( 'NONE',  ( 0.000000000000000000, 0.000000000000000000, 1.000000000000000000 ) ) ;
#21847 = DIRECTION ( 'NONE',  ( 0.7023080333803263242, 0.4054292351890085855, -0.5851414884483189249 ) ) ;
#21848 = CARTESIAN_POINT ( 'NONE',  ( 0.04575106512774684830, -0.2311453587453369818, 0.4288095618640354045 ) ) ;
#21849 = CARTESIAN_POINT ( 'NONE',  ( 0.002083146443013472390, -0.4777046557262296100, 0.1109577558998209867 ) ) ;
#21850 = CARTESIAN_POINT ( 'NONE',  ( 0.06667927146718531650, -1.148330793516402881, 0.7614259873238805598 ) ) ;
#21851 = APPROVAL_STATUS ( 'not_yet_approved' ) ;
#21852 = CARTESIAN_POINT ( 'NONE',  ( 0.3043431798205027405, -0.7811398438223191576, 0.6771279187310788039 ) ) ;
#21853 = AXIS2_PLACEMENT_3D ( 'NONE', #18135, #14420, #39327 ) ;
#21854 = EDGE_CURVE ( 'NONE', #19589, #9095, #24451, .T. ) ;
#21855 = CARTESIAN_POINT ( 'NONE',  ( -0.03643058821097221872, 0.4544345964805175386, 0.2356993163710971728 ) ) ;
#21856 = LINE ( 'NONE', #30893, #12302 ) ;
#21857 = EDGE_CURVE ( 'NONE', #9108, #20043, #37584, .T. ) ;
#21858 = CARTESIAN_POINT ( 'NONE',  ( 0.5538850894636544453, -1.624718492099754830, -0.5678182754891358819 ) ) ;
#21859 = CIRCLE ( 'NONE', #4095, 0.03749999999977554621 ) ;
#21860 = VECTOR ( 'NONE', #17379, 39.37007874015748143 ) ;
#21861 = DIRECTION ( 'NONE',  ( 1.000000000000000000, -7.000205099780415542E-17, -1.510243460696184374E-15 ) ) ;
#21862 = ORIENTED_EDGE ( 'NONE', *, *, #26344, .T. ) ;
#21863 = CARTESIAN_POINT ( 'NONE',  ( 0.4651649163319350189, -1.149540594742337607, -0.6230854793619403642 ) ) ;
#21864 = CARTESIAN_POINT ( 'NONE',  ( 0.2238418704740615384, -1.454669764064490778, 0.9245064154499356146 ) ) ;
#21865 = AXIS2_PLACEMENT_3D ( 'NONE', #24294, #15026, #27394 ) ;
#21866 = CARTESIAN_POINT ( 'NONE',  ( 0.5949972485239248821, -1.483920380426879682, 0.6302736613771389163 ) ) ;
#21868 = EDGE_LOOP ( 'NONE', ( #4638, #12762, #3926, #17882 ) ) ;
#21867 = CARTESIAN_POINT ( 'NONE',  ( 0.3486080135059020368, -1.166240872638638182, 0.4316577372902974941 ) ) ;
#21869 = CARTESIAN_POINT ( 'NONE',  ( 0.4727414870697744798, -1.078201156678013639, 0.7478468640933467748 ) ) ;
#21871 = ORIENTED_EDGE ( 'NONE', *, *, #930, .F. ) ;
#21870 = EDGE_LOOP ( 'NONE', ( #6208, #17965, #11592, #38000 ) ) ;
#21872 = CARTESIAN_POINT ( 'NONE',  ( 0.5737815958547760609, -1.229766092225264673, 0.8180618760404326784 ) ) ;
#21873 = CARTESIAN_POINT ( 'NONE',  ( 0.04293701532779490432, 0.4432143466407591492, -0.2195216604697225182 ) ) ;
#21874 = TOROIDAL_SURFACE ( 'NONE', #28432, 0.6154198107346402491, 0.7750185148639454624 ) ;
#21875 = DIRECTION ( 'NONE',  ( 1.000000000000000000, 0.000000000000000000, 0.000000000000000000 ) ) ;
#21876 = COORDINATED_UNIVERSAL_TIME_OFFSET ( 0, 0, .AHEAD. ) ;
#21877 = CARTESIAN_POINT ( 'NONE',  ( 0.3048982267989290840, -1.756746414302342796, 0.5594309555313056181 ) ) ;
#21878 = VERTEX_POINT ( 'NONE', #8805 ) ;
#21879 = ADVANCED_FACE ( 'NONE', ( #36773 ), #26349, .F. ) ;
#21880 = CARTESIAN_POINT ( 'NONE',  ( 0.1200857017990378389, -0.7890252880104620115, 0.4347573559404794841 ) ) ;
#21881 = CARTESIAN_POINT ( 'NONE',  ( 0.3677258932907612188, -1.634674973640408036, -0.3778581608314561802 ) ) ;
#21882 = CARTESIAN_POINT ( 'NONE',  ( 0.5104467154061602674, -1.495435902464579803, 0.7328012557383771775 ) ) ;
#21883 = EDGE_CURVE ( 'NONE', #1876, #24913, #36984, .T. ) ;
#21884 = CARTESIAN_POINT ( 'NONE',  ( 0.6291968284940171463, -1.616033820151582034, -0.4930595378406338880 ) ) ;
#21885 = CARTESIAN_POINT ( 'NONE',  ( -0.1642263571684470513, 0.5103503754387043179, 0.1528658435937215454 ) ) ;
#21886 = ORIENTED_EDGE ( 'NONE', *, *, #28710, .F. ) ;
#21887 = VECTOR ( 'NONE', #2855, 39.37007874015748854 ) ;
#21888 = DIRECTION ( 'NONE',  ( 0.000000000000000000, 0.000000000000000000, -1.000000000000000000 ) ) ;
#21889 = CARTESIAN_POINT ( 'NONE',  ( 0.7436037172534608608, -1.516441821114285382, 0.5740297838107625283 ) ) ;
#21890 = DIRECTION ( 'NONE',  ( 0.4999551463232372317, -0.8660512985181133550, 0.000000000000000000 ) ) ;
#21891 = CIRCLE ( 'NONE', #26457, 0.01500000000000001853 ) ;
#21892 = AXIS2_PLACEMENT_3D ( 'NONE', #11208, #1967, #36709 ) ;
#21893 = CARTESIAN_POINT ( 'NONE',  ( 0.5114126470110641476, -1.614748454822723556, -0.5166151207188711680 ) ) ;
#21894 = SHAPE_REPRESENTATION_RELATIONSHIP ( 'NONE' , 'NONE' ,  #40103, #5887 ) ;
#21895 = CONICAL_SURFACE ( 'NONE', #21241, 0.1600000000000007527, 1.047197551196599186 ) ;
#21896 = CARTESIAN_POINT ( 'NONE',  ( 0.2319960710055803677, -1.232736008543062090, 0.4687417262808780127 ) ) ;
#21897 = DIRECTION ( 'NONE',  ( 0.4999999999999991673, -0.1289820025937439552, -0.8563665354314752287 ) ) ;
#21898 = CARTESIAN_POINT ( 'NONE',  ( 0.0006292437964357017102, -0.9180166443092167006, 0.3683461522897012452 ) ) ;
#21899 = CARTESIAN_POINT ( 'NONE',  ( 0.5440395270977919084, -1.170651503450800268, 0.6371399293509031336 ) ) ;
#21900 = COORDINATED_UNIVERSAL_TIME_OFFSET ( 0, 0, .AHEAD. ) ;
#21901 = CARTESIAN_POINT ( 'NONE',  ( 0.5806656507430593139, -1.610816081966196078, 0.5908874216888502229 ) ) ;
#21902 = AXIS2_PLACEMENT_3D ( 'NONE', #25678, #35339, #22205 ) ;
#21903 = ADVANCED_FACE ( 'NONE', ( #27733 ), #40268, .F. ) ;
#21904 = CARTESIAN_POINT ( 'NONE',  ( 0.3870879061362800799, -1.718823008802655927, 0.4198165928321926366 ) ) ;
#21905 = CARTESIAN_POINT ( 'NONE',  ( -0.03672309138969667014, -0.04080728438229332816, 0.4790859898006363249 ) ) ;
#21906 = VERTEX_POINT ( 'NONE', #6514 ) ;
#21907 = CARTESIAN_POINT ( 'NONE',  ( 0.4775505920942409444, -1.133805584195902494, 0.4714299366448774786 ) ) ;
#21908 = CARTESIAN_POINT ( 'NONE',  ( -0.05464101615137770263, -2.177105168660885326, -0.3318349584362400018 ) ) ;
#21909 = VECTOR ( 'NONE', #3722, 39.37007874015748143 ) ;
#21910 = B_SPLINE_CURVE_WITH_KNOTS ( 'NONE', 3,
 ( #33461, #24425, #17828, #24037, #8166, #1620, #21135, #20745, #27512, #40035 ),
 .UNSPECIFIED., .F., .F.,
 ( 4, 2, 2, 2, 4 ),
 ( 0.000000000000000000, 0.0009922644452961607020, 0.001984528890592321404, 0.002976793335888482106, 0.003969057781184642808 ),
 .UNSPECIFIED. ) ;
#21911 = CARTESIAN_POINT ( 'NONE',  ( 0.1872551924900081322, -0.8472677374427307617, 0.2151649526408891677 ) ) ;
#21912 = ORIENTED_EDGE ( 'NONE', *, *, #1886, .F. ) ;
#21913 = CARTESIAN_POINT ( 'NONE',  ( -0.05615703521555036326, 0.01030498872321548333, -0.4592891699083767598 ) ) ;
#21914 = CARTESIAN_POINT ( 'NONE',  ( 0.1214394166101126354, -1.245726820615419062, 0.7465128526039198631 ) ) ;
#21916 = ORIENTED_EDGE ( 'NONE', *, *, #2660, .F. ) ;
#21915 = ORIENTED_EDGE ( 'NONE', *, *, #13178, .T. ) ;
#21917 = CARTESIAN_POINT ( 'NONE',  ( 0.1536596445529307131, -1.277574755431481579, 0.4245438548657216038 ) ) ;
#21918 = EDGE_LOOP ( 'NONE', ( #9517, #11324, #22755 ) ) ;
#21919 = FACE_OUTER_BOUND ( 'NONE', #24058, .T. ) ;
#21920 = CARTESIAN_POINT ( 'NONE',  ( 0.1890194704680109583, -1.936495776297340710, -0.3324113174558592787 ) ) ;
#21921 = DIRECTION ( 'NONE',  ( 0.000000000000000000, 0.000000000000000000, -1.000000000000000000 ) ) ;
#21923 = CARTESIAN_POINT ( 'NONE',  ( 0.2260509237186448805, -1.351684612934085372, 0.5412798235273647007 ) ) ;
#21922 = CARTESIAN_POINT ( 'NONE',  ( 0.01548846960707524721, -0.09061086148575756005, -0.5171215251571035232 ) ) ;
#21924 = CARTESIAN_POINT ( 'NONE',  ( 0.03170953572518930147, -0.2433677181033266079, -0.4274019581173345017 ) ) ;
#21925 = EDGE_LOOP ( 'NONE', ( #33322, #26362, #31481, #30630 ) ) ;
#21926 = CARTESIAN_POINT ( 'NONE',  ( 0.2629928857398323716, -0.9282033514108480876, 0.7349524644010387853 ) ) ;
#21927 = ORIENTED_EDGE ( 'NONE', *, *, #5363, .T. ) ;
#21928 = AXIS2_PLACEMENT_3D ( 'NONE', #12662, #16785, #29115 ) ;
#21929 = VERTEX_POINT ( 'NONE', #31836 ) ;
#21930 = DIRECTION ( 'NONE',  ( 0.8660512985181135770, 0.4999551463232370097, 0.000000000000000000 ) ) ;
#21931 = CARTESIAN_POINT ( 'NONE',  ( 0.07342862190203788830, -0.5555273798011833852, 0.2245834878394794565 ) ) ;
#21932 = CIRCLE ( 'NONE', #15984, 0.1249999999999999584 ) ;
#21934 = DIRECTION ( 'NONE',  ( -1.188678714063518030E-15, 1.000000000000000000, -3.676620095425087714E-16 ) ) ;
#21933 = CARTESIAN_POINT ( 'NONE',  ( 0.3374716419252246080, -1.644379157745376574, -0.6493782657834309413 ) ) ;
#21935 = DIRECTION ( 'NONE',  ( 2.465190328815661892E-32, 1.000000000000000000, 6.656013887802287108E-31 ) ) ;
#21936 = CARTESIAN_POINT ( 'NONE',  ( 0.1880425571213318880, -0.9154252179768241904, 0.1909967134266482292 ) ) ;
#21937 = EDGE_CURVE ( 'NONE', #3488, #16904, #28302, .T. ) ;
#21938 = LINE ( 'NONE', #18851, #6160 ) ;
#21939 = CARTESIAN_POINT ( 'NONE',  ( 0.2388414923709098747, -1.586845850796878121, -0.3224580823847754130 ) ) ;
#21940 = CARTESIAN_POINT ( 'NONE',  ( 0.1367236663606709313, -0.6234998906017088505, 0.3678473249437352322 ) ) ;
#21941 = CARTESIAN_POINT ( 'NONE',  ( 0.4876229533068589528, -1.660624946139342084, 0.5317207588342793834 ) ) ;
#21942 = FACE_OUTER_BOUND ( 'NONE', #27293, .T. ) ;
#21943 = DIRECTION ( 'NONE',  ( -1.416619696839555637E-11, 0.5877852522924655876, -0.8090169943749527803 ) ) ;
#21944 = FACE_BOUND ( 'NONE', #33927, .T. ) ;
#21945 = AXIS2_PLACEMENT_3D ( 'NONE', #6446, #16534, #943 ) ;
#21946 = DIRECTION ( 'NONE',  ( -7.000205099780496893E-17, -1.000000000000000000, -6.590151126658374952E-16 ) ) ;
#21947 = DIRECTION ( 'NONE',  ( 0.000000000000000000, -0.6645646360916347417, 0.7472307839325098566 ) ) ;
#21948 = B_SPLINE_CURVE_WITH_KNOTS ( 'NONE', 3,
 ( #25082, #28172, #5745, #9043 ),
 .UNSPECIFIED., .F., .F.,
 ( 4, 4 ),
 ( 3.324383805864000793E-17, 2.394154788142702125E-05 ),
 .UNSPECIFIED. ) ;
#21949 = CARTESIAN_POINT ( 'NONE',  ( 0.5297859054048726923, -1.159963375372088823, 0.8529160106009885389 ) ) ;
#21950 = CIRCLE ( 'NONE', #13384, 0.9237847906030155487 ) ;
#21951 = AXIS2_PLACEMENT_3D ( 'NONE', #36365, #23455, #17248 ) ;
#21952 = CARTESIAN_POINT ( 'NONE',  ( -0.05138886601528275949, 0.2952081121918923023, 0.3684218102521255589 ) ) ;
#21953 = CARTESIAN_POINT ( 'NONE',  ( 0.05954239774771610122, -1.330287657886653596, 0.5843365015712381760 ) ) ;
#21954 = DIRECTION ( 'NONE',  ( 8.881784197001246407E-16, -2.361472542561082612E-16, 1.000000000000000000 ) ) ;
#21955 = DIRECTION ( 'NONE',  ( -0.9107505893967028365, 0.000000000000000000, -0.4129568547845627324 ) ) ;
#21956 = CARTESIAN_POINT ( 'NONE',  ( 0.1898061597842229664, -0.8838521600963774594, 0.6041132961182806849 ) ) ;
#21957 = CARTESIAN_POINT ( 'NONE',  ( 0.06972317538281022631, -1.315496003368490152, 0.5114807970970258744 ) ) ;
#21958 = CARTESIAN_POINT ( 'NONE',  ( 0.6047538891612445067, -1.605163873594933843, 0.4396382108053981108 ) ) ;
#21959 = CIRCLE ( 'NONE', #23259, 1.986674066779353875 ) ;
#21960 = EDGE_LOOP ( 'NONE', ( #31109, #14725, #28240, #34082 ) ) ;
#21961 = CARTESIAN_POINT ( 'NONE',  ( -0.2746410161513779258, -3.291368864184588183, -0.6988176298300771139 ) ) ;
#21962 = CARTESIAN_POINT ( 'NONE',  ( 0.3336325236675090067, -1.050835064020409160, 0.7593003920438236021 ) ) ;
#21963 = CARTESIAN_POINT ( 'NONE',  ( 0.3641313327837605307, -1.992291791370100373, -0.5052991671685238551 ) ) ;
#21964 = DIRECTION ( 'NONE',  ( 1.000000000000000000, 0.000000000000000000, 0.000000000000000000 ) ) ;
#21965 = CARTESIAN_POINT ( 'NONE',  ( 0.3696433192220597852, -2.076078244643423609, -0.4731903481153287849 ) ) ;
#21966 = ORIENTED_EDGE ( 'NONE', *, *, #32337, .F. ) ;
#21967 = CARTESIAN_POINT ( 'NONE',  ( 0.3927971208821917082, -1.752502930713592200, -0.5454495665901371027 ) ) ;
#21968 = DIRECTION ( 'NONE',  ( 1.654489825136704222E-31, -0.9510565162951546414, -0.3090169943749438985 ) ) ;
#21969 = CARTESIAN_POINT ( 'NONE',  ( 0.07135087575717259656, -1.325947744100555603, 0.5536768997389298619 ) ) ;
#21970 = LINE ( 'NONE', #3043, #307 ) ;
#21971 = AXIS2_PLACEMENT_3D ( 'NONE', #32865, #8184, #39447 ) ;
#21972 = CARTESIAN_POINT ( 'NONE',  ( 0.3632587558834509123, -1.098712390806521499, 0.7441976441039135359 ) ) ;
#21974 = EDGE_LOOP ( 'NONE', ( #15598, #23510, #6255, #20542 ) ) ;
#21973 = CARTESIAN_POINT ( 'NONE',  ( -0.02000000000000000042, -2.198867511061768809, -0.9423512173156428640 ) ) ;
#21975 = CARTESIAN_POINT ( 'NONE',  ( 0.4813782568983027699, -1.076368431653871971, 0.6093178202591913450 ) ) ;
#21976 = ORIENTED_EDGE ( 'NONE', *, *, #30675, .T. ) ;
#21977 = CALENDAR_DATE ( 2026, 13, 10 ) ;
#21978 = CARTESIAN_POINT ( 'NONE',  ( 0.01358700006623634465, -0.9214419153559146869, 0.5592488618034630043 ) ) ;
#21979 = ORIENTED_EDGE ( 'NONE', *, *, #12355, .F. ) ;
#21980 = CIRCLE ( 'NONE', #10125, 0.09999999999999999167 ) ;
#21981 = VECTOR ( 'NONE', #31008, 39.37007874015748143 ) ;
#21982 = CARTESIAN_POINT ( 'NONE',  ( 0.3852639964463288047, -1.605627256116679336, 0.5745209014822190152 ) ) ;
#21984 = CARTESIAN_POINT ( 'NONE',  ( 0.1853660027032721369, -0.7908266843905505938, 0.01465295923235358268 ) ) ;
#21983 = DIRECTION ( 'NONE',  ( -7.000205099780314469E-17, -1.000000000000000000, 6.590151126658399604E-16 ) ) ;
#21985 = DIRECTION ( 'NONE',  ( -0.7432310347629357272, -0.4120354308901564844, 0.5271000214915373405 ) ) ;
#21986 = LOCAL_TIME ( 0, 53, 7.000000000000000000, #10700 ) ;
#21987 = EDGE_LOOP ( 'NONE', ( #13906, #38494, #31256, #33384 ) ) ;
#21988 = ORIENTED_EDGE ( 'NONE', *, *, #32755, .F. ) ;
#21989 = EDGE_LOOP ( 'NONE', ( #22518, #32622, #21976, #31516, #35374, #29695, #4739 ) ) ;
#21990 = CARTESIAN_POINT ( 'NONE',  ( 0.3426012929402474372, -0.9387369744000205740, 0.6409010290876834270 ) ) ;
#21991 = EDGE_CURVE ( 'NONE', #20248, #36967, #13175, .T. ) ;
#21992 = CARTESIAN_POINT ( 'NONE',  ( 0.5097106194861918960, -1.415068235197837199, 0.7887110192874389192 ) ) ;
#21993 = ORIENTED_EDGE ( 'NONE', *, *, #30750, .F. ) ;
#21994 = CIRCLE ( 'NONE', #21343, 0.1050228153667111808 ) ;
#21995 = CARTESIAN_POINT ( 'NONE',  ( 0.1873082927213247373, -0.6998484496557862977, 0.03162329823462053241 ) ) ;
#21996 = CARTESIAN_POINT ( 'NONE',  ( -0.001553869254396566353, -1.875183443470214151, -0.3468731710442038985 ) ) ;
#21997 = EDGE_CURVE ( 'NONE', #8795, #17394, #34878, .T. ) ;
#21998 = CARTESIAN_POINT ( 'NONE',  ( 0.6118202138478362473, -1.459615948755139003, -0.6250000000000000000 ) ) ;
#21999 = CARTESIAN_POINT ( 'NONE',  ( -0.01548846960712776770, 0.5203207976466729390, -0.08861466064782422269 ) ) ;
#22000 = EDGE_CURVE ( 'NONE', #26316, #1752, #35504, .T. ) ;
#22001 = CARTESIAN_POINT ( 'NONE',  ( 0.2999999999999784506, -1.937578511955589278, -0.3171235303465976818 ) ) ;
#22002 = ADVANCED_FACE ( 'NONE', ( #6927 ), #5863, .F. ) ;
#22003 = CARTESIAN_POINT ( 'NONE',  ( -0.01210526301015784831, 0.06117178301711245075, 0.1249999999999993894 ) ) ;
#22004 = DIRECTION ( 'NONE',  ( 0.000000000000000000, 3.414809992080312950E-15, -1.000000000000000000 ) ) ;
#22005 = CARTESIAN_POINT ( 'NONE',  ( 0.2106403741462083423, -1.241433952965754539, 0.5874914036943872375 ) ) ;
#22006 = CARTESIAN_POINT ( 'NONE',  ( 0.0009544144440424411633, -1.789965111182992175, -0.6370759315579171966 ) ) ;
#22007 = CARTESIAN_POINT ( 'NONE',  ( 0.08492870897506230032, -1.322602396236127520, 0.7244794688457697474 ) ) ;
#22008 = PERSON_AND_ORGANIZATION_ROLE ( 'creator' ) ;
#22009 = AXIS2_PLACEMENT_3D ( 'NONE', #37086, #15075, #14879 ) ;
#22010 = CARTESIAN_POINT ( 'NONE',  ( 0.4508097189255980131, -1.059596525805123202, 0.6314750327306427602 ) ) ;
#22011 = AXIS2_PLACEMENT_3D ( 'NONE', #3013, #36740, #39835 ) ;
#22012 = CARTESIAN_POINT ( 'NONE',  ( 0.1838304123260658118, -1.376269861257182203, 0.4854672772329559072 ) ) ;
#22013 = CARTESIAN_POINT ( 'NONE',  ( 0.4857959727310743325, -1.202259978777793226, 0.5856983068965045947 ) ) ;
#22014 = DIRECTION ( 'NONE',  ( 0.000000000000000000, 0.9246857012436752177, -0.3807313408632033713 ) ) ;
#22015 = VECTOR ( 'NONE', #17071, 39.37007874015748143 ) ;
#22016 = AXIS2_PLACEMENT_3D ( 'NONE', #11641, #21316, #24388 ) ;
#22017 = EDGE_CURVE ( 'NONE', #7249, #38394, #29128, .T. ) ;
#22018 = PRODUCT_DEFINITION_FORMATION_WITH_SPECIFIED_SOURCE ( 'ANY', '', #27114, .NOT_KNOWN. ) ;
#22019 = APPROVAL ( #15518, 'UNSPECIFIED' ) ;
#22020 = CARTESIAN_POINT ( 'NONE',  ( -0.003124719664520040317, -0.8057675726412020234, 0.1293934913668264852 ) ) ;
#22021 = CARTESIAN_POINT ( 'NONE',  ( -0.0001502531655640915837, -0.8192210497105464340, -0.06580348057302833065 ) ) ;
#22022 = DIRECTION ( 'NONE',  ( -1.000000000000000000, -2.280301054154495132E-31, 1.664003471950577689E-31 ) ) ;
#22023 = CARTESIAN_POINT ( 'NONE',  ( 0.3338768636023082270, -1.636289205640462541, 0.4854925386805667986 ) ) ;
#22024 = AXIS2_PLACEMENT_3D ( 'NONE', #12933, #38018, #35139 ) ;
#22025 = ORIENTED_EDGE ( 'NONE', *, *, #4613, .T. ) ;
#22026 = ORIENTED_EDGE ( 'NONE', *, *, #27106, .T. ) ;
#22027 = CARTESIAN_POINT ( 'NONE',  ( 0.05283710938261026308, -0.2421875768565588671, -0.4008269984734638691 ) ) ;
#22028 = ORIENTED_EDGE ( 'NONE', *, *, #17013, .F. ) ;
#22029 = CARTESIAN_POINT ( 'NONE',  ( 0.03113248654051816583, -0.3165425539888620521, -0.4137570037148034507 ) ) ;
#22030 = CARTESIAN_POINT ( 'NONE',  ( 0.03868649100028130616, 0.2522293598345318744, 0.4043344736883378032 ) ) ;
#22031 = CARTESIAN_POINT ( 'NONE',  ( 0.5974902904423020633, -1.460252601885912327, 0.6227098129790233916 ) ) ;
#22033 = ORIENTED_EDGE ( 'NONE', *, *, #22971, .T. ) ;
#22032 = CARTESIAN_POINT ( 'NONE',  ( 0.002302760697785899424, -0.5199223015690960237, 0.1489253775790380097 ) ) ;
#22034 = VERTEX_POINT ( 'NONE', #5666 ) ;
#22035 = CARTESIAN_POINT ( 'NONE',  ( 0.2033348128484126494, -0.6878582300498709001, 0.3466453153493967432 ) ) ;
#22036 = ORIENTED_EDGE ( 'NONE', *, *, #27113, .F. ) ;
#22037 = CARTESIAN_POINT ( 'NONE',  ( 0.03806478327246554799, -0.7058754152494622902, 0.5484913812544711664 ) ) ;
#22039 = DIRECTION ( 'NONE',  ( -1.000000000000000000, -0.000000000000000000, -0.000000000000000000 ) ) ;
#22038 = CARTESIAN_POINT ( 'NONE',  ( 0.3862110256088818194, -1.731934476144515900, 0.4282538419479027247 ) ) ;
#22040 = CARTESIAN_POINT ( 'NONE',  ( 0.2927350798623002959, -1.544518291098198715, -0.6925464747855896164 ) ) ;
#22041 = DIRECTION ( 'NONE',  ( -6.106226635438322318E-15, 2.142487232963740814E-14, 1.000000000000000000 ) ) ;
#22042 = AXIS2_PLACEMENT_3D ( 'NONE', #13364, #22041, #19555 ) ;
#22043 = CARTESIAN_POINT ( 'NONE',  ( -0.1212602504878781962, -0.5073146173917492119, 0.3032895567580783380 ) ) ;
#22045 = ORIENTED_EDGE ( 'NONE', *, *, #34025, .T. ) ;
#22044 = ORIENTED_EDGE ( 'NONE', *, *, #12763, .F. ) ;
#22046 = AXIS2_PLACEMENT_3D ( 'NONE', #11194, #7485, #36085 ) ;
#22047 = CARTESIAN_POINT ( 'NONE',  ( 0.1499999999999996059, -0.3232818887608613356, -0.4449593469062207429 ) ) ;
#22048 = FACE_OUTER_BOUND ( 'NONE', #22330, .T. ) ;
#22049 = CARTESIAN_POINT ( 'NONE',  ( -0.02881302694830086691, -0.4889319715862793791, 0.09562644460326608087 ) ) ;
#22050 = AXIS2_PLACEMENT_3D ( 'NONE', #32615, #32403, #7094 ) ;
#22051 = EDGE_CURVE ( 'NONE', #13521, #1646, #3981, .T. ) ;
#22052 = CARTESIAN_POINT ( 'NONE',  ( 0.5832544884196250168, -1.433562627639882292, 0.6981186852435199430 ) ) ;
#22053 = CARTESIAN_POINT ( 'NONE',  ( 0.1499999999999996336, -0.09319974324249266640, -0.5318964258758781538 ) ) ;
#22054 = LOCAL_TIME ( 0, 53, 7.000000000000000000, #16733 ) ;
#22055 = CARTESIAN_POINT ( 'NONE',  ( 0.03113248654051816583, -0.4415087982045245996, -0.1343585914930097158 ) ) ;
#22056 = EDGE_CURVE ( 'NONE', #26023, #39166, #27175, .T. ) ;
#22057 = CARTESIAN_POINT ( 'NONE',  ( 0.01378518146509891129, -0.4682930211632502782, 0.3166968367138670026 ) ) ;
#22058 = EDGE_CURVE ( 'NONE', #1527, #26316, #13878, .T. ) ;
#22059 = CONICAL_SURFACE ( 'NONE', #14810, 0.1500000000000011324, 1.047197551196599630 ) ;
#22060 = CARTESIAN_POINT ( 'NONE',  ( 0.4688459138424372341, -1.061988423737608045, -0.4248180574663140141 ) ) ;
#22061 = CARTESIAN_POINT ( 'NONE',  ( 0.3034770402916767695, -1.538524164614652578, -0.7285408748657138389 ) ) ;
#22062 = CARTESIAN_POINT ( 'NONE',  ( 0.4590722942007692264, -1.224561879564241673, 0.6545337212731852095 ) ) ;
#22063 = CARTESIAN_POINT ( 'NONE',  ( 0.4173046189016191287, -1.738355212467242561, -0.5155029497116575543 ) ) ;
#22064 = CARTESIAN_POINT ( 'NONE',  ( 0.05201782277453730063, -0.2909620873304541444, 0.3697179445082250382 ) ) ;
#22065 = CARTESIAN_POINT ( 'NONE',  ( 0.3165138724069220255, -1.757609964495261190, 0.6990733182572979043 ) ) ;
#22066 = PRODUCT_DEFINITION_CONTEXT ( 'detailed design', #16635, 'design' ) ;
#22067 = CARTESIAN_POINT ( 'NONE',  ( 0.09763382290327969615, -1.358444063574388183, 0.6820618144092522872 ) ) ;
#22068 = COORDINATED_UNIVERSAL_TIME_OFFSET ( 0, 0, .AHEAD. ) ;
#22069 = ADVANCED_FACE ( 'NONE', ( #18011 ), #20417, .T. ) ;
#22070 = CARTESIAN_POINT ( 'NONE',  ( -0.05076679145662017084, 0.4330939261214903357, 0.1921033382362740127 ) ) ;
#22071 = AXIS2_PLACEMENT_3D ( 'NONE', #26050, #13274, #22953 ) ;
#22072 = CARTESIAN_POINT ( 'NONE',  ( 0.6990213974170155220, -1.529262631747053902, 0.5876538509318743886 ) ) ;
#22073 = DIRECTION ( 'NONE',  ( -0.000000000000000000, 0.7071067811865474617, 0.7071067811865474617 ) ) ;
#22074 = DIRECTION ( 'NONE',  ( -0.4697114767686432213, -0.8828199865158355975, 0.000000000000000000 ) ) ;
#22075 = ORIENTED_EDGE ( 'NONE', *, *, #38058, .T. ) ;
#22076 = CARTESIAN_POINT ( 'NONE',  ( 0.4640112847229192483, -1.150115029303059089, -0.4078508934533979780 ) ) ;
#22077 = SECURITY_CLASSIFICATION ( '', '', #40480 ) ;
#22078 = CARTESIAN_POINT ( 'NONE',  ( 0.2194110478981629864, -1.459085012964730810, 0.9363139587045151702 ) ) ;
#22079 = CARTESIAN_POINT ( 'NONE',  ( 0.5946750165716045977, -1.487132221806371390, 0.5679954418029664609 ) ) ;
#22080 = B_SPLINE_CURVE_WITH_KNOTS ( 'NONE', 3,
 ( #15884, #1102, #32126, #13403, #16698, #9906, #303, #517, #23084, #7025, #13010, #3930, #25558, #19590, #38505, #32311, #29246, #13610, #14003, #20198, #36425, #17299, #23896, #13796, #29643, #26361, #4943, #4530, #32521, #1483, #39306, #8236, #24107, #32920, #1289, #30057, #7411, #1694, #32723, #36212, #39496, #11325, #10939, #38893, #26963, #10723, #14604, #7821, #11127, #11545, #23500, #20813 ),
 .UNSPECIFIED., .F., .F.,
 ( 4, 2, 2, 2, 2, 2, 2, 2, 2, 2, 2, 2, 2, 2, 2, 2, 2, 2, 2, 2, 2, 2, 2, 2, 2, 4 ),
 ( 0.001215176597727166043, 0.002640180933026298367, 0.003352683100675868649, 0.004065185268325438930, 0.005490189603624587300, 0.006915193938923737405, 0.008340198274222885774, 0.009052700441872457357, 0.009765202609522028940, 0.01119020694482118945, 0.01261521128012034997, 0.01546521995071867446, 0.01689022428601783324, 0.01831522862131699722, 0.02116523729191532519, 0.02401524596251365662, 0.02686525463311198805, 0.02971526330371031602, 0.03256527197430864745, 0.03541528064490696848, 0.03684028498020613940, 0.03826528931550530338, 0.04111529798610363828, 0.04254030232140279533, 0.04396530665670195931, 0.04681531532730028033 ),
 .UNSPECIFIED. ) ;
#22082 = EDGE_LOOP ( 'NONE', ( #22734, #35611, #5792, #35479 ) ) ;
#22081 = CARTESIAN_POINT ( 'NONE',  ( 0.5473076987003111515, -1.651760216406904513, -0.4929644493450987541 ) ) ;
#22083 = CIRCLE ( 'NONE', #24077, 0.04330708661417336652 ) ;
#22084 = ADVANCED_FACE ( 'NONE', ( #11649 ), #31184, .F. ) ;
#22085 = CARTESIAN_POINT ( 'NONE',  ( 0.3991878447057942703, -0.9797369418029474586, 0.7176166460480870590 ) ) ;
#22087 = EDGE_LOOP ( 'NONE', ( #38905, #2444, #22086, #10029 ) ) ;
#22086 = ORIENTED_EDGE ( 'NONE', *, *, #933, .F. ) ;
#22088 = CARTESIAN_POINT ( 'NONE',  ( 0.1909286924077255587, -1.257064795538239466, -0.7137159211901569211 ) ) ;
#22089 = CARTESIAN_POINT ( 'NONE',  ( 0.3393515303230732472, -1.642456816116736107, -0.5888195431444244177 ) ) ;
#22090 = B_SPLINE_CURVE_WITH_KNOTS ( 'NONE', 3,
 ( #15805, #24464, #27961, #31036 ),
 .UNSPECIFIED., .F., .F.,
 ( 4, 4 ),
 ( 0.000000000000000000, 0.001818400350217978497 ),
 .UNSPECIFIED. ) ;
#22091 = DIRECTION ( 'NONE',  ( -8.881784197001246407E-16, 2.361472542561082612E-16, -1.000000000000000000 ) ) ;
#22092 = DATE_TIME_ROLE ( 'classification_date' ) ;
#22093 = DIRECTION ( 'NONE',  ( -0.8660254037844384856, 1.232595164407831384E-31, 0.5000000000000004441 ) ) ;
#22094 = ORIENTED_EDGE ( 'NONE', *, *, #28191, .T. ) ;
#22095 = CARTESIAN_POINT ( 'NONE',  ( 0.08744249762914983737, -0.7479857328945178629, 0.2113153514082470319 ) ) ;
#22096 = CARTESIAN_POINT ( 'NONE',  ( 0.1909286924077255032, -1.257064795538239022, -0.4400554600884079015 ) ) ;
#22097 = CARTESIAN_POINT ( 'NONE',  ( 0.1038539065874188316, -0.5467874247544137756, 0.1622444650650389786 ) ) ;
#22098 = CARTESIAN_POINT ( 'NONE',  ( 0.5767571638091754105, -1.611000162511842415, -0.5470636458226728616 ) ) ;
#22099 = DIRECTION ( 'NONE',  ( -1.000000000000000000, -0.000000000000000000, -0.000000000000000000 ) ) ;
#22100 = ORIENTED_EDGE ( 'NONE', *, *, #18593, .T. ) ;
#22101 = EDGE_CURVE ( 'NONE', #24018, #4341, #37949, .T. ) ;
#22102 = CARTESIAN_POINT ( 'NONE',  ( 0.4224071670835765624, -1.711981311311245646, 0.6086670734470306376 ) ) ;
#22103 = AXIS2_PLACEMENT_3D ( 'NONE', #23190, #11436, #7918 ) ;
#22104 = CARTESIAN_POINT ( 'NONE',  ( 0.6657490759106345912, -1.561538255549536736, 0.5663076794875994135 ) ) ;
#22105 = VECTOR ( 'NONE', #35379, 39.37007874015748854 ) ;
#22106 = LINE ( 'NONE', #19198, #22689 ) ;
#22107 = CARTESIAN_POINT ( 'NONE',  ( 0.1361552210536516039, -0.5798312371597438286, 0.2613271312737237007 ) ) ;
#22108 = CARTESIAN_POINT ( 'NONE',  ( 0.04582889109739183425, -0.4790149006698671830, 0.08746027838083611505 ) ) ;
#22109 = APPLIED_SECURITY_CLASSIFICATION_ASSIGNMENT ( #39812, ( #40655 ) ) ;
#22110 = EDGE_CURVE ( 'NONE', #23675, #22635, #12444, .T. ) ;
#22111 = CARTESIAN_POINT ( 'NONE',  ( 0.05563540667800927902, -1.335270441939011121, 0.5197417262808780025 ) ) ;
#22112 = CARTESIAN_POINT ( 'NONE',  ( 0.08978098643734198914, 0.000000000000000000, 0.000000000000000000 ) ) ;
#22113 = CIRCLE ( 'NONE', #29344, 0.1946589359789743512 ) ;
#22114 = CARTESIAN_POINT ( 'NONE',  ( 0.03852435536883173223, -1.195394391876414719, 0.6677169776219902264 ) ) ;
#22115 = CARTESIAN_POINT ( 'NONE',  ( 0.2858575041057334065, -0.8891697324286316206, 0.5691962326423758434 ) ) ;
#22116 = ADVANCED_BREP_SHAPE_REPRESENTATION ( '', ( #31982, #27819 ), #20008 ) ;
#22117 = APPROVAL_DATE_TIME ( #19206, #6886 ) ;
#22118 = CARTESIAN_POINT ( 'NONE',  ( -0.2300000000000005651, 0.5182417262804733804, 0.08500000000000004774 ) ) ;
#22119 = EDGE_CURVE ( 'NONE', #39497, #1588, #19130, .T. ) ;
#22120 = ORIENTED_EDGE ( 'NONE', *, *, #24063, .T. ) ;
#22121 = ADVANCED_FACE ( 'NONE', ( #11837 ), #19761, .T. ) ;
#22122 = CARTESIAN_POINT ( 'NONE',  ( 0.5140974934605563318, -1.532472854630404946, 0.5610796881895311339 ) ) ;
#22123 = CARTESIAN_POINT ( 'NONE',  ( -0.04575334816097881979, 0.06504672743687374414, 0.4827724779829230539 ) ) ;
#22124 = ORIENTED_EDGE ( 'NONE', *, *, #18860, .F. ) ;
#22125 = CARTESIAN_POINT ( 'NONE',  ( 0.3572222731481287661, -1.622781385286526934, -0.3671481750039431446 ) ) ;
#22126 = DIRECTION ( 'NONE',  ( -0.4999551463232359549, 0.8660512985181140211, 0.000000000000000000 ) ) ;
#22127 = CARTESIAN_POINT ( 'NONE',  ( 0.1906473341773986807, -0.8225591132712883891, 0.2611071221664287845 ) ) ;
#22128 = ORIENTED_EDGE ( 'NONE', *, *, #30517, .T. ) ;
#22129 = VECTOR ( 'NONE', #5075, 39.37007874015748143 ) ;
#22130 = CARTESIAN_POINT ( 'NONE',  ( 0.2316917763911649497, -1.232208891764917880, 0.5707417262808780478 ) ) ;
#22131 = CARTESIAN_POINT ( 'NONE',  ( 0.03213308919446983269, -1.082564143163080805, 0.7440698363395104042 ) ) ;
#22133 = ORIENTED_EDGE ( 'NONE', *, *, #34048, .F. ) ;
#22132 = ORIENTED_EDGE ( 'NONE', *, *, #16235, .T. ) ;
#22134 = CYLINDRICAL_SURFACE ( 'NONE', #19211, 0.03749999999977557397 ) ;
#22135 = DIRECTION ( 'NONE',  ( -0.4999551463232372317, 0.8660512985181135770, -0.000000000000000000 ) ) ;
#22136 = ADVANCED_FACE ( 'NONE', ( #20884 ), #2191, .T. ) ;
#22137 = CARTESIAN_POINT ( 'NONE',  ( 0.3571444853020102617, -1.839383662986079138, -0.5196660627627504025 ) ) ;
#22139 = DIRECTION ( 'NONE',  ( 0.000000000000000000, 0.000000000000000000, 1.000000000000000000 ) ) ;
#22138 = LINE ( 'NONE', #15930, #20684 ) ;
#22140 = DIRECTION ( 'NONE',  ( 1.000000000000000000, 1.138269997360102476E-15, -8.881784197001243449E-16 ) ) ;
#22141 = VERTEX_POINT ( 'NONE', #8960 ) ;
#22142 = CARTESIAN_POINT ( 'NONE',  ( 0.05999999999999990757, 0.7171888913565960255, -0.2950238883388468514 ) ) ;
#22143 = ORIENTED_EDGE ( 'NONE', *, *, #7708, .F. ) ;
#22144 = CIRCLE ( 'NONE', #4373, 0.2500000000000000000 ) ;
#22145 = CARTESIAN_POINT ( 'NONE',  ( 0.09046525539546303174, -0.5659545125636742391, 0.1933820889497062101 ) ) ;
#22146 = ORIENTED_EDGE ( 'NONE', *, *, #22762, .T. ) ;
#22147 = CARTESIAN_POINT ( 'NONE',  ( 0.6630839938131345423, -1.446213159395746128, -0.6155857397476032222 ) ) ;
#22148 = CARTESIAN_POINT ( 'NONE',  ( 0.07284975538018015340, -0.5413571526563850655, 0.1629110515435110984 ) ) ;
#22150 = DIRECTION ( 'NONE',  ( 1.000000000000000000, 1.441651681710401470E-15, -8.317221240636930495E-16 ) ) ;
#22149 = CARTESIAN_POINT ( 'NONE',  ( 0.5412176055846257272, -1.597081727404586093, -0.4604589859954540398 ) ) ;
#22151 = CARTESIAN_POINT ( 'NONE',  ( 0.4112193008909481584, -1.591609915475934889, -0.6177460231409163116 ) ) ;
#22152 = CARTESIAN_POINT ( 'NONE',  ( 0.2233957848829526416, -0.9348223186165968146, 0.4130400850522266687 ) ) ;
#22153 = EDGE_CURVE ( 'NONE', #26023, #23035, #7256, .T. ) ;
#22154 = CARTESIAN_POINT ( 'NONE',  ( 0.1399999999999994582, 0.000000000000000000, 0.000000000000000000 ) ) ;
#22155 = CARTESIAN_POINT ( 'NONE',  ( 0.1897112079047663935, -0.5340520988485693010, 0.1365881794216592948 ) ) ;
#22156 = CARTESIAN_POINT ( 'NONE',  ( 0.1255523023994105369, -0.5499328071996130163, 0.1534195410746523047 ) ) ;
#22157 = CARTESIAN_POINT ( 'NONE',  ( -0.04230258372739908318, 0.2720195588163330513, -0.3815939145425404355 ) ) ;
#22158 = CARTESIAN_POINT ( 'NONE',  ( -0.1399999999999997358, 4.857225732735056783E-17, 0.1250000000000000000 ) ) ;
#22159 = CARTESIAN_POINT ( 'NONE',  ( -0.2746410161513782033, -1.891808285041389093, -0.4498908273618595910 ) ) ;
#22160 = CARTESIAN_POINT ( 'NONE',  ( 0.07039376183350297411, -0.5541924008705879645, 0.2222877572371358135 ) ) ;
#22161 = DIRECTION ( 'NONE',  ( 0.000000000000000000, 0.8063205929144885431, -0.5914787413272156735 ) ) ;
#22162 = B_SPLINE_CURVE_WITH_KNOTS ( 'NONE', 3,
 ( #2526, #14868, #27428, #27616 ),
 .UNSPECIFIED., .F., .F.,
 ( 4, 4 ),
 ( 1.309687503460227108E-17, 0.0002394164927460790192 ),
 .UNSPECIFIED. ) ;
#22163 = AXIS2_PLACEMENT_3D ( 'NONE', #18191, #14091, #39199 ) ;
#22164 = CARTESIAN_POINT ( 'NONE',  ( 0.5016144086874707586, -1.117686766064061255, 0.8075564334577929326 ) ) ;
#22165 = CARTESIAN_POINT ( 'NONE',  ( -0.04140212552917726246, 0.2901315858634238576, 0.3705031754532664423 ) ) ;
#22166 = CARTESIAN_POINT ( 'NONE',  ( 0.04593167833806930528, -1.243000510969585415, 0.6581084539110385601 ) ) ;
#22167 = B_SPLINE_CURVE_WITH_KNOTS ( 'NONE', 3,
 ( #8204, #11509, #1856, #36181 ),
 .UNSPECIFIED., .F., .F.,
 ( 4, 4 ),
 ( 0.000000000000000000, 0.0002765389585800600018 ),
 .UNSPECIFIED. ) ;
#22168 = CARTESIAN_POINT ( 'NONE',  ( 0.6328450409950655553, -1.528231567268848234, -0.4195382387927960588 ) ) ;
#22169 = DIRECTION ( 'NONE',  ( 1.000000000000000000, 0.000000000000000000, 0.000000000000000000 ) ) ;
#22170 = CARTESIAN_POINT ( 'NONE',  ( 0.1207196391192309343, -0.8326872279821241341, 0.4345446219756442519 ) ) ;
#22171 = CARTESIAN_POINT ( 'NONE',  ( 0.06955161396059786338, -1.315588549135835894, 0.5148643997387302162 ) ) ;
#22172 = CARTESIAN_POINT ( 'NONE',  ( 0.01548846960707524721, 0.5198120922912040642, 0.07362328916749247276 ) ) ;
#22173 = EDGE_LOOP ( 'NONE', ( #31720, #14153, #37019, #1832 ) ) ;
#22174 = FACE_OUTER_BOUND ( 'NONE', #5105, .T. ) ;
#22175 = CARTESIAN_POINT ( 'NONE',  ( 0.3830941788893716948, -1.614634721936343498, -0.3633953494663126893 ) ) ;
#22176 = CARTESIAN_POINT ( 'NONE',  ( 0.3641400453962177486, -1.992249701587664790, -0.4900924681091965440 ) ) ;
#22177 = CARTESIAN_POINT ( 'NONE',  ( 0.5508559616054408137, -1.661258531014996986, -0.4933326546058601214 ) ) ;
#22178 = FACE_OUTER_BOUND ( 'NONE', #345, .T. ) ;
#22179 = ORIENTED_EDGE ( 'NONE', *, *, #37220, .T. ) ;
#22180 = CARTESIAN_POINT ( 'NONE',  ( 0.5399038930177494366, -1.667580954481910904, -0.5371941175943450997 ) ) ;
#22181 = CARTESIAN_POINT ( 'NONE',  ( 0.3316311659535515766, -1.291330680059900260, 0.4674458267467086481 ) ) ;
#22182 = CARTESIAN_POINT ( 'NONE',  ( -0.2399999999999999079, -3.849534981189179028, -0.1910928155360645808 ) ) ;
#22183 = CARTESIAN_POINT ( 'NONE',  ( 0.04285640132274361885, 0.2295067898340935886, -0.4383690285535431497 ) ) ;
#22184 = CARTESIAN_POINT ( 'NONE',  ( 0.5066646123182778627, -1.303543819055811515, 0.6363843823558122947 ) ) ;
#22186 = CARTESIAN_POINT ( 'NONE',  ( 0.3806788393426449035, -1.717835445135155625, 0.4208877479360482732 ) ) ;
#22185 = DIRECTION ( 'NONE',  ( 0.4999551463232373427, -0.8660512985181134660, 0.000000000000000000 ) ) ;
#22187 = CARTESIAN_POINT ( 'NONE',  ( 0.4579382962256918765, -1.063507731091402952, 0.6287285752299462960 ) ) ;
#22188 = ORIENTED_EDGE ( 'NONE', *, *, #28234, .T. ) ;
#22189 = CALENDAR_DATE ( 2026, 13, 10 ) ;
#22190 =( REPRESENTATION_RELATIONSHIP ('NONE','NONE', #27514, #33020 ) REPRESENTATION_RELATIONSHIP_WITH_TRANSFORMATION ( #17565 )SHAPE_REPRESENTATION_RELATIONSHIP( ) );
#22191 = DIRECTION ( 'NONE',  ( -7.000205099780314469E-17, -1.000000000000000000, 6.590151126658399604E-16 ) ) ;
#22192 = ORIENTED_EDGE ( 'NONE', *, *, #5671, .F. ) ;
#22193 = CARTESIAN_POINT ( 'NONE',  ( 0.3615071206352756805, -1.531905561232253188, 0.8175632647814430332 ) ) ;
#22195 = CARTESIAN_POINT ( 'NONE',  ( 0.1861028475561006812, -0.7105372532307299149, -0.02003343372011650789 ) ) ;
#22194 = CARTESIAN_POINT ( 'NONE',  ( 0.08634205943466652378, -0.7634307173544517822, 0.04861706834207135675 ) ) ;
#22196 = FACE_OUTER_BOUND ( 'NONE', #18365, .T. ) ;
#22197 = ORIENTED_EDGE ( 'NONE', *, *, #4728, .T. ) ;
#22198 = CARTESIAN_POINT ( 'NONE',  ( -0.1196601186823882668, -0.4996350631411420884, 0.1296977380670712998 ) ) ;
#22199 = CARTESIAN_POINT ( 'NONE',  ( 0.5672310176675520177, -1.503268715516413945, 0.5784013901591326112 ) ) ;
#22200 = VERTEX_POINT ( 'NONE', #24611 ) ;
#22201 = CARTESIAN_POINT ( 'NONE',  ( 0.1868122149958911793, -0.7339159750268756666, 0.03456946681538086014 ) ) ;
#22202 = DIRECTION ( 'NONE',  ( 0.000000000000000000, 0.000000000000000000, -1.000000000000000000 ) ) ;
#22203 = CARTESIAN_POINT ( 'NONE',  ( 0.5922249234364754811, -1.371803823430798541, -0.6250000000000000000 ) ) ;
#22204 = CARTESIAN_POINT ( 'NONE',  ( -0.02000000000000000042, -1.845925619402022155, -0.3444148183989317880 ) ) ;
#22205 = DIRECTION ( 'NONE',  ( 0.000000000000000000, 0.000000000000000000, -1.000000000000000000 ) ) ;
#22206 = PLANE ( 'NONE',  #16748 ) ;
#22207 = CARTESIAN_POINT ( 'NONE',  ( 0.08668499250304141646, -0.7271995642927178150, 0.06208601679367901915 ) ) ;
#22208 = CARTESIAN_POINT ( 'NONE',  ( 0.4136294883733457883, -1.694877849074676091, 0.4182417262808776903 ) ) ;
#22209 = CARTESIAN_POINT ( 'NONE',  ( 0.07497864282572899719, -1.322056043867073427, 0.4862695133534066794 ) ) ;
#22210 = CARTESIAN_POINT ( 'NONE',  ( 0.2011421443510955920, -1.242285083301493120, 0.5974872228881977776 ) ) ;
#22211 = CARTESIAN_POINT ( 'NONE',  ( 0.07619306301934503090, -1.974142829211253503, -0.6628502878266334664 ) ) ;
#22212 = CARTESIAN_POINT ( 'NONE',  ( 0.3397077535880359545, -1.654685348432989089, -0.3858274525146626055 ) ) ;
#22213 = DATE_TIME_ROLE ( 'creation_date' ) ;
#22214 = CARTESIAN_POINT ( 'NONE',  ( 0.2370370725713593918, -0.9423068241879761775, 0.4501375130042485906 ) ) ;
#22215 = CARTESIAN_POINT ( 'NONE',  ( 0.3392508469782434810, -1.160100971070933795, 0.4507252195672304951 ) ) ;
#22216 = LINE ( 'NONE', #12945, #13295 ) ;
#22217 = CARTESIAN_POINT ( 'NONE',  ( 0.2615233978049238406, -1.678084768816710648, 0.5373352594323992371 ) ) ;
#22218 = CARTESIAN_POINT ( 'NONE',  ( -0.001215370517532385992, -0.9049306443239834019, 0.2850616817831099770 ) ) ;
#22219 = CARTESIAN_POINT ( 'NONE',  ( -0.0003249894700343514218, -0.9114069365513199905, 0.03530629958352291681 ) ) ;
#22220 = CARTESIAN_POINT ( 'NONE',  ( 0.1986084012382124953, -2.036380768698693444, -0.7103514068621292754 ) ) ;
#22221 = CARTESIAN_POINT ( 'NONE',  ( 0.3434800707737146741, -1.169184835483404905, 0.4282596159937968605 ) ) ;
#22222 = EDGE_CURVE ( 'NONE', #15271, #22420, #31593, .T. ) ;
#22223 = AXIS2_PLACEMENT_3D ( 'NONE', #20396, #28274, #25198 ) ;
#22224 = ORIENTED_EDGE ( 'NONE', *, *, #36841, .F. ) ;
#22225 = ORIENTED_EDGE ( 'NONE', *, *, #30335, .T. ) ;
#22226 = DIRECTION ( 'NONE',  ( 5.551115123125400598E-17, 3.263080277421932464E-16, -1.000000000000000000 ) ) ;
#22227 = ORIENTED_EDGE ( 'NONE', *, *, #21311, .F. ) ;
#22228 = CARTESIAN_POINT ( 'NONE',  ( -0.03158843595483520200, 0.05459869295506113857, 0.4890616322892843981 ) ) ;
#22229 = CARTESIAN_POINT ( 'NONE',  ( -0.04293317454820639451, -0.4876093284570337527, -0.08292018301452905304 ) ) ;
#22230 = EDGE_CURVE ( 'NONE', #19587, #27977, #21533, .T. ) ;
#22231 = CARTESIAN_POINT ( 'NONE',  ( 0.5621458515759424346, -1.398487943849158199, 0.7472131749405318546 ) ) ;
#22233 = ORIENTED_EDGE ( 'NONE', *, *, #24326, .F. ) ;
#22232 = DIRECTION ( 'NONE',  ( 7.000205099780314469E-17, 1.000000000000000000, -6.590151126658399604E-16 ) ) ;
#22234 = B_SPLINE_CURVE_WITH_KNOTS ( 'NONE', 3,
 ( #39994, #2171, #12029, #37318, #33616, #12425, #2567, #2768, #17991, #9127, #18197, #37508, #24376, #5643 ),
 .UNSPECIFIED., .F., .F.,
 ( 4, 2, 2, 2, 2, 2, 4 ),
 ( -6.000000003697073285E-08, 0.004089234075588695644, 0.008178528151177427361, 0.01226782222676616081, 0.01329014574566334157, 0.01431246926456052233, 0.01635711630235487865 ),
 .UNSPECIFIED. ) ;
#22235 = ADVANCED_FACE ( 'NONE', ( #10382 ), #18495, .F. ) ;
#22236 = ORIENTED_EDGE ( 'NONE', *, *, #20600, .F. ) ;
#22237 = CARTESIAN_POINT ( 'NONE',  ( 0.1499999999999993561, 5.828670879282072084E-17, 0.1749999999999999889 ) ) ;
#22238 = ORIENTED_EDGE ( 'NONE', *, *, #5674, .T. ) ;
#22239 = CARTESIAN_POINT ( 'NONE',  ( 0.05196760682231239825, -0.7635565754909066083, 0.6226813947830622809 ) ) ;
#22241 = CARTESIAN_POINT ( 'NONE',  ( 0.2397435495978002262, -1.344164646061327462, 0.4182417262808770797 ) ) ;
#22240 = CARTESIAN_POINT ( 'NONE',  ( 0.4104656799765715736, -1.198377304174871316, 0.6811348502778500347 ) ) ;
#22242 = CARTESIAN_POINT ( 'NONE',  ( -0.2789010053595600835, 0.4834754829570387935, 0.3599999999999999867 ) ) ;
#22243 = CARTESIAN_POINT ( 'NONE',  ( 0.1864213255783573886, -0.8266995537623093027, -0.03797464539687132185 ) ) ;
#22244 = CARTESIAN_POINT ( 'NONE',  ( 0.4136294883733860894, -1.694877849074643228, 0.4182417262808776903 ) ) ;
#22246 = VERTEX_POINT ( 'NONE', #6667 ) ;
#22245 = ORIENTED_EDGE ( 'NONE', *, *, #35019, .T. ) ;
#22247 = CARTESIAN_POINT ( 'NONE',  ( 0.4667607702232405842, -1.076905671295661948, -0.4183295294279661403 ) ) ;
#22248 = CARTESIAN_POINT ( 'NONE',  ( 0.1886409489414842822, -0.8408369741812754539, 0.2375134434870870004 ) ) ;
#22249 = CARTESIAN_POINT ( 'NONE',  ( -0.03301200226531703086, -0.4610556019031558095, 0.2426442821263273819 ) ) ;
#22250 = CARTESIAN_POINT ( 'NONE',  ( 0.5780881571870869484, -1.425136765289637841, 0.7439213802220401295 ) ) ;
#22251 =( BOUNDED_SURFACE ( )  B_SPLINE_SURFACE ( 3, 2, ( 
 ( #15506, #15692, #28242 ),
 ( #31734, #34415, #529 ),
 ( #18373, #9109, #2744 ),
 ( #37296, #30921, #40388 ),
 ( #37916, #34623, #12603 ),
 ( #15293, #18581, #2955 ),
 ( #21675, #40584, #28444 ),
 ( #9726, #37702, #317 ),
 ( #6015, #9525, #31139 ),
 ( #22102, #28060, #12406 ),
 ( #24958, #6424, #31524 ),
 ( #3339, #12822, #22295 ),
 ( #34810, #6615, #16122 ),
 ( #7224, #19411, #1116 ),
 ( #32741, #35840, #26188 ),
 ( #3765, #16318, #13215 ),
 ( #7652, #13623, #4151 ),
 ( #16920, #10350, #38712 ),
 ( #32142, #20216, #38912 ),
 ( #714, #7435, #25996 ),
 ( #16509, #22492, #26385 ),
 ( #35017, #10742, #4548 ),
 ( #10533, #20010, #35239 ),
 ( #14021, #23316, #38518 ) ),
 .UNSPECIFIED., .F., .F., .F. ) 
 B_SPLINE_SURFACE_WITH_KNOTS ( ( 4, 2, 2, 2, 2, 2, 2, 2, 2, 2, 2, 4 ),
 ( 3, 3 ),
 ( 0.008433819124337599629, 0.009129665800632340289, 0.009477589138779709751, 0.009825512476927079214, 0.01052135915322181987, 0.01086928249136918934, 0.01121720582951656053, 0.01191305250581130119, 0.01260889918210604185, 0.01295682252025341305, 0.01330474585840078251, 0.01400059253469552317 ),
 ( 0.000000000000000000, 1.000000000000000000 ),
 .UNSPECIFIED. ) 
 GEOMETRIC_REPRESENTATION_ITEM ( )  RATIONAL_B_SPLINE_SURFACE ( (
 ( 1.000000000000000000, 0.6948880044713926507, 1.000000000000000000),
 ( 1.000000000000000000, 0.6960840624298344492, 1.000000000000000000),
 ( 1.000000000000000000, 0.6983799194115379860, 1.000000000000000000),
 ( 1.000000000000000000, 0.7023957980309022409, 1.000000000000000000),
 ( 1.000000000000000000, 0.7038384642190140816, 1.000000000000000000),
 ( 1.000000000000000000, 0.7066519844213186019, 1.000000000000000000),
 ( 1.000000000000000000, 0.7080301531803978587, 1.000000000000000000),
 ( 1.000000000000000000, 0.7118414011448579437, 1.000000000000000000),
 ( 1.000000000000000000, 0.7139388523227178096, 1.000000000000000000),
 ( 1.000000000000000000, 0.7156078395921124935, 1.000000000000000000),
 ( 1.000000000000000000, 0.7159334618363153435, 1.000000000000000000),
 ( 1.000000000000000000, 0.7160867862248367910, 1.000000000000000000),
 ( 1.000000000000000000, 0.7159093286432843817, 1.000000000000000000),
 ( 1.000000000000000000, 0.7146582677834552033, 1.000000000000000000),
 ( 1.000000000000000000, 0.7128727118445921107, 1.000000000000000000),
 ( 1.000000000000000000, 0.7079968471081192760, 1.000000000000000000),
 ( 1.000000000000000000, 0.7050215538929806014, 1.000000000000000000),
 ( 1.000000000000000000, 0.7005626529068207375, 1.000000000000000000),
 ( 1.000000000000000000, 0.6990679116423534900, 1.000000000000000000),
 ( 1.000000000000000000, 0.6963021034989965719, 1.000000000000000000),
 ( 1.000000000000000000, 0.6950231705106640900, 1.000000000000000000),
 ( 1.000000000000000000, 0.6916869647287414713, 1.000000000000000000),
 ( 1.000000000000000000, 0.6899239366554796860, 1.000000000000000000),
 ( 1.000000000000000000, 0.6900227658400107655, 1.000000000000000000) ) ) 
 REPRESENTATION_ITEM ( '' )  SURFACE ( )  );
#22252 = EDGE_CURVE ( 'NONE', #13794, #18202, #18877, .T. ) ;
#22253 = CARTESIAN_POINT ( 'NONE',  ( 0.3364639209793421348, -1.089988309885336681, 0.7406982884823408719 ) ) ;
#22254 = CARTESIAN_POINT ( 'NONE',  ( 0.1859432605888821921, -0.7573098151843028480, 0.1022962920937455361 ) ) ;
#22255 = APPROVAL ( #36661, 'UNSPECIFIED' ) ;
#22256 = CARTESIAN_POINT ( 'NONE',  ( 0.2959710460089218231, -1.597927643852713464, 0.9577133037227931744 ) ) ;
#22257 = CIRCLE ( 'NONE', #30742, 0.5302738246768088359 ) ;
#22258 = DIRECTION ( 'NONE',  ( 1.000000000000000000, 0.000000000000000000, 0.000000000000000000 ) ) ;
#22259 = DIRECTION ( 'NONE',  ( 0.000000000000000000, 0.3090169943749439541, -0.9510565162951547524 ) ) ;
#22260 = CARTESIAN_POINT ( 'NONE',  ( 0.05999999999999990757, 0.1428018198284763673, -0.2638325989215043466 ) ) ;
#22261 = DIRECTION ( 'NONE',  ( 1.000000000000000000, 6.779273404243070203E-32, 4.314083075427408311E-32 ) ) ;
#22262 = DIRECTION ( 'NONE',  ( -1.000000000000000000, -0.000000000000000000, -0.000000000000000000 ) ) ;
#22263 = CARTESIAN_POINT ( 'NONE',  ( 0.002083146443013521830, -0.4777046557262296100, 0.1638349238242636507 ) ) ;
#22264 = CARTESIAN_POINT ( 'NONE',  ( 0.1169578367557221887, -1.398407385406643222, 0.6329296710379738178 ) ) ;
#22265 = DATE_AND_TIME ( #28211, #35216 ) ;
#22266 = CARTESIAN_POINT ( 'NONE',  ( -0.05078310099561082064, 0.4632425114130818700, 0.09919524461159424933 ) ) ;
#22267 = CARTESIAN_POINT ( 'NONE',  ( 0.2090306192065299884, -1.362070338884064258, -0.3027639479267801859 ) ) ;
#22268 = EDGE_CURVE ( 'NONE', #34829, #13520, #40133, .T. ) ;
#22269 = EDGE_LOOP ( 'NONE', ( #8426, #39264, #9669, #36856 ) ) ;
#22270 = CARTESIAN_POINT ( 'NONE',  ( 0.4831567767736278385, -1.121977757481035010, 0.5105939270972588151 ) ) ;
#22271 = ORIENTED_EDGE ( 'NONE', *, *, #36823, .T. ) ;
#22272 = CARTESIAN_POINT ( 'NONE',  ( 0.4527603377605404766, -1.144379813877050012, -0.3965114147629228980 ) ) ;
#22273 = CARTESIAN_POINT ( 'NONE',  ( 0.2439840020134950993, -1.523895357778563664, 0.8969720475523240699 ) ) ;
#22274 = EDGE_CURVE ( 'NONE', #11170, #19917, #3633, .T. ) ;
#22275 = CARTESIAN_POINT ( 'NONE',  ( 0.5954621451176055347, -1.487120967891011114, 0.5849300529686594086 ) ) ;
#22276 = EDGE_CURVE ( 'NONE', #17780, #34098, #11008, .T. ) ;
#22278 = VERTEX_POINT ( 'NONE', #29920 ) ;
#22277 = CARTESIAN_POINT ( 'NONE',  ( 0.3511079287476752686, -1.164805985122749687, 0.4335040596137051394 ) ) ;
#22279 = EDGE_CURVE ( 'NONE', #30753, #24795, #34204, .T. ) ;
#22281 = ORIENTED_EDGE ( 'NONE', *, *, #23378, .T. ) ;
#22280 = ORIENTED_EDGE ( 'NONE', *, *, #35305, .F. ) ;
#22282 = CARTESIAN_POINT ( 'NONE',  ( 0.5299567605269758230, -1.673323247217261223, -0.5639626154930592605 ) ) ;
#22283 = VERTEX_POINT ( 'NONE', #14675 ) ;
#22284 = CYLINDRICAL_SURFACE ( 'NONE', #2928, 0.06000000000000038636 ) ;
#22285 = ITEM_DEFINED_TRANSFORMATION ( 'NONE', 'NONE', #13420,  #27819 ) ;
#22286 = LINE ( 'NONE', #12594, #34285 ) ;
#22287 = ORIENTED_EDGE ( 'NONE', *, *, #22762, .F. ) ;
#22288 = CARTESIAN_POINT ( 'NONE',  ( 0.1029610634938303709, -0.7684373263134592902, 0.3557047774870934487 ) ) ;
#22289 = CARTESIAN_POINT ( 'NONE',  ( 0.1409906984825553267, -1.239706420848685875, -0.5155029497116575543 ) ) ;
#22290 = CARTESIAN_POINT ( 'NONE',  ( 0.5266619910787769809, -1.525087864311528429, 0.6234923701237724547 ) ) ;
#22291 = CARTESIAN_POINT ( 'NONE',  ( 0.6404767502594985729, -1.465846671489676067, -0.6342850214802828734 ) ) ;
#22292 = ADVANCED_FACE ( 'NONE', ( #40383 ), #5203, .F. ) ;
#22293 = CARTESIAN_POINT ( 'NONE',  ( -0.1699617389507599718, 0.4951775333576751148, 0.1374137075621940374 ) ) ;
#22294 = ORIENTED_EDGE ( 'NONE', *, *, #17180, .T. ) ;
#22295 = CARTESIAN_POINT ( 'NONE',  ( 0.4074647527740007380, -1.709076545307301798, 0.6202421242740956409 ) ) ;
#22296 = CARTESIAN_POINT ( 'NONE',  ( 0.7005072418814222157, -1.435918383503960394, 0.7932214653155064132 ) ) ;
#22297 = ORIENTED_EDGE ( 'NONE', *, *, #24100, .F. ) ;
#22298 = FACE_OUTER_BOUND ( 'NONE', #37249, .T. ) ;
#22299 = CARTESIAN_POINT ( 'NONE',  ( 0.5900193846650280127, -1.451085630206152999, 0.7130590060845574119 ) ) ;
#22300 = DIRECTION ( 'NONE',  ( 0.000000000000000000, 3.330669073875470114E-16, 1.000000000000000000 ) ) ;
#22301 = LENGTH_MEASURE_WITH_UNIT ( LENGTH_MEASURE( 0.02539999999999999897 ), #9732 );
#22302 = CARTESIAN_POINT ( 'NONE',  ( 0.4952488905928916774, -1.196841907270136840, 0.4182417262808778013 ) ) ;
#22303 = CARTESIAN_POINT ( 'NONE',  ( -0.01548846960721252282, -0.4730347584884301293, 0.2341461249027971259 ) ) ;
#22304 = CARTESIAN_POINT ( 'NONE',  ( 0.02115399423329476433, -1.083931147575175613, 0.6303919839426973537 ) ) ;
#22305 = CARTESIAN_POINT ( 'NONE',  ( 0.5043207191046787941, -1.105492587439252494, 0.6133613128836958861 ) ) ;
#22306 = PERSON_AND_ORGANIZATION_ROLE ( 'design_owner' ) ;
#22307 = FACE_OUTER_BOUND ( 'NONE', #20079, .T. ) ;
#22308 = CARTESIAN_POINT ( 'NONE',  ( 0.05999999999999990757, 0.1369749717427355129, -0.1457321416712075435 ) ) ;
#22309 = CARTESIAN_POINT ( 'NONE',  ( -0.03874953289575296805, -0.03331175461110518626, 0.4752512399555741673 ) ) ;
#22310 = ADVANCED_FACE ( 'NONE', ( #8908 ), #5613, .T. ) ;
#22311 = VERTEX_POINT ( 'NONE', #15501 ) ;
#22312 = CARTESIAN_POINT ( 'NONE',  ( 0.2059273467974225835, -1.283046334493782359, -0.3904158619672754016 ) ) ;
#22313 = CARTESIAN_POINT ( 'NONE',  ( 0.05999999999999990757, 0.7171888913565960255, -0.2950238883388468514 ) ) ;
#22314 = B_SPLINE_CURVE_WITH_KNOTS ( 'NONE', 3,
 ( #9995, #178, #19661, #16575, #32197, #9594, #28517, #6490 ),
 .UNSPECIFIED., .F., .F.,
 ( 4, 2, 2, 4 ),
 ( 0.000000000000000000, 0.0002979882110954374698, 0.0005959764221908749396, 0.001191952844381744675 ),
 .UNSPECIFIED. ) ;
#22315 = EDGE_CURVE ( 'NONE', #39656, #4670, #27245, .T. ) ;
#22316 = CARTESIAN_POINT ( 'NONE',  ( 0.08955701898351196844, -0.5706670494699135343, 0.1066062274051425146 ) ) ;
#22317 = ORIENTED_EDGE ( 'NONE', *, *, #31770, .T. ) ;
#22318 = CARTESIAN_POINT ( 'NONE',  ( 0.05999999999999990757, 0.7171888913565960255, -0.2950238883388468514 ) ) ;
#22319 = EDGE_CURVE ( 'NONE', #4341, #25189, #21735, .T. ) ;
#22320 = CARTESIAN_POINT ( 'NONE',  ( 0.005103737174765597510, -0.9529501791669972022, 0.6308053658798797869 ) ) ;
#22322 = VERTEX_POINT ( 'NONE', #12401 ) ;
#22321 = ORIENTED_EDGE ( 'NONE', *, *, #38776, .F. ) ;
#22323 = CARTESIAN_POINT ( 'NONE',  ( -0.05464101615137762630, -2.023118915020511999, -0.4686803309516410221 ) ) ;
#22324 = EDGE_LOOP ( 'NONE', ( #39395, #10502 ) ) ;
#22325 = CARTESIAN_POINT ( 'NONE',  ( -0.1743922129835736579, -0.5166151207188712791, 0.3599999999999997091 ) ) ;
#22326 = CYLINDRICAL_SURFACE ( 'NONE', #35752, 0.03749999999977551152 ) ;
#22328 = DIRECTION ( 'NONE',  ( -1.000000000000000000, 0.000000000000000000, -5.691349986800505477E-16 ) ) ;
#22327 = DIRECTION ( 'NONE',  ( -1.000000000000000000, -6.779273404243070203E-32, -4.314083075427408311E-32 ) ) ;
#22329 = CARTESIAN_POINT ( 'NONE',  ( 0.01896931156527473933, -0.2428675472501181931, -0.4598342473848889278 ) ) ;
#22330 = EDGE_LOOP ( 'NONE', ( #24244, #18889, #28528, #39998, #10767, #27874, #2126, #16798, #1474 ) ) ;
#22331 = CARTESIAN_POINT ( 'NONE',  ( 0.3371096829608895007, -1.701240623061720969, -0.6069842154957213465 ) ) ;
#22332 = ORIENTED_EDGE ( 'NONE', *, *, #39615, .T. ) ;
#22333 = CARTESIAN_POINT ( 'NONE',  ( 0.08992510688325772161, -0.6057077997829167781, 0.1553500322290060354 ) ) ;
#22334 = VERTEX_POINT ( 'NONE', #37093 ) ;
#22335 = CARTESIAN_POINT ( 'NONE',  ( 0.004323292021450524797, -0.5016872349303481693, 0.3729438605722754096 ) ) ;
#22336 = CARTESIAN_POINT ( 'NONE',  ( 0.4314429043751959458, -1.476193151465878595, 0.8070760231935298901 ) ) ;
#22337 = ADVANCED_FACE ( 'NONE', ( #12208 ), #9236, .T. ) ;
#22339 = CARTESIAN_POINT ( 'NONE',  ( -0.1304423469995341367, -0.5262799683630398073, 0.3599999999999994316 ) ) ;
#22338 = CARTESIAN_POINT ( 'NONE',  ( 0.004308327751199931069, -0.5715689420563186962, 0.3310798223114407302 ) ) ;
#22340 = CARTESIAN_POINT ( 'NONE',  ( 0.3302290664199810100, -1.638364056477709996, -0.3722368618827794906 ) ) ;
#22341 = CARTESIAN_POINT ( 'NONE',  ( 0.2561730234726187216, -0.9528060625594280131, 0.4936757400543403396 ) ) ;
#22342 = ADVANCED_FACE ( 'NONE', ( #21061 ), #15623, .F. ) ;
#22343 = UNCERTAINTY_MEASURE_WITH_UNIT (LENGTH_MEASURE( 1.000000000000000082E-05 ), #16516, 'distance_accuracy_value', 'NONE');
#22344 = LINE ( 'NONE', #9155, #17993 ) ;
#22345 = ADVANCED_FACE ( 'NONE', ( #2950 ), #22424, .T. ) ;
#22346 = CARTESIAN_POINT ( 'NONE',  ( 0.2597702376225676235, -1.565296447219295173, -0.3170323014659355287 ) ) ;
#22347 = CARTESIAN_POINT ( 'NONE',  ( 0.5809782845877130564, -1.495266891998359382, 0.5744612900028297497 ) ) ;
#22348 = CARTESIAN_POINT ( 'NONE',  ( -0.05187277790672548822, 0.2620383623028448850, -0.3911539469301719696 ) ) ;
#22349 = CARTESIAN_POINT ( 'NONE',  ( -0.03170752374382804911, -0.4481131438208651452, -0.2027288335082092219 ) ) ;
#22350 = CARTESIAN_POINT ( 'NONE',  ( 0.1204904522838102926, -0.7160080108176953839, 0.5344870570319224523 ) ) ;
#22351 = CARTESIAN_POINT ( 'NONE',  ( 0.5255575159092462645, -1.179369731138129040, 0.4666486945702073563 ) ) ;
#22352 = CARTESIAN_POINT ( 'NONE',  ( 0.6778058174389349766, -1.398346805643282620, 0.6444391890521875554 ) ) ;
#22353 = CARTESIAN_POINT ( 'NONE',  ( 0.4209353462971754944, -1.136818033495635261, 0.4445034551534702283 ) ) ;
#22354 = CARTESIAN_POINT ( 'NONE',  ( 0.06015859323110296641, -1.307383187822563020, 0.6320855273814715014 ) ) ;
#22355 = VECTOR ( 'NONE', #22603, 39.37007874015748143 ) ;
#22356 = CARTESIAN_POINT ( 'NONE',  ( 0.04230170315644477680, 0.4483301424763361243, -0.1366247710447582586 ) ) ;
#22357 = DIRECTION ( 'NONE',  ( -1.000000000000000000, -0.000000000000000000, -0.000000000000000000 ) ) ;
#22358 = CARTESIAN_POINT ( 'NONE',  ( 0.09719910960680759604, -0.8177032743061471987, 0.3260758418614409515 ) ) ;
#22359 = CARTESIAN_POINT ( 'NONE',  ( 0.03868264068766665009, 0.2522289290439784226, -0.4043438810462526845 ) ) ;
#22360 = CARTESIAN_POINT ( 'NONE',  ( -0.2746410161513779258, -2.423474325126674156, -0.5576739111151496342 ) ) ;
#22361 = AXIS2_PLACEMENT_3D ( 'NONE', #30048, #23674, #1873 ) ;
#22362 = ORIENTED_EDGE ( 'NONE', *, *, #22787, .F. ) ;
#22363 = CARTESIAN_POINT ( 'NONE',  ( -0.02953079040095700838, 0.000000000000000000, 0.000000000000000000 ) ) ;
#22364 = CARTESIAN_POINT ( 'NONE',  ( 0.1746104702851725143, -0.8080234154602033980, 0.5960121186932698656 ) ) ;
#22365 = EDGE_CURVE ( 'NONE', #26020, #16545, #35521, .T. ) ;
#22366 = CARTESIAN_POINT ( 'NONE',  ( -0.08000000000000000167, -1.622350287959229087, -0.08960079202753243321 ) ) ;
#22367 = CARTESIAN_POINT ( 'NONE',  ( 0.3332916228607076259, -1.159868621030426983, 0.5808959208038069200 ) ) ;
#22368 = EDGE_CURVE ( 'NONE', #14209, #10794, #36846, .T. ) ;
#22369 = ORIENTED_EDGE ( 'NONE', *, *, #16291, .F. ) ;
#22370 = CARTESIAN_POINT ( 'NONE',  ( 0.7059656540691128246, -1.571716619208481935, -0.5155029497116575543 ) ) ;
#22371 = DIRECTION ( 'NONE',  ( -0.4999999999999952816, 0.7066258520834667323, 0.5006794435238172136 ) ) ;
#22372 = LINE ( 'NONE', #35493, #12561 ) ;
#22373 = DIRECTION ( 'NONE',  ( 0.000000000000000000, -0.9510565162951545304, -0.3090169943749445092 ) ) ;
#22374 = CARTESIAN_POINT ( 'NONE',  ( 0.4828762206425698533, -1.264095418145567251, 0.6661113250919497020 ) ) ;
#22376 = CARTESIAN_POINT ( 'NONE',  ( 0.5744493500335104974, -1.624687623158924232, 0.5560814181295907765 ) ) ;
#22375 = FACE_OUTER_BOUND ( 'NONE', #10477, .T. ) ;
#22377 = CARTESIAN_POINT ( 'NONE',  ( 0.4835150722484384267, -1.077540828773440484, 0.6059843185820091849 ) ) ;
#22378 = VERTEX_POINT ( 'NONE', #526 ) ;
#22379 = DATE_TIME_ROLE ( 'classification_date' ) ;
#22380 = DIRECTION ( 'NONE',  ( -0.8660512985181423318, -0.4999551463231871051, 0.000000000000000000 ) ) ;
#22381 = ORIENTED_EDGE ( 'NONE', *, *, #33623, .F. ) ;
#22382 = CARTESIAN_POINT ( 'NONE',  ( 0.08947281526746891922, -0.7905738690218343523, 0.6404966654700502415 ) ) ;
#22384 = CARTESIAN_POINT ( 'NONE',  ( 0.1109460505795314550, -0.9288804736197510126, 0.1344306538234449899 ) ) ;
#22383 = DIRECTION ( 'NONE',  ( 1.445848444424219201E-15, -1.000000000000000000, -2.361472542561095431E-16 ) ) ;
#22385 = CARTESIAN_POINT ( 'NONE',  ( -0.6247879186461524625, 0.2375666616292461675, 0.3749999999999991673 ) ) ;
#22386 = ORIENTED_EDGE ( 'NONE', *, *, #29537, .F. ) ;
#22387 = CONICAL_SURFACE ( 'NONE', #4597, 0.1620173459747806799, 1.047197551196601184 ) ;
#22388 = EDGE_LOOP ( 'NONE', ( #27483, #36477, #40274, #39884 ) ) ;
#22389 = VERTEX_POINT ( 'NONE', #25570 ) ;
#22390 = CARTESIAN_POINT ( 'NONE',  ( 0.4930915531067465718, -1.082784575164420726, 0.5786337965014383133 ) ) ;
#22391 = CARTESIAN_POINT ( 'NONE',  ( 0.1440976411593163087, -0.6767727035454040863, 0.4660634794818891424 ) ) ;
#22392 = ORIENTED_EDGE ( 'NONE', *, *, #11709, .T. ) ;
#22393 = FACE_OUTER_BOUND ( 'NONE', #23935, .T. ) ;
#22394 = CARTESIAN_POINT ( 'NONE',  ( 0.06540210900078118061, -2.045735273566230639, -0.3096830216599801844 ) ) ;
#22395 = FACE_OUTER_BOUND ( 'NONE', #34105, .T. ) ;
#22396 = AXIS2_PLACEMENT_3D ( 'NONE', #23890, #32914, #30453 ) ;
#22397 = CARTESIAN_POINT ( 'NONE',  ( 0.1855153659605877081, -0.8219892960459125320, 0.1767872597970533977 ) ) ;
#22398 = FACE_OUTER_BOUND ( 'NONE', #38704, .T. ) ;
#22399 = CARTESIAN_POINT ( 'NONE',  ( 0.3922565764085018114, -1.717990344284888060, 0.6205140842479107688 ) ) ;
#22400 = CARTESIAN_POINT ( 'NONE',  ( 0.08833238169483845215, -0.6441912979656407856, 0.06334869283158285624 ) ) ;
#22401 = CARTESIAN_POINT ( 'NONE',  ( 0.7394099696849650849, -1.503374687208528737, 0.6698237402283935271 ) ) ;
#22402 = DIRECTION ( 'NONE',  ( -1.000000000000000000, -0.000000000000000000, -0.000000000000000000 ) ) ;
#22403 = CARTESIAN_POINT ( 'NONE',  ( 0.1099113005465149340, -1.419268643255550355, 0.5685633924154458452 ) ) ;
#22404 = DIRECTION ( 'NONE',  ( 1.188678714063518227E-15, -1.000000000000000000, -3.263080277421930985E-16 ) ) ;
#22405 = CARTESIAN_POINT ( 'NONE',  ( 0.1003432527060652141, -1.374243440585479981, 0.6783211582849573151 ) ) ;
#22406 = PERSON_AND_ORGANIZATION_ROLE ( 'creator' ) ;
#22407 = CARTESIAN_POINT ( 'NONE',  ( 0.6349199332347138514, -1.492121435015029585, -0.6355974108494197861 ) ) ;
#22408 = DIRECTION ( 'NONE',  ( -0.9378410757839557021, -0.1072489841977669889, -0.3300784330442382286 ) ) ;
#22409 = FACE_OUTER_BOUND ( 'NONE', #18738, .T. ) ;
#22410 = PLANE ( 'NONE',  #10711 ) ;
#22411 = CARTESIAN_POINT ( 'NONE',  ( -8.537024980200822558E-17, -0.6872203660140397963, 0.1457185332388691301 ) ) ;
#22412 = CARTESIAN_POINT ( 'NONE',  ( 0.5826009915492634805, -1.549810527521380932, -0.4246621135213465847 ) ) ;
#22413 = CARTESIAN_POINT ( 'NONE',  ( 0.1807987625579654534, -1.701547269739460022, -0.6830814722341453926 ) ) ;
#22414 = AXIS2_PLACEMENT_3D ( 'NONE', #15536, #34651, #13052 ) ;
#22415 = DIRECTION ( 'NONE',  ( -1.000000000000000000, -0.000000000000000000, -0.000000000000000000 ) ) ;
#22416 = VERTEX_POINT ( 'NONE', #12600 ) ;
#22417 = ORIENTED_EDGE ( 'NONE', *, *, #37555, .F. ) ;
#22418 = AXIS2_PLACEMENT_3D ( 'NONE', #6968, #19541, #32072 ) ;
#22419 = CARTESIAN_POINT ( 'NONE',  ( 0.000000000000000000, -0.05999999999999990757, 0.000000000000000000 ) ) ;
#22420 = VERTEX_POINT ( 'NONE', #19408 ) ;
#22421 = AXIS2_PLACEMENT_3D ( 'NONE', #11270, #1834, #27116 ) ;
#22422 = FACE_OUTER_BOUND ( 'NONE', #37429, .T. ) ;
#22423 = CARTESIAN_POINT ( 'NONE',  ( 0.4559719632891929830, -1.698713290701216350, -0.5155029497116575543 ) ) ;
#22424 = TOROIDAL_SURFACE ( 'NONE', #32229, 1.971674066779348866, 0.02999999999999999889 ) ;
#22425 = CARTESIAN_POINT ( 'NONE',  ( 0.5935870542470136346, -1.451877841075679632, 0.6599787284733793502 ) ) ;
#22426 = B_SPLINE_CURVE_WITH_KNOTS ( 'NONE', 3,
 ( #25494, #12523, #18704, #12726 ),
 .UNSPECIFIED., .F., .F.,
 ( 4, 4 ),
 ( 0.000000000000000000, 0.0005928691263773363217 ),
 .UNSPECIFIED. ) ;
#22428 = ORIENTED_EDGE ( 'NONE', *, *, #14401, .T. ) ;
#22427 = DIRECTION ( 'NONE',  ( 1.000000000000000000, 0.000000000000000000, 7.906745362128971688E-16 ) ) ;
#22429 = ORIENTED_EDGE ( 'NONE', *, *, #18790, .F. ) ;
#22430 = CARTESIAN_POINT ( 'NONE',  ( 0.5546634778460078907, -1.622195262996998233, 0.4988266963081158800 ) ) ;
#22431 = VERTEX_POINT ( 'NONE', #28851 ) ;
#22432 = CARTESIAN_POINT ( 'NONE',  ( 0.01967356235354560112, -0.6161222107093594635, 0.4019596896130384622 ) ) ;
#22434 = CARTESIAN_POINT ( 'NONE',  ( 0.1123349855930559915, -0.8080303305208232922, -0.06315017404710350502 ) ) ;
#22433 = CARTESIAN_POINT ( 'NONE',  ( 0.5473076987003111515, -1.651760216406904513, -0.4929644493450987541 ) ) ;
#22435 = DIRECTION ( 'NONE',  ( -0.8660254037844400399, -0.3758398823372107178, 0.3297641321380319068 ) ) ;
#22436 = LINE ( 'NONE', #25519, #39078 ) ;
#22437 = APPROVAL_ROLE ( '' ) ;
#22438 = CARTESIAN_POINT ( 'NONE',  ( 0.4047092701292824279, -1.701611041320455708, 0.4182417262808776903 ) ) ;
#22440 = ORIENTED_EDGE ( 'NONE', *, *, #17430, .F. ) ;
#22439 = EDGE_LOOP ( 'NONE', ( #24485, #18623, #38330, #5229 ) ) ;
#22441 = CARTESIAN_POINT ( 'NONE',  ( 0.4602558791604159927, -1.075954481373732508, -0.4172575352404306881 ) ) ;
#22442 = CARTESIAN_POINT ( 'NONE',  ( 0.1109778970610976606, -0.9286704811356188971, 0.1599727523405532759 ) ) ;
#22443 = CARTESIAN_POINT ( 'NONE',  ( -0.01895884884825295436, 0.07380796352548431305, -0.5147901372834192690 ) ) ;
#22444 = CARTESIAN_POINT ( 'NONE',  ( 0.5633198742680586291, -1.401022841391578400, 0.7649915433844801660 ) ) ;
#22445 = CARTESIAN_POINT ( 'NONE',  ( 0.3523921359471319237, -1.112685253907127247, 0.7380400840877293644 ) ) ;
#22446 = CARTESIAN_POINT ( 'NONE',  ( -0.05464101615137770263, -2.320036485105098301, -0.2941690811493925528 ) ) ;
#22447 = VECTOR ( 'NONE', #35717, 39.37007874015748854 ) ;
#22448 = FACE_OUTER_BOUND ( 'NONE', #834, .T. ) ;
#22449 = VECTOR ( 'NONE', #25479, 39.37007874015748143 ) ;
#22450 = CARTESIAN_POINT ( 'NONE',  ( 0.4342919329069486190, -1.232046631451992225, 0.5547567841613109119 ) ) ;
#22451 = CARTESIAN_POINT ( 'NONE',  ( 0.3254773505639530495, -1.768308184846890452, 0.5269442850043757343 ) ) ;
#22452 = DIRECTION ( 'NONE',  ( -1.000000000000000000, -6.779273404243070203E-32, -4.314083075427408311E-32 ) ) ;
#22453 = DIRECTION ( 'NONE',  ( 0.9378410757839510392, -0.2807814858886686360, -0.2039996905746500333 ) ) ;
#22454 = CARTESIAN_POINT ( 'NONE',  ( 0.001268890223027725143, -0.002211790590265117970, -0.001112171007692230656 ) ) ;
#22455 = CIRCLE ( 'NONE', #25641, 0.1033070866141734129 ) ;
#22456 = VECTOR ( 'NONE', #11055, 39.37007874015748143 ) ;
#22457 = CARTESIAN_POINT ( 'NONE',  ( -0.01736481776669303659, -0.6872203660140440151, 0.1457185332388702681 ) ) ;
#22458 = CARTESIAN_POINT ( 'NONE',  ( -0.02000000000000000042, -1.999693152383498873, -0.3073943322174664261 ) ) ;
#22459 = CARTESIAN_POINT ( 'NONE',  ( 0.1849042594950439655, -1.699762810001741453, -0.6534071581412237428 ) ) ;
#22460 = PERSON_AND_ORGANIZATION ( #28500, #32463 ) ;
#22461 = CARTESIAN_POINT ( 'NONE',  ( 0.3634995547569259688, -1.769442106537615134, -0.6725227346654005789 ) ) ;
#22462 = CARTESIAN_POINT ( 'NONE',  ( 0.3316976289008216061, -1.758220054772660745, 0.5638205628752049892 ) ) ;
#22463 = CARTESIAN_POINT ( 'NONE',  ( 0.6436302007692352722, -1.590381715263790463, -0.5770581850489380216 ) ) ;
#22464 = EDGE_CURVE ( 'NONE', #39409, #14867, #27641, .T. ) ;
#22465 = EDGE_LOOP ( 'NONE', ( #8014, #36980, #16598, #11530, #36126, #36595 ) ) ;
#22466 = CARTESIAN_POINT ( 'NONE',  ( 0.4830778208102094462, -1.123855190747131472, 0.5028193722743440341 ) ) ;
#22467 = ORIENTED_EDGE ( 'NONE', *, *, #15527, .T. ) ;
#22468 = CARTESIAN_POINT ( 'NONE',  ( 0.1056036318510553268, -1.411794347249417880, 0.5652933847224521635 ) ) ;
#22469 = APPLIED_DATE_AND_TIME_ASSIGNMENT ( #29913, #22588, ( #3006 ) ) ;
#22470 = CARTESIAN_POINT ( 'NONE',  ( 0.2709457873140602158, -1.674456041952191887, 0.6046742933308183465 ) ) ;
#22471 = CARTESIAN_POINT ( 'NONE',  ( 0.1358503106379023995, -0.5959801875305653640, 0.3049145827815397669 ) ) ;
#22473 = EDGE_LOOP ( 'NONE', ( #23730, #32181, #31506 ) ) ;
#22472 = CYLINDRICAL_SURFACE ( 'NONE', #8613, 2.001674066779353556 ) ;
#22475 = ORIENTED_EDGE ( 'NONE', *, *, #28545, .F. ) ;
#22474 = VERTEX_POINT ( 'NONE', #34620 ) ;
#22476 = DIRECTION ( 'NONE',  ( -1.000000000000000000, -2.280301054154495132E-31, 1.664003471950577689E-31 ) ) ;
#22477 = VECTOR ( 'NONE', #26179, 39.37007874015748143 ) ;
#22478 =( BOUNDED_SURFACE ( )  B_SPLINE_SURFACE ( 3, 2, ( 
 ( #24368, #8930, #39988 ),
 ( #5419, #2366, #30740 ),
 ( #11412, #36512, #18190 ),
 ( #5824, #27655, #8324 ),
 ( #14905, #40188, #33415 ),
 ( #30332, #36906, #34022 ),
 ( #27266, #36707, #5637 ),
 ( #12023, #33608, #8516 ),
 ( #21081, #24580, #37117 ),
 ( #21507, #6032, #18599 ),
 ( #21687, #3734, #19760 ),
 ( #32297, #19970, #32110 ),
 ( #881, #35595, #1087 ),
 ( #31155, #16681, #4112 ),
 ( #35399, #22461, #15309 ),
 ( #25544, #25964, #22676 ),
 ( #32505, #28826, #38072 ),
 ( #24791, #37311, #7394 ),
 ( #10498, #40403, #12229 ),
 ( #34987, #10320, #3525 ),
 ( #16288, #6797, #9121 ),
 ( #13174, #9889, #38487 ),
 ( #34217, #12997, #31913 ),
 ( #3917, #684, #19379 ),
 ( #16475, #25744, #28628 ),
 ( #38270, #10103, #35208 ) ),
 .UNSPECIFIED., .F., .F., .T. ) 
 B_SPLINE_SURFACE_WITH_KNOTS ( ( 4, 2, 2, 2, 2, 2, 2, 2, 2, 2, 2, 2, 4 ),
 ( 3, 3 ),
 ( 0.03478970966414503263, 0.03529932688707621696, 0.03580894411000740130, 0.03682817855586976996, 0.03886664744759451423, 0.04090511633931925850, 0.04294358523104399583, 0.04498205412276874010, 0.04600128856863111571, 0.04702052301449348437, 0.04803975746035585304, 0.04905899190621822170, 0.05109746079794296597 ),
 ( 0.000000000000000000, 1.000000000000000000 ),
 .UNSPECIFIED. ) 
 GEOMETRIC_REPRESENTATION_ITEM ( )  RATIONAL_B_SPLINE_SURFACE ( (
 ( 1.000000000000000000, 0.7053326528219874270, 1.000000000000000000),
 ( 1.000000000000000000, 0.7069087193608284414, 1.000000000000000000),
 ( 1.000000000000000000, 0.7074454249098806047, 1.000000000000000000),
 ( 1.000000000000000000, 0.7079727039066888716, 1.000000000000000000),
 ( 1.000000000000000000, 0.7079140579849947379, 1.000000000000000000),
 ( 1.000000000000000000, 0.7072990859638439431, 1.000000000000000000),
 ( 1.000000000000000000, 0.7062992663257996462, 1.000000000000000000),
 ( 1.000000000000000000, 0.7026654075174075809, 1.000000000000000000),
 ( 1.000000000000000000, 0.6993568048661583658, 1.000000000000000000),
 ( 1.000000000000000000, 0.6923303540839972348, 1.000000000000000000),
 ( 1.000000000000000000, 0.6885467396574446175, 1.000000000000000000),
 ( 1.000000000000000000, 0.6809569680526225133, 1.000000000000000000),
 ( 1.000000000000000000, 0.6771650901613724960, 1.000000000000000000),
 ( 1.000000000000000000, 0.6704471956693288659, 1.000000000000000000),
 ( 1.000000000000000000, 0.6675067785250807795, 1.000000000000000000),
 ( 1.000000000000000000, 0.6649784099743590859, 1.000000000000000000),
 ( 1.000000000000000000, 0.6644567522668610726, 1.000000000000000000),
 ( 1.000000000000000000, 0.6643594168469727501, 1.000000000000000000),
 ( 1.000000000000000000, 0.6647836916442323441, 1.000000000000000000),
 ( 1.000000000000000000, 0.6667676599421886730, 1.000000000000000000),
 ( 1.000000000000000000, 0.6683270600134922912, 1.000000000000000000),
 ( 1.000000000000000000, 0.6727537477506539965, 1.000000000000000000),
 ( 1.000000000000000000, 0.6756357399901673499, 1.000000000000000000),
 ( 1.000000000000000000, 0.6860398255734453388, 1.000000000000000000),
 ( 1.000000000000000000, 0.6954024235273548182, 1.000000000000000000),
 ( 1.000000000000000000, 0.7067908011272799884, 1.000000000000000000) ) ) 
 REPRESENTATION_ITEM ( '' )  SURFACE ( )  );
#22479 = ORIENTED_EDGE ( 'NONE', *, *, #29933, .F. ) ;
#22480 = VECTOR ( 'NONE', #2857, 39.37007874015748143 ) ;
#22481 = DIRECTION ( 'NONE',  ( 0.000000000000000000, 0.000000000000000000, -1.000000000000000000 ) ) ;
#22482 = CIRCLE ( 'NONE', #2088, 0.1000000000000000194 ) ;
#22483 = CARTESIAN_POINT ( 'NONE',  ( 0.3048157867855714742, -1.756814508404978215, 0.5624209259133406968 ) ) ;
#22484 = ORIENTED_EDGE ( 'NONE', *, *, #24547, .F. ) ;
#22485 = CARTESIAN_POINT ( 'NONE',  ( 0.1593808023014779141, -0.8351711200615056230, 0.5495798524048867151 ) ) ;
#22486 = CARTESIAN_POINT ( 'NONE',  ( 0.08990954768171793843, -0.5436503405977816117, 0.1466997848779070523 ) ) ;
#22487 = CARTESIAN_POINT ( 'NONE',  ( 0.4534567705953844730, -1.373683393137863584, 0.8250533907914637810 ) ) ;
#22488 = CARTESIAN_POINT ( 'NONE',  ( 0.5835086506366403691, -1.603182442426240417, -0.5754264449309163254 ) ) ;
#22489 = CARTESIAN_POINT ( 'NONE',  ( -0.1623906354757116699, 0.5045448597005526281, 0.1308137833173692033 ) ) ;
#22490 = CARTESIAN_POINT ( 'NONE',  ( 0.6947424619376043609, -1.490652314882815688, 0.4500177634849870101 ) ) ;
#22491 = VERTEX_POINT ( 'NONE', #25159 ) ;
#22492 = CARTESIAN_POINT ( 'NONE',  ( 0.3447343635093774172, -1.745799762367185926, 0.5848968271157334309 ) ) ;
#22493 = CARTESIAN_POINT ( 'NONE',  ( 0.6290611267951696783, -1.457193995254231433, 0.8259264861884191289 ) ) ;
#22494 = CARTESIAN_POINT ( 'NONE',  ( -0.3000000000000000999, -3.751862894713570817, -0.4282819086714443890 ) ) ;
#22495 = EDGE_CURVE ( 'NONE', #32357, #26267, #9917, .T. ) ;
#22496 = CARTESIAN_POINT ( 'NONE',  ( 0.1353763015934749681, -0.5739868718191323271, 0.2449457213022636637 ) ) ;
#22497 = CARTESIAN_POINT ( 'NONE',  ( -0.02953079040095700838, 0.000000000000000000, 0.000000000000000000 ) ) ;
#22498 = EDGE_CURVE ( 'NONE', #652, #2027, #19846, .T. ) ;
#22499 = VECTOR ( 'NONE', #36946, 39.37007874015748854 ) ;
#22500 = CARTESIAN_POINT ( 'NONE',  ( -0.1443922129835726875, -0.5166151207188712791, 0.3750000000000001110 ) ) ;
#22501 = EDGE_CURVE ( 'NONE', #28743, #7643, #30637, .T. ) ;
#22502 = DIRECTION ( 'NONE',  ( -1.000000000000000000, -0.000000000000000000, -0.000000000000000000 ) ) ;
#22503 = EDGE_CURVE ( 'NONE', #17394, #10276, #23068, .T. ) ;
#22504 = DIRECTION ( 'NONE',  ( -1.000000000000000000, 0.000000000000000000, 0.000000000000000000 ) ) ;
#22505 = CARTESIAN_POINT ( 'NONE',  ( 0.2247355409086003175, -0.8309010600190726015, 0.4364284219733364223 ) ) ;
#22506 = APPLICATION_PROTOCOL_DEFINITION ( 'international standard', 'automotive_design', 2000, #21638 ) ;
#22507 = CIRCLE ( 'NONE', #23829, 0.1346589359789726881 ) ;
#22508 = AXIS2_PLACEMENT_3D ( 'NONE', #35395, #38871, #16676 ) ;
#22509 = DIRECTION ( 'NONE',  ( 0.000000000000000000, 0.000000000000000000, -1.000000000000000000 ) ) ;
#22510 = CIRCLE ( 'NONE', #9323, 0.5302738246768106123 ) ;
#22511 = CARTESIAN_POINT ( 'NONE',  ( -0.2399999999999999079, -3.941790907013290823, -0.4709369376873030477 ) ) ;
#22512 = CARTESIAN_POINT ( 'NONE',  ( -0.02953079040095627286, 0.09152108205202029445, 0.5223162075576441854 ) ) ;
#22513 = EDGE_CURVE ( 'NONE', #24668, #5937, #16715, .T. ) ;
#22514 = EDGE_LOOP ( 'NONE', ( #26026, #11419, #1941, #30665, #27085, #36424, #18796 ) ) ;
#22515 = CARTESIAN_POINT ( 'NONE',  ( 0.2117001771772084040, -1.293046366063226538, -0.4065196447463829132 ) ) ;
#22516 = CYLINDRICAL_SURFACE ( 'NONE', #28269, 0.1000000000000000056 ) ;
#22517 = CARTESIAN_POINT ( 'NONE',  ( 0.08760676156666630243, -0.6788582240935653322, 0.02273922730970788161 ) ) ;
#22518 = ORIENTED_EDGE ( 'NONE', *, *, #36623, .T. ) ;
#22519 = DIRECTION ( 'NONE',  ( 0.3468893892380646715, 0.3199132558031939078, 0.8816593788960921385 ) ) ;
#22520 = CARTESIAN_POINT ( 'NONE',  ( 0.1482163224994231254, -1.323752227822259542, 0.6994010967223863728 ) ) ;
#22522 = VERTEX_POINT ( 'NONE', #10737 ) ;
#22521 = ORIENTED_EDGE ( 'NONE', *, *, #13909, .T. ) ;
#22523 = CARTESIAN_POINT ( 'NONE',  ( 0.1625982857068778153, -0.6782215948270849948, 0.2386756342038218459 ) ) ;
#22524 = ORIENTED_EDGE ( 'NONE', *, *, #28279, .F. ) ;
#22525 = CARTESIAN_POINT ( 'NONE',  ( 0.7009661026058806588, -1.563056106223300823, -0.5155029497116575543 ) ) ;
#22526 = CARTESIAN_POINT ( 'NONE',  ( -0.1443922129835735757, -0.5166151207188711680, 0.08499999999999974243 ) ) ;
#22527 = AXIS2_PLACEMENT_3D ( 'NONE', #19797, #7655, #3400 ) ;
#22528 = DIRECTION ( 'NONE',  ( 0.000000000000000000, -0.3563057211773426602, -0.9343694307158671997 ) ) ;
#22529 = CARTESIAN_POINT ( 'NONE',  ( 0.04946426091937270592, -0.2513512500265240313, -0.4057590668656845256 ) ) ;
#22530 = EDGE_LOOP ( 'NONE', ( #34001, #33843 ) ) ;
#22531 = CARTESIAN_POINT ( 'NONE',  ( 0.008654831750343138300, -0.6462809503128671418, -0.007129606758741551496 ) ) ;
#22532 = EDGE_LOOP ( 'NONE', ( #12504, #20857, #39355, #39907 ) ) ;
#22533 = ORIENTED_EDGE ( 'NONE', *, *, #31662, .T. ) ;
#22534 = ADVANCED_FACE ( 'NONE', ( #29261 ), #32943, .F. ) ;
#22535 = CARTESIAN_POINT ( 'NONE',  ( 0.09006073176016128612, -0.5638610315313903332, 0.1703137466647555442 ) ) ;
#22536 = EDGE_CURVE ( 'NONE', #37901, #22853, #16416, .T. ) ;
#22537 = CIRCLE ( 'NONE', #34348, 0.2200000000000000011 ) ;
#22538 = FACE_OUTER_BOUND ( 'NONE', #11832, .T. ) ;
#22539 = AXIS2_PLACEMENT_3D ( 'NONE', #30597, #14341, #11258 ) ;
#22540 = CARTESIAN_POINT ( 'NONE',  ( 0.09462334978017705733, -0.6107534901994555732, 0.3586568835318235116 ) ) ;
#22542 = CARTESIAN_POINT ( 'NONE',  ( -0.02953079040095652960, 0.5250338024619264354, -0.07436286310882528339 ) ) ;
#22541 = CARTESIAN_POINT ( 'NONE',  ( 0.4513655011140282891, -1.638057308912242549, -0.4132293443021504697 ) ) ;
#22543 = CARTESIAN_POINT ( 'NONE',  ( 0.01364417761961938744, -0.8803303390833581155, 0.4681144232289236040 ) ) ;
#22544 = CARTESIAN_POINT ( 'NONE',  ( 0.3576271336300551607, -1.040820894166447630, 0.6313593842330901262 ) ) ;
#22545 = AXIS2_PLACEMENT_3D ( 'NONE', #9242, #21427, #15222 ) ;
#22546 = CARTESIAN_POINT ( 'NONE',  ( 0.4000000000034333314, -2.064900289389559607, -0.7181543511010001213 ) ) ;
#22547 = CARTESIAN_POINT ( 'NONE',  ( 0.1153471661799955333, -0.4465907051537503225, 0.1446142472693831005 ) ) ;
#22548 = CARTESIAN_POINT ( 'NONE',  ( -0.04211812644076726175, 0.2687274166943798837, -0.3844079338164257398 ) ) ;
#22549 = EDGE_CURVE ( 'NONE', #37283, #19840, #33550, .T. ) ;
#22550 = AXIS2_PLACEMENT_3D ( 'NONE', #40448, #25010, #15562 ) ;
#22551 = LINE ( 'NONE', #32186, #17910 ) ;
#22552 = EDGE_CURVE ( 'NONE', #24406, #40516, #125, .T. ) ;
#22553 = EDGE_CURVE ( 'NONE', #16305, #16916, #28717, .T. ) ;
#22554 = FACE_BOUND ( 'NONE', #23849, .T. ) ;
#22555 = EDGE_CURVE ( 'NONE', #33041, #990, #19400, .T. ) ;
#22556 = CARTESIAN_POINT ( 'NONE',  ( 0.5385451171429854744, -1.174625208511617114, 0.8096455807874475274 ) ) ;
#22557 = CARTESIAN_POINT ( 'NONE',  ( 0.5112813987709829977, -1.114248626770950823, 0.5535915447156093405 ) ) ;
#22558 = CARTESIAN_POINT ( 'NONE',  ( 0.02968583136207634046, -1.058910347371198268, 0.6069042338158797678 ) ) ;
#22559 = VECTOR ( 'NONE', #28773, 39.37007874015748143 ) ;
#22560 = CARTESIAN_POINT ( 'NONE',  ( 0.01548846960707360443, 0.4730347584886807066, -0.2341461249029813674 ) ) ;
#22561 = CARTESIAN_POINT ( 'NONE',  ( 0.1954870513704480839, -0.7169417872080507959, 0.3287089370885468154 ) ) ;
#22562 = CARTESIAN_POINT ( 'NONE',  ( 0.3385785554808135034, -1.058259937818618379, 0.7608351996376890858 ) ) ;
#22563 = CARTESIAN_POINT ( 'NONE',  ( 0.04155248107635910182, -0.01723053523177138849, 0.4699878081388675910 ) ) ;
#22564 = LINE ( 'NONE', #35096, #29157 ) ;
#22565 = VECTOR ( 'NONE', #30389, 39.37007874015748854 ) ;
#22566 = CONICAL_SURFACE ( 'NONE', #27168, 0.1600000000000007527, 1.047197551196599186 ) ;
#22567 = EDGE_CURVE ( 'NONE', #4940, #22989, #31147, .T. ) ;
#22568 = EDGE_LOOP ( 'NONE', ( #12155, #20699 ) ) ;
#22569 = CARTESIAN_POINT ( 'NONE',  ( 0.4657365369423695500, -1.116270101206942922, 0.5666720171803257822 ) ) ;
#22570 = CARTESIAN_POINT ( 'NONE',  ( 0.5953303036072959964, -1.457508885835639978, 0.6057417262805095959 ) ) ;
#22571 = EDGE_CURVE ( 'NONE', #18975, #25557, #8573, .T. ) ;
#22572 = CARTESIAN_POINT ( 'NONE',  ( -0.02000000000000000042, -2.577535374323032702, -0.2789082543815905035 ) ) ;
#22573 = CARTESIAN_POINT ( 'NONE',  ( 0.09075956982381812310, -1.322849663306714829, 0.4537812744180037550 ) ) ;
#22574 = ADVANCED_FACE ( 'NONE', ( #22393 ), #7685, .T. ) ;
#22575 = AXIS2_PLACEMENT_3D ( 'NONE', #21454, #27809, #40343 ) ;
#22576 = ORIENTED_EDGE ( 'NONE', *, *, #20493, .T. ) ;
#22577 = CARTESIAN_POINT ( 'NONE',  ( -0.1707812261971866086, 0.4977922652119593505, 0.3123933982393745090 ) ) ;
#22578 = VECTOR ( 'NONE', #12010, 39.37007874015748854 ) ;
#22579 = CARTESIAN_POINT ( 'NONE',  ( 0.1835632973924980760, -0.5276942279169911654, 0.2392151530743482357 ) ) ;
#22580 = CARTESIAN_POINT ( 'NONE',  ( 0.01548846960706677829, 0.5198120922912281561, -0.07362328916749191765 ) ) ;
#22581 = CARTESIAN_POINT ( 'NONE',  ( 0.06666666666664561314, -2.107936428766273629, -0.7005084057759866090 ) ) ;
#22582 = CARTESIAN_POINT ( 'NONE',  ( 0.4235506502418905916, -1.177630414603479281, 0.7006544390589145577 ) ) ;
#22584 = LINE ( 'NONE', #28536, #18799 ) ;
#22583 = CARTESIAN_POINT ( 'NONE',  ( -0.1399999999999997358, 0.000000000000000000, 0.000000000000000000 ) ) ;
#22585 = B_SPLINE_CURVE_WITH_KNOTS ( 'NONE', 3,
 ( #13184, #295, #25754, #23449, #691, #508, #3741, #35967, #16294, #22468, #28422, #25139, #32117, #13942, #7773, #3922 ),
 .UNSPECIFIED., .F., .F.,
 ( 4, 2, 2, 2, 2, 2, 2, 4 ),
 ( 0.000000000000000000, 0.0008266127476143557374, 0.001239919121421530299, 0.001446572308325117526, 0.001549898901776911465, 0.001601562198502808326, 0.001627393846865756539, 0.001653225495228704970 ),
 .UNSPECIFIED. ) ;
#22586 = CARTESIAN_POINT ( 'NONE',  ( 0.4471380481896147785, -1.057582006303192657, 0.6325253032963528144 ) ) ;
#22587 = ORIENTED_EDGE ( 'NONE', *, *, #20039, .F. ) ;
#22588 = DATE_TIME_ROLE ( 'classification_date' ) ;
#22589 = CARTESIAN_POINT ( 'NONE',  ( 0.09351869311172626709, -1.333801252570538942, 0.7037513887513892064 ) ) ;
#22590 = ORIENTED_EDGE ( 'NONE', *, *, #20029, .T. ) ;
#22591 = CARTESIAN_POINT ( 'NONE',  ( 0.03978348861078892518, -0.5859180147546816375, 0.3261096058830926236 ) ) ;
#22593 = CARTESIAN_POINT ( 'NONE',  ( 0.2008473531602258111, -0.6365206772495614063, 0.3321400968866717318 ) ) ;
#22592 = DIRECTION ( 'NONE',  ( 0.000000000000000000, 0.000000000000000000, -1.000000000000000000 ) ) ;
#22594 = DIRECTION ( 'NONE',  ( 1.000000000000000000, 1.445848444424219398E-15, -8.326672684688652360E-16 ) ) ;
#22595 = ORIENTED_EDGE ( 'NONE', *, *, #33089, .T. ) ;
#22596 = AXIS2_PLACEMENT_3D ( 'NONE', #37235, #21613, #21812 ) ;
#22597 = ORIENTED_EDGE ( 'NONE', *, *, #22732, .F. ) ;
#22598 = DIRECTION ( 'NONE',  ( 0.8543860900384366852, 0.5196387294542549329, -1.017227249256228896E-13 ) ) ;
#22599 = CARTESIAN_POINT ( 'NONE',  ( 0.1167732631504307256, -0.5657854654953510254, 0.2312607435301864134 ) ) ;
#22600 = EDGE_LOOP ( 'NONE', ( #25991, #28495, #11225, #21249 ) ) ;
#22601 = CARTESIAN_POINT ( 'NONE',  ( 0.07043814880409834944, -1.334972480813817031, 0.5056242588139941985 ) ) ;
#22602 = CARTESIAN_POINT ( 'NONE',  ( -0.004773644027431071801, -1.959412267866362356, -0.3319689416633392898 ) ) ;
#22603 = DIRECTION ( 'NONE',  ( -1.000000000000000000, -2.341930812374887555E-31, 1.664003471950578127E-31 ) ) ;
#22604 = AXIS2_PLACEMENT_3D ( 'NONE', #29579, #24045, #17237 ) ;
#22605 = DIRECTION ( 'NONE',  ( 7.771561172376107616E-16, -7.170354002788761615E-17, 1.000000000000000000 ) ) ;
#22606 = PRODUCT_DEFINITION_SHAPE ( 'NONE', 'NONE',  #40563 ) ;
#22607 = DIRECTION ( 'NONE',  ( 1.000000000000000000, 2.280301054154495132E-31, -1.664003471950577689E-31 ) ) ;
#22608 = ADVANCED_FACE ( 'NONE', ( #10433, #13112 ), #1021, .F. ) ;
#22609 = CARTESIAN_POINT ( 'NONE',  ( 0.4079495573748788129, -1.708779812455338165, 0.6204884880800459745 ) ) ;
#22610 = DIRECTION ( 'NONE',  ( 0.5257402267398344486, 0.3034999571474336633, -0.7946602984917855439 ) ) ;
#22611 = VECTOR ( 'NONE', #17983, 39.37007874015748854 ) ;
#22612 = CARTESIAN_POINT ( 'NONE',  ( 0.06980746140711582837, 7.160938508832261116E-17, 0.2149999999999999967 ) ) ;
#22613 = DIRECTION ( 'NONE',  ( -0.4999551463232372317, 0.8660512985181135770, -0.000000000000000000 ) ) ;
#22614 = AXIS2_PLACEMENT_3D ( 'NONE', #29038, #27884, #10119 ) ;
#22615 = DIRECTION ( 'NONE',  ( 1.000000000000000000, 0.000000000000000000, 0.000000000000000000 ) ) ;
#22616 = CARTESIAN_POINT ( 'NONE',  ( 0.1034728371066890584, -1.383544289075226974, 0.6669953293747845624 ) ) ;
#22617 = PERSON_AND_ORGANIZATION ( #28500, #32463 ) ;
#22618 = DIRECTION ( 'NONE',  ( 0.9998941247116546194, -0.01455087607601020412, 0.0001066420868422379362 ) ) ;
#22619 = DIRECTION ( 'NONE',  ( 1.000000000000000000, -1.671477276948176127E-11, -5.600159359328265480E-12 ) ) ;
#22620 = CARTESIAN_POINT ( 'NONE',  ( 0.7062706752423565382, -1.445327451526715823, 0.7203384021836691797 ) ) ;
#22621 = CARTESIAN_POINT ( 'NONE',  ( 0.2590435573837815419, -1.679512851806065576, 0.5266323208858617599 ) ) ;
#22622 = DIRECTION ( 'NONE',  ( 1.188678714063518227E-15, -1.000000000000000000, -3.263080277421930985E-16 ) ) ;
#22623 = CARTESIAN_POINT ( 'NONE',  ( 0.01037466073212112323, -0.7737952308255096057, 0.4846566707863347867 ) ) ;
#22624 = CARTESIAN_POINT ( 'NONE',  ( -1.643206837334582843E-05, -0.7039665126479284218, -0.1033155573469211747 ) ) ;
#22625 = ADVANCED_FACE ( 'NONE', ( #6727 ), #9922, .T. ) ;
#22626 = AXIS2_PLACEMENT_3D ( 'NONE', #10010, #13298, #19878 ) ;
#22627 = CARTESIAN_POINT ( 'NONE',  ( 0.4115766028365042128, -1.733048369835246794, 0.5182417262812423209 ) ) ;
#22628 = FACE_OUTER_BOUND ( 'NONE', #25047, .T. ) ;
#22629 = EDGE_CURVE ( 'NONE', #22416, #12314, #32594, .T. ) ;
#22630 = ORIENTED_EDGE ( 'NONE', *, *, #18289, .F. ) ;
#22631 = VECTOR ( 'NONE', #5231, 39.37007874015748143 ) ;
#22632 = EDGE_LOOP ( 'NONE', ( #16003, #7812, #31991, #31115 ) ) ;
#22633 = TOROIDAL_SURFACE ( 'NONE', #35760, 0.08830708661417342731, 0.01499999999999999944 ) ;
#22634 = CARTESIAN_POINT ( 'NONE',  ( 0.05634307799789382148, -0.2780413953411557948, -0.3652007531760622094 ) ) ;
#22635 = VERTEX_POINT ( 'NONE', #4847 ) ;
#22636 = CARTESIAN_POINT ( 'NONE',  ( 0.4234909963964843538, -1.082397635545747638, -0.5155029497116575543 ) ) ;
#22637 = CARTESIAN_POINT ( 'NONE',  ( 0.3447453106071770579, -1.668772187017560915, -0.4515255377999706221 ) ) ;
#22638 = CARTESIAN_POINT ( 'NONE',  ( 0.5982972540623748836, -1.463353734898567238, 0.5950316300567694006 ) ) ;
#22640 = ORIENTED_EDGE ( 'NONE', *, *, #4146, .F. ) ;
#22639 = DIRECTION ( 'NONE',  ( 7.771561172376107616E-16, -7.170354002788761615E-17, 1.000000000000000000 ) ) ;
#22641 = AXIS2_PLACEMENT_3D ( 'NONE', #26743, #17262, #20167 ) ;
#22642 = EDGE_LOOP ( 'NONE', ( #3213, #39906 ) ) ;
#22643 = CARTESIAN_POINT ( 'NONE',  ( 0.1996512133853552973, -0.6037243375952904278, 0.3287643322477424301 ) ) ;
#22644 = ORIENTED_EDGE ( 'NONE', *, *, #4864, .F. ) ;
#22645 = AXIS2_PLACEMENT_3D ( 'NONE', #26752, #20174, #35792 ) ;
#22646 = CARTESIAN_POINT ( 'NONE',  ( 0.2811029688069974775, -1.576922886774730026, 0.8430380186458928948 ) ) ;
#22648 = CARTESIAN_POINT ( 'NONE',  ( 0.1909286924077255032, -1.257064795538239022, -0.3194753470178354759 ) ) ;
#22647 = CARTESIAN_POINT ( 'NONE',  ( 0.5271998568634933546, -1.674914755915226205, -0.4628290575799461348 ) ) ;
#22649 = FACE_OUTER_BOUND ( 'NONE', #9856, .T. ) ;
#22650 = DIRECTION ( 'NONE',  ( -1.000000000000000000, -7.857794173099924470E-32, -8.628166150854818811E-32 ) ) ;
#22651 = CARTESIAN_POINT ( 'NONE',  ( 0.003300408388875467319, -1.849130736997417479, -0.3506394244204662503 ) ) ;
#22653 = ORIENTED_EDGE ( 'NONE', *, *, #22279, .T. ) ;
#22652 = ORIENTED_EDGE ( 'NONE', *, *, #19260, .F. ) ;
#22654 = CARTESIAN_POINT ( 'NONE',  ( -0.1710642718812833418, 0.4986889572247755753, 0.1528658435937000626 ) ) ;
#22655 = CARTESIAN_POINT ( 'NONE',  ( 0.1863396098874236240, -0.9154215460517445280, 0.1638900048413362009 ) ) ;
#22656 = CARTESIAN_POINT ( 'NONE',  ( -0.01895494625228214686, -0.07381100255646640129, -0.5147985126481153806 ) ) ;
#22657 = CARTESIAN_POINT ( 'NONE',  ( 0.5952542337618718093, -1.458258124885792872, 0.5925654897410345123 ) ) ;
#22658 = CARTESIAN_POINT ( 'NONE',  ( 0.2663031117850838680, -1.076423138501223509, 0.7428620000047612137 ) ) ;
#22659 = CYLINDRICAL_SURFACE ( 'NONE', #10644, 0.1000000000000000194 ) ;
#22660 = AXIS2_PLACEMENT_3D ( 'NONE', #18361, #9297, #21875 ) ;
#22661 = EDGE_CURVE ( 'NONE', #19455, #33728, #25055, .T. ) ;
#22662 = CARTESIAN_POINT ( 'NONE',  ( 0.1840595033465176056, -0.8547675690073376353, 0.1457166466292989515 ) ) ;
#22663 = CIRCLE ( 'NONE', #333, 0.1033070866141732325 ) ;
#22664 = VECTOR ( 'NONE', #25025, 39.37007874015748143 ) ;
#22665 = CARTESIAN_POINT ( 'NONE',  ( 0.005980720888701209978, -0.8455916207747946611, 0.1457185332388707122 ) ) ;
#22666 = DIRECTION ( 'NONE',  ( 0.8660512985181130219, 0.4999551463232377868, 0.000000000000000000 ) ) ;
#22667 = VECTOR ( 'NONE', #20296, 39.37007874015748143 ) ;
#22668 = DIRECTION ( 'NONE',  ( 1.000000000000000000, 1.049121689386595374E-11, -1.416614914756797075E-11 ) ) ;
#22669 = FACE_OUTER_BOUND ( 'NONE', #24491, .T. ) ;
#22670 = CARTESIAN_POINT ( 'NONE',  ( 0.03875673594170116892, -0.3062691647558810071, 0.3649083695375496816 ) ) ;
#22671 = CARTESIAN_POINT ( 'NONE',  ( 0.2920835003669574048, -1.623987781970284594, 0.9481157836879084977 ) ) ;
#22672 = AXIS2_PLACEMENT_3D ( 'NONE', #11797, #24568, #14467 ) ;
#22673 = CARTESIAN_POINT ( 'NONE',  ( 0.1102619990977181802, -1.417135361233744728, 0.5934404726580401190 ) ) ;
#22674 = APPLICATION_PROTOCOL_DEFINITION ( 'international standard', 'automotive_design', 2000, #17419 ) ;
#22675 = DIRECTION ( 'NONE',  ( 0.000000000000000000, 0.9343694307158671997, -0.3563057211773426602 ) ) ;
#22676 = CARTESIAN_POINT ( 'NONE',  ( 0.3710009529117821447, -1.739873908940936298, -0.4854938087489614196 ) ) ;
#22677 = CARTESIAN_POINT ( 'NONE',  ( -0.02242828275839765448, 0.5043161982042816405, 0.09034400517547079568 ) ) ;
#22678 = DIRECTION ( 'NONE',  ( 0.000000000000000000, 0.000000000000000000, -1.000000000000000000 ) ) ;
#22679 = EDGE_LOOP ( 'NONE', ( #1566, #19588, #16301, #10896 ) ) ;
#22680 = CARTESIAN_POINT ( 'NONE',  ( 0.1499999999999996336, 1.092739197465705287E-15, 0.5500000000000003775 ) ) ;
#22681 = ORIENTED_EDGE ( 'NONE', *, *, #19710, .F. ) ;
#22682 = CARTESIAN_POINT ( 'NONE',  ( 0.4441836334028865796, -1.145505455753590418, -0.6481113851292223949 ) ) ;
#22683 = CARTESIAN_POINT ( 'NONE',  ( 0.2687519046691748126, -1.687296055496309677, 0.6251195327720597827 ) ) ;
#22684 = CIRCLE ( 'NONE', #10830, 0.03749999999977554621 ) ;
#22685 = CARTESIAN_POINT ( 'NONE',  ( 0.5948985926855137052, -1.487191034969570502, 0.5724586774276513301 ) ) ;
#22686 = EDGE_CURVE ( 'NONE', #29183, #37390, #20442, .T. ) ;
#22688 = EDGE_LOOP ( 'NONE', ( #15128, #24596, #25658, #27223 ) ) ;
#22687 = DIRECTION ( 'NONE',  ( -0.4999551463232372317, 0.8660512985181134660, 6.869252350113302335E-17 ) ) ;
#22689 = VECTOR ( 'NONE', #40587, 39.37007874015748143 ) ;
#22691 = VERTEX_POINT ( 'NONE', #13907 ) ;
#22690 = ORIENTED_EDGE ( 'NONE', *, *, #7273, .T. ) ;
#22692 = DIRECTION ( 'NONE',  ( 0.000000000000000000, 0.5877852522924426060, -0.8090169943749696557 ) ) ;
#22693 = VECTOR ( 'NONE', #26861, 39.37007874015748143 ) ;
#22694 = ORIENTED_EDGE ( 'NONE', *, *, #21600, .F. ) ;
#22695 = CYLINDRICAL_SURFACE ( 'NONE', #29820, 0.06250000000000001388 ) ;
#22696 = LOCAL_TIME ( 0, 53, 7.000000000000000000, #38624 ) ;
#22697 = CARTESIAN_POINT ( 'NONE',  ( 0.6299594026003103586, -1.615593600444566569, -0.5387823540836409464 ) ) ;
#22698 = CARTESIAN_POINT ( 'NONE',  ( 0.0001922330474179282408, -0.9534082139883226503, 0.1483282180229331948 ) ) ;
#22699 = VERTEX_POINT ( 'NONE', #36739 ) ;
#22700 = CARTESIAN_POINT ( 'NONE',  ( 0.1642392807452758841, -0.8691899957643679508, 0.5538582745929433448 ) ) ;
#22701 = AXIS2_PLACEMENT_3D ( 'NONE', #37663, #25339, #12369 ) ;
#22702 = CARTESIAN_POINT ( 'NONE',  ( 0.08990936761269098521, -0.5436479961250846316, 0.1460913089649385210 ) ) ;
#22703 = CARTESIAN_POINT ( 'NONE',  ( 0.1112219432785723217, -0.5687467704934952017, 0.2435113322008175263 ) ) ;
#22704 = EDGE_LOOP ( 'NONE', ( #8499, #2438, #35817, #29148 ) ) ;
#22705 = CARTESIAN_POINT ( 'NONE',  ( 0.5895803812855957560, -1.594679580009012776, -0.5906415517346027544 ) ) ;
#22706 = CARTESIAN_POINT ( 'NONE',  ( -0.1593650814506418767, 0.4947962564849443523, 0.1029884207726652623 ) ) ;
#22707 = CARTESIAN_POINT ( 'NONE',  ( -0.05634304521267748805, 0.01028134608269738216, 0.4588823192046725952 ) ) ;
#22708 = CARTESIAN_POINT ( 'NONE',  ( 0.1048591973540500683, -1.410537849644770025, 0.5682417262808777680 ) ) ;
#22709 = CARTESIAN_POINT ( 'NONE',  ( 0.6944912789943821219, -1.426234547408998354, 0.6673110007802252053 ) ) ;
#22710 = CARTESIAN_POINT ( 'NONE',  ( 0.5401403459456773914, -1.597711863851910996, -0.5730363334735802949 ) ) ;
#22711 = CARTESIAN_POINT ( 'NONE',  ( 0.5955909224605128172, -1.457896359989123480, 0.6966997756915641604 ) ) ;
#22712 = CARTESIAN_POINT ( 'NONE',  ( 0.01176895705049121714, -0.6529346896220689089, -0.1114654361404705807 ) ) ;
#22713 = AXIS2_PLACEMENT_3D ( 'NONE', #4310, #23048, #1451 ) ;
#22714 = CARTESIAN_POINT ( 'NONE',  ( 0.2322138788700108258, -1.233113307957229177, 0.3157417262808777658 ) ) ;
#22715 = CIRCLE ( 'NONE', #10216, 0.3698489655878002824 ) ;
#22716 = CARTESIAN_POINT ( 'NONE',  ( 0.4278413765848551042, -1.120299553241070001, -0.3830631589809549431 ) ) ;
#22717 = CARTESIAN_POINT ( 'NONE',  ( 0.04965997019300262549, -1.266850117287420696, 0.6475152895583352608 ) ) ;
#22718 = CARTESIAN_POINT ( 'NONE',  ( 0.2182827306251404198, -0.8246641648518335810, 0.4150641157079975052 ) ) ;
#22719 = PRODUCT_CONTEXT ( 'NONE', #13202, 'mechanical' ) ;
#22720 = DIRECTION ( 'NONE',  ( -2.465190328815661892E-32, -1.000000000000000000, -6.656013887802287108E-31 ) ) ;
#22721 = LOCAL_TIME ( 0, 53, 7.000000000000000000, #13036 ) ;
#22722 = CARTESIAN_POINT ( 'NONE',  ( -0.2399999999999999079, -4.289222312108804225, -0.7308809693675260011 ) ) ;
#22723 = AXIS2_PLACEMENT_3D ( 'NONE', #13774, #17070, #26547 ) ;
#22724 = CARTESIAN_POINT ( 'NONE',  ( -0.05268850283020124620, -0.004611971649426341129, 0.4686124025367036650 ) ) ;
#22725 =( BOUNDED_SURFACE ( )  B_SPLINE_SURFACE ( 3, 2, ( 
 ( #5875, #15755, #28306 ),
 ( #18437, #30988, #12664 ),
 ( #2812, #27918, #15360 ),
 ( #22358, #37362, #31407 ),
 ( #37771, #24639, #9592 ),
 ( #22170, #34683, #6690 ),
 ( #9173, #25021, #6080 ),
 ( #6488, #8986, #21554 ),
 ( #36560, #28727, #31209 ),
 ( #3028, #15572, #12889 ),
 ( #34882, #37552, #9376 ),
 ( #21956, #19059, #34483 ),
 ( #25446, #37977, #19267 ),
 ( #31807, #3622, #16186 ),
 ( #588, #29117, #25851 ),
 ( #35297, #38764, #19862 ),
 ( #20080, #7090, #10208 ),
 ( #23168, #775, #4601 ),
 ( #979, #16787, #32397 ),
 ( #16981, #6897, #20279 ),
 ( #7285, #26445, #10813 ),
 ( #35480, #9993, #13493 ),
 ( #13281, #26059, #29521 ),
 ( #3814, #17177, #19470 ),
 ( #32195, #28909, #32609 ),
 ( #22775, #35093, #35697 ),
 ( #22562, #16370, #38169 ),
 ( #7501, #10397, #38369 ),
 ( #19659, #32003, #23388 ),
 ( #29723, #4010, #4220 ),
 ( #38578, #13082, #16573 ),
 ( #38981, #29334, #26243 ),
 ( #13680, #22960, #1180 ),
 ( #32800, #10595, #4421 ),
 ( #35904, #1361, #13870 ),
 ( #7712, #25637, #20690 ),
 ( #14907, #1567, #24370 ),
 ( #39796, #27465, #33222 ),
 ( #36096, #21293, #1966 ),
 ( #14702, #33004, #8110 ),
 ( #39582, #36708, #17595 ),
 ( #7901, #5226, #20472 ) ),
 .UNSPECIFIED., .F., .F., .T. ) 
 B_SPLINE_SURFACE_WITH_KNOTS ( ( 4, 2, 2, 2, 2, 2, 2, 2, 2, 2, 2, 2, 2, 2, 2, 2, 2, 2, 2, 2, 4 ),
 ( 3, 3 ),
 ( 0.007479710391323436854, 0.01100368895397634515, 0.01452766751662925432, 0.01628965679795570803, 0.01805164607928216175, 0.01981363536060861547, 0.02069463000127184232, 0.02157562464193507265, 0.02333761392326152984, 0.02421860856392475669, 0.02509960320458798355, 0.02598059784525121041, 0.02686159248591443727, 0.02774258712657766413, 0.02862358176724089098, 0.02950457640790411784, 0.03038557104856734470, 0.03214756032989379841, 0.03302855497055702527, 0.03390954961122025213, 0.03567153889254670585 ),
 ( 0.000000000000000000, 1.000000000000000000 ),
 .UNSPECIFIED. ) 
 GEOMETRIC_REPRESENTATION_ITEM ( )  RATIONAL_B_SPLINE_SURFACE ( (
 ( 1.000000000000000000, 0.7659916417601224659, 1.000000000000000000),
 ( 1.000000000000000000, 0.7660618423663158039, 1.000000000000000000),
 ( 1.000000000000000000, 0.7663819230775843483, 1.000000000000000000),
 ( 1.000000000000000000, 0.7675928100430011725, 1.000000000000000000),
 ( 1.000000000000000000, 0.7687294063333358629, 1.000000000000000000),
 ( 1.000000000000000000, 0.7716951888074965460, 1.000000000000000000),
 ( 1.000000000000000000, 0.7729019889268164967, 1.000000000000000000),
 ( 1.000000000000000000, 0.7757527099395760128, 1.000000000000000000),
 ( 1.000000000000000000, 0.7773719702424962685, 1.000000000000000000),
 ( 1.000000000000000000, 0.7807403279777797023, 1.000000000000000000),
 ( 1.000000000000000000, 0.7824602495331657304, 1.000000000000000000),
 ( 1.000000000000000000, 0.7843589238246971851, 1.000000000000000000),
 ( 1.000000000000000000, 0.7848581668868191974, 1.000000000000000000),
 ( 1.000000000000000000, 0.7852721754964663292, 1.000000000000000000),
 ( 1.000000000000000000, 0.7851778104893205601, 1.000000000000000000),
 ( 1.000000000000000000, 0.7835785179914779297, 1.000000000000000000),
 ( 1.000000000000000000, 0.7804117671199929385, 1.000000000000000000),
 ( 1.000000000000000000, 0.7725400516492265668, 1.000000000000000000),
 ( 1.000000000000000000, 0.7694933636094736240, 1.000000000000000000),
 ( 1.000000000000000000, 0.7633371169485945185, 1.000000000000000000),
 ( 1.000000000000000000, 0.7602722165944099109, 1.000000000000000000),
 ( 1.000000000000000000, 0.7547023054668801079, 1.000000000000000000),
 ( 1.000000000000000000, 0.7521850639428176999, 1.000000000000000000),
 ( 1.000000000000000000, 0.7476002769756485700, 1.000000000000000000),
 ( 1.000000000000000000, 0.7455123382604045279, 1.000000000000000000),
 ( 1.000000000000000000, 0.7415958813887417733, 1.000000000000000000),
 ( 1.000000000000000000, 0.7397619986562821159, 1.000000000000000000),
 ( 1.000000000000000000, 0.7361471414609971342, 1.000000000000000000),
 ( 1.000000000000000000, 0.7343594884252070409, 1.000000000000000000),
 ( 1.000000000000000000, 0.7309782830180014956, 1.000000000000000000),
 ( 1.000000000000000000, 0.7293746573561863400, 1.000000000000000000),
 ( 1.000000000000000000, 0.7264315972118717823, 1.000000000000000000),
 ( 1.000000000000000000, 0.7250888023308159624, 1.000000000000000000),
 ( 1.000000000000000000, 0.7216279031333409089, 1.000000000000000000),
 ( 1.000000000000000000, 0.7203114455652043224, 1.000000000000000000),
 ( 1.000000000000000000, 0.7183868100543469026, 1.000000000000000000),
 ( 1.000000000000000000, 0.7177772480437595304, 1.000000000000000000),
 ( 1.000000000000000000, 0.7162016412217627748, 1.000000000000000000),
 ( 1.000000000000000000, 0.7153339323267929872, 1.000000000000000000),
 ( 1.000000000000000000, 0.7125888713840239364, 1.000000000000000000),
 ( 1.000000000000000000, 0.7104034760854559538, 1.000000000000000000),
 ( 1.000000000000000000, 0.7083861251860454900, 1.000000000000000000) ) ) 
 REPRESENTATION_ITEM ( '' )  SURFACE ( )  );
#22726 = ORIENTED_EDGE ( 'NONE', *, *, #24087, .F. ) ;
#22727 = CARTESIAN_POINT ( 'NONE',  ( 0.4517177305807006937, -1.568671020668126914, 0.6057417262804751790 ) ) ;
#22728 = CARTESIAN_POINT ( 'NONE',  ( 0.002297679438261008168, -0.5200315581813911292, 0.1541446757893583930 ) ) ;
#22729 = DIRECTION ( 'NONE',  ( 0.000000000000000000, -0.5781348229923763959, 0.8159412518334722142 ) ) ;
#22730 = ORIENTED_EDGE ( 'NONE', *, *, #32103, .F. ) ;
#22731 = CARTESIAN_POINT ( 'NONE',  ( 0.1223045647424210181, -1.412159682085746271, 0.4849083929475432320 ) ) ;
#22732 = EDGE_CURVE ( 'NONE', #38394, #4902, #23793, .T. ) ;
#22733 = CARTESIAN_POINT ( 'NONE',  ( 0.6674886243000348607, -1.379560724353076306, 0.6935688206045713677 ) ) ;
#22735 = VERTEX_POINT ( 'NONE', #29978 ) ;
#22734 = ORIENTED_EDGE ( 'NONE', *, *, #23255, .F. ) ;
#22736 = EDGE_CURVE ( 'NONE', #29150, #37623, #7078, .T. ) ;
#22737 = FACE_OUTER_BOUND ( 'NONE', #25840, .T. ) ;
#22738 = CARTESIAN_POINT ( 'NONE',  ( 0.3590244010119321150, -1.770436742188270740, -0.4892477637902210019 ) ) ;
#22739 = CARTESIAN_POINT ( 'NONE',  ( 0.3895266417130452408, -1.699103805033106651, -0.5245809722717744705 ) ) ;
#22740 = ADVANCED_FACE ( 'NONE', ( #14130 ), #1813, .F. ) ;
#22741 = VECTOR ( 'NONE', #18619, 39.37007874015748143 ) ;
#22742 = CARTESIAN_POINT ( 'NONE',  ( 0.04047043078436068225, -0.2415826219374506978, -0.4392104278742940404 ) ) ;
#22743 = ORIENTED_EDGE ( 'NONE', *, *, #13928, .F. ) ;
#22744 = CARTESIAN_POINT ( 'NONE',  ( 0.09375000000000012490, -0.4427825420493726183, 0.1457185332388693244 ) ) ;
#22745 = ADVANCED_FACE ( 'NONE', ( #10852 ), #20311, .T. ) ;
#22746 = CARTESIAN_POINT ( 'NONE',  ( 0.09028630236563642275, -0.6068359833129397529, 0.1815368149905945694 ) ) ;
#22747 = B_SPLINE_CURVE_WITH_KNOTS ( 'NONE', 3,
 ( #6072, #34261, #9165, #40026, #40641, #21727 ),
 .UNSPECIFIED., .F., .F.,
 ( 4, 2, 4 ),
 ( 0.000000000000000000, 0.5000000000000000000, 1.000000000000000000 ),
 .UNSPECIFIED. ) ;
#22748 = CARTESIAN_POINT ( 'NONE',  ( 0.004052029362975025431, -0.4904197722336705589, 0.3777681374143450621 ) ) ;
#22749 = CARTESIAN_POINT ( 'NONE',  ( 0.08534804946041728291, -0.5449560838406929397, 0.1719968967555055850 ) ) ;
#22751 = CARTESIAN_POINT ( 'NONE',  ( -0.1127323924368017344, -0.5155369761421052521, 0.3191796960528185401 ) ) ;
#22750 = CARTESIAN_POINT ( 'NONE',  ( 0.4747730085490121654, -1.591067186900658070, -0.4394709153640856125 ) ) ;
#22752 = CARTESIAN_POINT ( 'NONE',  ( 0.02261441518021851602, -0.9148528262931132637, 0.5668782753494319149 ) ) ;
#22753 = CARTESIAN_POINT ( 'NONE',  ( 0.1478010146435930483, -0.9292797905990020091, 0.2962792169381038287 ) ) ;
#22754 = APPLIED_SECURITY_CLASSIFICATION_ASSIGNMENT ( #22077, ( #17475 ) ) ;
#22755 = ORIENTED_EDGE ( 'NONE', *, *, #26886, .T. ) ;
#22756 = B_SPLINE_CURVE_WITH_KNOTS ( 'NONE', 3,
 ( #9296, #38452, #22852, #21873, #34402, #35371, #6217, #18784, #35976, #7580, #20763, #29802, #39263, #26315, #5093, #13750, #17251, #20351 ),
 .UNSPECIFIED., .F., .F.,
 ( 4, 2, 2, 2, 2, 2, 2, 2, 4 ),
 ( -0.003133633995111210699, -0.002350221109836731284, -0.001566808224562251869, -0.0007833953392877724548, 1.754598670695994844E-08, 0.0007834304312611863746, 0.001566843316535665789, 0.002350256201810145204, 0.003133669087084624619 ),
 .UNSPECIFIED. ) ;
#22757 = EDGE_LOOP ( 'NONE', ( #3446, #36205, #30823, #13738 ) ) ;
#22758 = CARTESIAN_POINT ( 'NONE',  ( 0.3762269255763664999, -1.611863304361743854, 0.5413035033958920605 ) ) ;
#22759 = CARTESIAN_POINT ( 'NONE',  ( 0.4352673078179172816, -1.693613930004312262, -0.5063126144843520526 ) ) ;
#22760 = CIRCLE ( 'NONE', #37833, 0.08000000000000002942 ) ;
#22761 = CARTESIAN_POINT ( 'NONE',  ( -0.05137569054208679376, 0.2953118892970998943, -0.3683837247633647283 ) ) ;
#22762 = EDGE_CURVE ( 'NONE', #16145, #39882, #5317, .T. ) ;
#22763 = APPROVAL ( #6949, 'UNSPECIFIED' ) ;
#22764 = CARTESIAN_POINT ( 'NONE',  ( -0.04308449196697855532, -0.4494173824501559444, -0.2058378951121007383 ) ) ;
#22765 = B_SPLINE_CURVE_WITH_KNOTS ( 'NONE', 3,
 ( #25915, #13553, #21858, #29391, #38436, #19715, #34385, #26122, #10274, #1235, #82, #22837 ),
 .UNSPECIFIED., .F., .F.,
 ( 4, 2, 2, 2, 2, 4 ),
 ( 1.163687884334659274E-17, 0.0008294755721960583124, 0.001244213358294084162, 0.001658951144392109686, 0.002488426716588164420, 0.003317902288784219372 ),
 .UNSPECIFIED. ) ;
#22766 = CARTESIAN_POINT ( 'NONE',  ( 0.5394647426574938898, -1.171356344921436365, 0.5164463399402798860 ) ) ;
#22767 = ORIENTED_EDGE ( 'NONE', *, *, #34936, .F. ) ;
#22768 = CARTESIAN_POINT ( 'NONE',  ( 0.5691520580847880817, -1.222151117369431939, 0.8040585553043922973 ) ) ;
#22769 = DIRECTION ( 'NONE',  ( 0.9378410757839521494, 0.1072489841977705138, -0.3300784330442476655 ) ) ;
#22770 = CARTESIAN_POINT ( 'NONE',  ( 0.05183675104700934816, -1.280743812480995780, 0.6394744559116233296 ) ) ;
#22771 = CARTESIAN_POINT ( 'NONE',  ( 0.03170953572518750430, 0.4816881781209779723, -0.09938198567066169886 ) ) ;
#22772 = VECTOR ( 'NONE', #16262, 39.37007874015748143 ) ;
#22773 = CARTESIAN_POINT ( 'NONE',  ( 0.5129993572544877534, -1.641037272694954474, -0.6170790168603458303 ) ) ;
#22774 = VERTEX_POINT ( 'NONE', #11656 ) ;
#22775 = CARTESIAN_POINT ( 'NONE',  ( 0.3323313641875296764, -1.048848748898059124, 0.7591878350141942899 ) ) ;
#22776 = CARTESIAN_POINT ( 'NONE',  ( 0.01895494625228159868, -0.3623053290766977130, 0.3730957266516582438 ) ) ;
#22777 = CARTESIAN_POINT ( 'NONE',  ( 0.6894585631977647733, -1.505591693816618282, 0.4630974732098093738 ) ) ;
#22778 = APPROVAL_PERSON_ORGANIZATION ( #19184, #29739, #34612 ) ;
#22779 = EDGE_LOOP ( 'NONE', ( #32224, #22963, #6202, #608 ) ) ;
#22780 = CARTESIAN_POINT ( 'NONE',  ( 0.4792469954158677936, -1.117519082122008900, -0.6343516840475907914 ) ) ;
#22781 = CARTESIAN_POINT ( 'NONE',  ( 0.3780067941418981392, -1.616348147715449768, -0.3643140746640379790 ) ) ;
#22782 = FACE_OUTER_BOUND ( 'NONE', #30239, .T. ) ;
#22783 = CARTESIAN_POINT ( 'NONE',  ( -0.2399999999999999079, -1.804235510932644004, -0.05018601889714981862 ) ) ;
#22784 = AXIS2_PLACEMENT_3D ( 'NONE', #31750, #3567, #542 ) ;
#22785 = CARTESIAN_POINT ( 'NONE',  ( 0.1497070752459234155, -1.041491121288300681, 0.7282887345088536746 ) ) ;
#22786 = ORIENTED_EDGE ( 'NONE', *, *, #2098, .F. ) ;
#22787 = EDGE_CURVE ( 'NONE', #30962, #39909, #6643, .T. ) ;
#22788 = CARTESIAN_POINT ( 'NONE',  ( -0.1679391139942377487, 0.5216964164670698789, 0.3184569295944921774 ) ) ;
#22789 = FACE_OUTER_BOUND ( 'NONE', #10523, .T. ) ;
#22790 = DIRECTION ( 'NONE',  ( 0.9378410757839510392, 0.3470650033817896385, 0.000000000000000000 ) ) ;
#22791 = CARTESIAN_POINT ( 'NONE',  ( 0.1999999999999789724, -2.107936428766273629, -0.7005084057759867200 ) ) ;
#22792 = EDGE_CURVE ( 'NONE', #31508, #18074, #13214, .T. ) ;
#22793 = CARTESIAN_POINT ( 'NONE',  ( 0.4740991274768489583, -1.249207495721872840, 0.6570441671156094232 ) ) ;
#22795 = CARTESIAN_POINT ( 'NONE',  ( 0.3247324306351095924, -1.759421949583082734, 0.4854534786567432647 ) ) ;
#22794 = CARTESIAN_POINT ( 'NONE',  ( 0.01548846960707528191, -0.4638115001430989648, 0.2459753896937853235 ) ) ;
#22796 = CARTESIAN_POINT ( 'NONE',  ( 0.4929433234940127639, -1.082713786091526353, 0.5692160337251114255 ) ) ;
#22797 = ORIENTED_EDGE ( 'NONE', *, *, #28339, .T. ) ;
#22798 = APPROVAL_ROLE ( '' ) ;
#22799 = B_SPLINE_CURVE_WITH_KNOTS ( 'NONE', 3,
 ( #14534, #40453, #18242, #17632, #27315, #40031, #27097, #18036, #30179, #5264 ),
 .UNSPECIFIED., .F., .F.,
 ( 4, 2, 2, 2, 4 ),
 ( 0.001421410091499697263, 0.001776295181873945809, 0.002131180272248194355, 0.002486065362622442466, 0.002840950452996691012 ),
 .UNSPECIFIED. ) ;
#22800 = EDGE_CURVE ( 'NONE', #30067, #3878, #4639, .T. ) ;
#22801 = DIRECTION ( 'NONE',  ( 0.5147264766109145295, -0.8573544507820052285, 0.000000000000000000 ) ) ;
#22802 = EDGE_LOOP ( 'NONE', ( #3094, #21197, #24864, #29758 ) ) ;
#22803 = CARTESIAN_POINT ( 'NONE',  ( 0.05410802736446353872, -0.5974446213890977075, 0.3459503305939781725 ) ) ;
#22805 = CARTESIAN_POINT ( 'NONE',  ( 0.01128677947712186484, -0.9461986806730106059, 0.1457185332388702959 ) ) ;
#22804 = CARTESIAN_POINT ( 'NONE',  ( 0.06602991763110438450, -0.7534794085705573963, 0.01325795176106262310 ) ) ;
#22806 = CARTESIAN_POINT ( 'NONE',  ( 0.06727760473923048712, -0.6490144398117091429, 0.002857611472789892224 ) ) ;
#22807 = ORIENTED_EDGE ( 'NONE', *, *, #10168, .T. ) ;
#22808 = EDGE_LOOP ( 'NONE', ( #28876, #14975 ) ) ;
#22809 = CIRCLE ( 'NONE', #30689, 0.04749999999977550652 ) ;
#22810 = CARTESIAN_POINT ( 'NONE',  ( 0.4931437851155135443, -1.083180748979025498, 0.5665107511466522805 ) ) ;
#22811 = CARTESIAN_POINT ( 'NONE',  ( 0.1718176880793481076, -0.7513250685104085891, 0.5656676516626540918 ) ) ;
#22812 = EDGE_LOOP ( 'NONE', ( #17288, #6170, #36622, #29806 ) ) ;
#22813 = CARTESIAN_POINT ( 'NONE',  ( 0.06896958704128998419, -1.329019900465761905, 0.4989856710699280273 ) ) ;
#22814 = LINE ( 'NONE', #4045, #34466 ) ;
#22815 = ADVANCED_FACE ( 'NONE', ( #23613 ), #3015, .F. ) ;
#22816 = LOCAL_TIME ( 0, 53, 7.000000000000000000, #29453 ) ;
#22817 = CARTESIAN_POINT ( 'NONE',  ( -2.070754768975505034, -0.09959325338431362917, 0.09999999999999933942 ) ) ;
#22818 = CARTESIAN_POINT ( 'NONE',  ( 0.6984663268742642428, -1.558725849730709934, -0.5155029497116575543 ) ) ;
#22819 = CARTESIAN_POINT ( 'NONE',  ( 0.09999999999998167299, -1.869535141313860782, -0.3418892918993297059 ) ) ;
#22820 = CARTESIAN_POINT ( 'NONE',  ( 0.08750868709893994124, -0.6856954311291793003, 0.06271735481263093770 ) ) ;
#22821 = AXIS2_PLACEMENT_3D ( 'NONE', #34918, #9819, #6520 ) ;
#22822 = CARTESIAN_POINT ( 'NONE',  ( 0.7370562124357561418, -1.515684240363464941, 0.4449423861150900716 ) ) ;
#22823 = CARTESIAN_POINT ( 'NONE',  ( 0.1953801488688421129, -1.653727163013434920, -0.6877973177680917205 ) ) ;
#22824 = CARTESIAN_POINT ( 'NONE',  ( 0.06690724611807970235, -1.340115547279100428, 0.5315811339006457636 ) ) ;
#22825 = DIRECTION ( 'NONE',  ( 0.1010117037271631713, 0.05706541553526763705, -0.9932472874666826712 ) ) ;
#22826 = SHAPE_DEFINITION_REPRESENTATION ( #13717, #33020 ) ;
#22827 = B_SPLINE_CURVE_WITH_KNOTS ( 'NONE', 3,
 ( #249, #9663, #29193, #13351 ),
 .UNSPECIFIED., .F., .F.,
 ( 4, 4 ),
 ( 1.873907885762902204E-16, 0.0005779611142783052345 ),
 .UNSPECIFIED. ) ;
#22828 = DIRECTION ( 'NONE',  ( 0.8660512985181133550, 0.4999551463232372317, 0.000000000000000000 ) ) ;
#22829 = CARTESIAN_POINT ( 'NONE',  ( 0.1685272260733683414, -1.385079421489360474, 0.5084237370591300209 ) ) ;
#22830 = CARTESIAN_POINT ( 'NONE',  ( 0.1850180133982991526, -0.7563345632739647550, -0.01070758755936668249 ) ) ;
#22831 = CARTESIAN_POINT ( 'NONE',  ( 0.05999999999999990757, -0.3458405862425447119, -0.1052451372150005060 ) ) ;
#22832 = CARTESIAN_POINT ( 'NONE',  ( 0.2646723247128293655, -1.687375416948911244, 0.5682417262808783232 ) ) ;
#22833 = CARTESIAN_POINT ( 'NONE',  ( 0.09565263806948612335, -1.148840486724431953, 0.8358535653919648700 ) ) ;
#22834 = CARTESIAN_POINT ( 'NONE',  ( -0.0001800219140582012974, -0.8396310703285838617, -0.05215014162539268611 ) ) ;
#22835 = B_SPLINE_CURVE_WITH_KNOTS ( 'NONE', 3,
 ( #31415, #3217, #21748, #28916, #15765, #10000 ),
 .UNSPECIFIED., .F., .F.,
 ( 4, 2, 4 ),
 ( 0.000000000000000000, 0.5000000000000002220, 1.000000000000000000 ),
 .UNSPECIFIED. ) ;
#22836 = DIRECTION ( 'NONE',  ( 0.000000000000000000, 1.686145379822168900E-15, -1.000000000000000000 ) ) ;
#22837 = CARTESIAN_POINT ( 'NONE',  ( 0.4751758298663427693, -1.652426242819087010, -0.6334442537810193175 ) ) ;
#22838 = VECTOR ( 'NONE', #19167, 39.37007874015748143 ) ;
#22839 = CARTESIAN_POINT ( 'NONE',  ( 0.2073148280362371032, -1.247401114506933917, 0.4282226788861551725 ) ) ;
#22840 = ORIENTED_EDGE ( 'NONE', *, *, #32376, .T. ) ;
#22841 = ORIENTED_EDGE ( 'NONE', *, *, #13249, .F. ) ;
#22842 = ADVANCED_FACE ( 'NONE', ( #20927 ), #7181, .F. ) ;
#22843 = CARTESIAN_POINT ( 'NONE',  ( 0.04582713223189486401, -0.3361263728083079827, -0.3523178389613200179 ) ) ;
#22844 = ORIENTED_EDGE ( 'NONE', *, *, #33901, .T. ) ;
#22845 = CARTESIAN_POINT ( 'NONE',  ( -0.04229956186878661151, 0.008769846780145210130, 0.4686106502047103772 ) ) ;
#22846 = CARTESIAN_POINT ( 'NONE',  ( 0.3264244126186546802, -1.294301107126978767, -0.5166151207188711680 ) ) ;
#22847 = EDGE_CURVE ( 'NONE', #38602, #22431, #37506, .T. ) ;
#22848 = CARTESIAN_POINT ( 'NONE',  ( 0.5184242004029562256, -1.327098421978155640, 0.7590059521294971745 ) ) ;
#22850 = ORIENTED_EDGE ( 'NONE', *, *, #2018, .F. ) ;
#22849 = DIRECTION ( 'NONE',  ( 5.551115123125868984E-17, -5.531779426422974156E-16, -1.000000000000000000 ) ) ;
#22851 = CARTESIAN_POINT ( 'NONE',  ( 0.3219050788564604137, -0.8784703629548025194, 0.6443316309767920247 ) ) ;
#22852 = CARTESIAN_POINT ( 'NONE',  ( 0.03650581953630514798, 0.4542932396444852028, -0.2355374485430464515 ) ) ;
#22853 = VERTEX_POINT ( 'NONE', #14255 ) ;
#22854 = CARTESIAN_POINT ( 'NONE',  ( 0.5976280483195713922, -1.483999647174189862, -0.6415005453050633966 ) ) ;
#22855 = VERTEX_POINT ( 'NONE', #11371 ) ;
#22856 = CARTESIAN_POINT ( 'NONE',  ( 0.3272817739344252574, -1.639265242723384697, 0.5775048433984611984 ) ) ;
#22858 = DIRECTION ( 'NONE',  ( 1.000000000000000000, 0.000000000000000000, 0.000000000000000000 ) ) ;
#22857 = CARTESIAN_POINT ( 'NONE',  ( 0.6119653131825866232, -1.588158183054942496, 0.4221774592016356298 ) ) ;
#22859 = CARTESIAN_POINT ( 'NONE',  ( 0.3066658489686008293, -1.757170713505755710, 0.5393683295168898439 ) ) ;
#22860 = ADVANCED_FACE ( 'NONE', ( #36060 ), #3481, .T. ) ;
#22861 = CARTESIAN_POINT ( 'NONE',  ( 0.04930870543692147251, -1.485063399300671882, -0.3452542621255675348 ) ) ;
#22862 = VERTEX_POINT ( 'NONE', #30501 ) ;
#22863 = DIMENSIONAL_EXPONENTS ( 1.000000000000000000, 0.000000000000000000, 0.000000000000000000, 0.000000000000000000, 0.000000000000000000, 0.000000000000000000, 0.000000000000000000 ) ;
#22864 = CARTESIAN_POINT ( 'NONE',  ( 0.05999999999999990757, 0.000000000000000000, 0.000000000000000000 ) ) ;
#22865 = CARTESIAN_POINT ( 'NONE',  ( 0.2666607338143368588, -0.9575770305785957781, 0.5134922487128943391 ) ) ;
#22866 = DIRECTION ( 'NONE',  ( -1.000000000000000000, -2.341930812374887555E-31, 1.664003471950578127E-31 ) ) ;
#22867 = CARTESIAN_POINT ( 'NONE',  ( 0.5965761245944036784, -1.493465029535157029, 0.5182417262812423209 ) ) ;
#22868 = EDGE_CURVE ( 'NONE', #25611, #34346, #7859, .T. ) ;
#22869 = CARTESIAN_POINT ( 'NONE',  ( 0.1391441241210990831, -0.8698021353542626510, 0.5024695666797485138 ) ) ;
#22870 = CARTESIAN_POINT ( 'NONE',  ( 0.01057097757788910339, -0.5312311850581503681, 0.1694607747591961866 ) ) ;
#22871 = ADVANCED_FACE ( 'NONE', ( #23939 ), #35554, .T. ) ;
#22872 = DIRECTION ( 'NONE',  ( 0.3468893892380643384, -0.7770416411310734350, -0.5252371270030050665 ) ) ;
#22873 = EDGE_CURVE ( 'NONE', #5090, #8849, #39987, .T. ) ;
#22874 = CARTESIAN_POINT ( 'NONE',  ( -0.1646293987946891302, 0.5114631127588012971, 0.3384789781300878708 ) ) ;
#22875 = CYLINDRICAL_SURFACE ( 'NONE', #32411, 0.04330708661417322775 ) ;
#22876 = CYLINDRICAL_SURFACE ( 'NONE', #12613, 0.02999999999999998848 ) ;
#22877 = DIRECTION ( 'NONE',  ( 0.9378410757839554801, 0.1072489841977693065, 0.3300784330442383396 ) ) ;
#22878 = DATE_TIME_ROLE ( 'classification_date' ) ;
#22879 = CARTESIAN_POINT ( 'NONE',  ( 0.03171861681800964422, -0.3665016810530177804, 0.3753647833258587641 ) ) ;
#22880 = CARTESIAN_POINT ( 'NONE',  ( 0.1835961851041346959, -0.5126270562563732813, 0.08826789480522242992 ) ) ;
#22881 = CARTESIAN_POINT ( 'NONE',  ( 0.2161879510971927987, -1.277123080371499242, -0.7187326247832955817 ) ) ;
#22882 = DIRECTION ( 'NONE',  ( -1.000000000000000000, -0.000000000000000000, -0.000000000000000000 ) ) ;
#22883 = DIRECTION ( 'NONE',  ( 5.879757087911781259E-34, 0.5877852522924815748, 0.8090169943749412340 ) ) ;
#22884 = CARTESIAN_POINT ( 'NONE',  ( 0.3766954841305968360, -1.761798103149637029, -0.5753806683247417730 ) ) ;
#22885 = CARTESIAN_POINT ( 'NONE',  ( 0.4820730268389710194, -1.120100422993975275, 0.5182417262812748504 ) ) ;
#22886 = VERTEX_POINT ( 'NONE', #1744 ) ;
#22887 = CARTESIAN_POINT ( 'NONE',  ( 0.2613660211529243438, -1.686120988816170119, 0.5257579584705852627 ) ) ;
#22888 = EDGE_CURVE ( 'NONE', #36123, #9809, #11589, .T. ) ;
#22890 = VERTEX_POINT ( 'NONE', #26819 ) ;
#22889 = CARTESIAN_POINT ( 'NONE',  ( 0.1380264030324899749, -0.6050966432626355695, 0.3254296826921013741 ) ) ;
#22892 = EDGE_LOOP ( 'NONE', ( #30816, #15321, #9456, #38587 ) ) ;
#22891 = FACE_OUTER_BOUND ( 'NONE', #18879, .T. ) ;
#22893 = EDGE_CURVE ( 'NONE', #17370, #1876, #21253, .T. ) ;
#22895 = ORIENTED_EDGE ( 'NONE', *, *, #6998, .F. ) ;
#22894 = ORIENTED_EDGE ( 'NONE', *, *, #2442, .T. ) ;
#22896 = CARTESIAN_POINT ( 'NONE',  ( 0.5172910145215950939, -1.680634944466891323, -0.5803635445188605191 ) ) ;
#22897 = ORIENTED_EDGE ( 'NONE', *, *, #15988, .F. ) ;
#22898 = DIRECTION ( 'NONE',  ( -1.355854680848614260E-31, 3.330669073875470114E-16, 1.000000000000000000 ) ) ;
#22899 = CARTESIAN_POINT ( 'NONE',  ( 0.6511295279640840761, -1.603372484741562687, -0.5770581850489380216 ) ) ;
#22900 = PERSON_AND_ORGANIZATION ( #18660, #2416 ) ;
#22901 = CARTESIAN_POINT ( 'NONE',  ( 0.0003981076881877283497, -0.5275076572294771227, -0.1178596299512809226 ) ) ;
#22902 = ORIENTED_EDGE ( 'NONE', *, *, #20575, .F. ) ;
#22903 = CARTESIAN_POINT ( 'NONE',  ( 0.08507626058706400929, -0.7891241300377995760, 0.1593484486019202950 ) ) ;
#22904 = CIRCLE ( 'NONE', #32734, 0.01000000000000002970 ) ;
#22905 = CARTESIAN_POINT ( 'NONE',  ( 0.08991945692117814248, -0.5437780353368280029, 0.1532396220041035706 ) ) ;
#22906 = CARTESIAN_POINT ( 'NONE',  ( 0.1110044217621600354, -0.5667795212461463894, 0.2377383413596886597 ) ) ;
#22907 = ORIENTED_EDGE ( 'NONE', *, *, #18808, .T. ) ;
#22908 = CARTESIAN_POINT ( 'NONE',  ( 0.1766140053765036799, -0.4884607529735562892, 0.1457336358543773192 ) ) ;
#22909 = CARTESIAN_POINT ( 'NONE',  ( 0.5848508152300195828, -1.486263022089187036, 0.6467108361231791447 ) ) ;
#22910 = CARTESIAN_POINT ( 'NONE',  ( -5.117090377708623197E-34, 0.08000000000000023759, -0.08769881541126035851 ) ) ;
#22911 = CARTESIAN_POINT ( 'NONE',  ( 0.4142925369596769380, -1.705023740597148008, 0.4226190609429597567 ) ) ;
#22912 = CARTESIAN_POINT ( 'NONE',  ( 0.4181400076792504139, -1.624779815497015001, -0.6506891825583066558 ) ) ;
#22913 = CARTESIAN_POINT ( 'NONE',  ( 0.4368279861777725204, -1.677667223885754844, 0.4182417262808776903 ) ) ;
#22914 = DIRECTION ( 'NONE',  ( 0.000000000000000000, -1.951319995474454795E-15, -1.000000000000000000 ) ) ;
#22915 = CARTESIAN_POINT ( 'NONE',  ( 0.1390279997722746186, -0.5963079674089665216, 0.3040810692042346108 ) ) ;
#22916 = CARTESIAN_POINT ( 'NONE',  ( 1.598725267176023850E-05, -0.6709277514742212345, -0.1033257619575898290 ) ) ;
#22917 =( LENGTH_UNIT ( ) NAMED_UNIT ( * ) SI_UNIT ( $, .METRE. ) );
#22918 = CARTESIAN_POINT ( 'NONE',  ( -0.1669433606228599432, 0.5138636982738122860, 0.1528658435937006732 ) ) ;
#22919 = CARTESIAN_POINT ( 'NONE',  ( 0.03868264068766581742, -0.4624969084406961306, -0.1149348357506052437 ) ) ;
#22920 = CARTESIAN_POINT ( 'NONE',  ( 0.1120276941441372132, -1.367097346105948130, 0.7195291715619951400 ) ) ;
#22921 = CARTESIAN_POINT ( 'NONE',  ( 0.2122887247597850247, -0.8188226314918697346, 0.3927370908608381339 ) ) ;
#22922 = APPROVAL_ROLE ( '' ) ;
#22923 = DIRECTION ( 'NONE',  ( 0.000000000000000000, 0.000000000000000000, -1.000000000000000000 ) ) ;
#22924 = DIRECTION ( 'NONE',  ( 0.000000000000000000, -0.9804888279246389837, -0.1965748160751215334 ) ) ;
#22925 = ORIENTED_EDGE ( 'NONE', *, *, #26502, .T. ) ;
#22926 = DIRECTION ( 'NONE',  ( 1.000000000000000000, 0.000000000000000000, 0.000000000000000000 ) ) ;
#22927 = CARTESIAN_POINT ( 'NONE',  ( 0.002367394983765751248, -0.5282119844061630154, 0.1467999231854355824 ) ) ;
#22928 = CARTESIAN_POINT ( 'NONE',  ( 0.1029498318846682331, -1.296234522660387967, 0.4455275691814166161 ) ) ;
#22929 = ORIENTED_EDGE ( 'NONE', *, *, #28342, .F. ) ;
#22930 = CARTESIAN_POINT ( 'NONE',  ( 0.1438070510857625550, -1.283988175806205723, 0.3667417262808778111 ) ) ;
#22931 = CARTESIAN_POINT ( 'NONE',  ( 0.6265937217076796850, -1.312621381056858993, 0.7675331558851111735 ) ) ;
#22933 = ORIENTED_EDGE ( 'NONE', *, *, #1657, .T. ) ;
#22932 = EDGE_LOOP ( 'NONE', ( #30287, #33132, #16766, #38828 ) ) ;
#22934 = DIRECTION ( 'NONE',  ( -1.000000000000000000, 0.000000000000000000, 0.000000000000000000 ) ) ;
#22935 = EDGE_LOOP ( 'NONE', ( #31292, #39165, #22652, #16391, #1896, #22120 ) ) ;
#22936 = CARTESIAN_POINT ( 'NONE',  ( -0.02587796518899032269, 0.000000000000000000, 0.000000000000000000 ) ) ;
#22937 = PRODUCT_DEFINITION_SHAPE ( 'NONE', 'NONE',  #11907 ) ;
#22938 = CARTESIAN_POINT ( 'NONE',  ( 0.3790029845727732605, -1.717173918479974803, -0.3392914156897724465 ) ) ;
#22939 = CARTESIAN_POINT ( 'NONE',  ( -0.02953079040095619306, 0.5250338024619283228, -0.07436286310882472828 ) ) ;
#22940 = ORIENTED_EDGE ( 'NONE', *, *, #9491, .F. ) ;
#22941 = CARTESIAN_POINT ( 'NONE',  ( 0.000000000000000000, -0.4262518876079541830, 0.1457185332388689636 ) ) ;
#22942 = CARTESIAN_POINT ( 'NONE',  ( 0.09222453600979922672, -0.6532506521049682435, 0.2501001928013826259 ) ) ;
#22943 = CARTESIAN_POINT ( 'NONE',  ( 0.01375146018318225069, -0.4678462169232188161, 0.3154892069967682455 ) ) ;
#22944 = CARTESIAN_POINT ( 'NONE',  ( 0.3831456390985862326, -1.321512013252764906, 0.8548773317760315349 ) ) ;
#22946 = CARTESIAN_POINT ( 'NONE',  ( 0.3512175092685453359, -1.737626439724724303, 0.4368660991148545780 ) ) ;
#22945 = CARTESIAN_POINT ( 'NONE',  ( 0.5010447282329528740, -1.606058451036832757, -0.4018775084353748972 ) ) ;
#22947 = CARTESIAN_POINT ( 'NONE',  ( 0.06593013508327637273, -0.9837097893939223958, 0.4880478824260481852 ) ) ;
#22948 = ORIENTED_EDGE ( 'NONE', *, *, #7608, .F. ) ;
#22949 = B_SPLINE_CURVE_WITH_KNOTS ( 'NONE', 3,
 ( #29302, #16542, #13250, #25817, #26028, #11596, #32773, #7868, #1754, #1938 ),
 .UNSPECIFIED., .F., .F.,
 ( 4, 2, 2, 2, 4 ),
 ( 9.931801139967757520E-05, 0.0004520544377635757880, 0.0008047908641274740009, 0.001157527290491372268, 0.001510263716855270427 ),
 .UNSPECIFIED. ) ;
#22950 = PLANE ( 'NONE',  #8837 ) ;
#22951 = CARTESIAN_POINT ( 'NONE',  ( 0.1922391936362386755, -0.4904811663640207819, 0.2844517592273411721 ) ) ;
#22952 = CARTESIAN_POINT ( 'NONE',  ( -0.05464101615137770263, -2.177105168660885326, -0.2518349584362399862 ) ) ;
#22953 = DIRECTION ( 'NONE',  ( 0.000000000000000000, 0.000000000000000000, 1.000000000000000000 ) ) ;
#22954 = CARTESIAN_POINT ( 'NONE',  ( 0.4845724100169539472, -1.091512197975673670, 0.8037230719241761356 ) ) ;
#22955 =( BOUNDED_SURFACE ( )  B_SPLINE_SURFACE ( 3, 2, ( 
 ( #14871, #36672, #2118 ),
 ( #27432, #24150, #39756 ),
 ( #27009, #17943, #39956 ),
 ( #30500, #8480, #14652 ),
 ( #36471, #17735, #11588 ),
 ( #21041, #11776, #20855 ) ),
 .UNSPECIFIED., .F., .F., .T. ) 
 B_SPLINE_SURFACE_WITH_KNOTS ( ( 4, 2, 4 ),
 ( 3, 3 ),
 ( -7.708135345285693774E-16, 0.0003922111778123613546, 0.0007844223556254935770 ),
 ( 0.000000000000000000, 1.000000000000000000 ),
 .UNSPECIFIED. ) 
 GEOMETRIC_REPRESENTATION_ITEM ( )  RATIONAL_B_SPLINE_SURFACE ( (
 ( 1.000000000000000000, 0.8959137433787442983, 1.000000000000000000),
 ( 1.000000000000000000, 0.9145433835206386863, 1.000000000000000000),
 ( 1.000000000000000000, 0.9368263804283851748, 1.000000000000000000),
 ( 1.000000000000000000, 0.9787315261369833319, 1.000000000000000000),
 ( 1.000000000000000000, 0.9990824601813189654, 1.000000000000000000),
 ( 1.000000000000000000, 1.000000000000000000, 1.000000000000000000) ) ) 
 REPRESENTATION_ITEM ( '' )  SURFACE ( )  );
#22956 = CARTESIAN_POINT ( 'NONE',  ( 0.5043831596453355326, -1.118121868638674687, 0.5040939098466322710 ) ) ;
#22957 = CARTESIAN_POINT ( 'NONE',  ( -0.01548846960688955027, -0.3772621329476795737, 0.3651003739306307172 ) ) ;
#22958 = CARTESIAN_POINT ( 'NONE',  ( 0.04308558661662140882, 0.4494156853470169244, -0.2058346122081022578 ) ) ;
#22959 = CARTESIAN_POINT ( 'NONE',  ( 0.5240124945691670977, -1.643385070224909095, -0.5720511728448423039 ) ) ;
#22960 = CARTESIAN_POINT ( 'NONE',  ( 0.3894760245852240677, -1.134673749242862018, 0.7271684844242152224 ) ) ;
#22961 = CARTESIAN_POINT ( 'NONE',  ( 0.03868264068766624070, -0.2522289290439759801, 0.4043438810462554045 ) ) ;
#22962 = CARTESIAN_POINT ( 'NONE',  ( -0.02872242845530504490, -0.2464193076120103354, -0.4721747535844858512 ) ) ;
#22963 = ORIENTED_EDGE ( 'NONE', *, *, #20545, .F. ) ;
#22964 = DIRECTION ( 'NONE',  ( 1.000000000000000000, 0.000000000000000000, 0.000000000000000000 ) ) ;
#22965 = DIRECTION ( 'NONE',  ( -1.000000000000000000, -7.857794173099924470E-32, -8.628166150854818811E-32 ) ) ;
#22966 = CARTESIAN_POINT ( 'NONE',  ( 0.3643499753119555651, -1.728436088122397241, -0.4712977219643614268 ) ) ;
#22967 = CARTESIAN_POINT ( 'NONE',  ( 0.3229289876128840775, -1.169687821100875658, 0.5631135379446852163 ) ) ;
#22968 = CARTESIAN_POINT ( 'NONE',  ( 0.1213752263504523504, -0.9708261959865926993, 0.6725932955394058332 ) ) ;
#22969 = ORIENTED_EDGE ( 'NONE', *, *, #4622, .T. ) ;
#22970 = CARTESIAN_POINT ( 'NONE',  ( -0.04155248107635989285, -0.2901916982059679073, -0.3701002694350356559 ) ) ;
#22971 = EDGE_CURVE ( 'NONE', #10166, #1535, #30943, .T. ) ;
#22972 = CARTESIAN_POINT ( 'NONE',  ( 0.3595715536228106801, -1.625401886829162423, -0.3696110269036073093 ) ) ;
#22973 = DIRECTION ( 'NONE',  ( -2.280301054154496008E-31, 1.000000000000000000, -3.330669073875470114E-16 ) ) ;
#22974 = APPROVAL ( #32955, 'UNSPECIFIED' ) ;
#22975 = CARTESIAN_POINT ( 'NONE',  ( 0.3969982963057278047, -1.750077671058422046, -0.4821875037442182599 ) ) ;
#22976 = CARTESIAN_POINT ( 'NONE',  ( 0.4058008863267686395, -1.155685782444805687, 0.7188585313195411386 ) ) ;
#22978 = FACE_OUTER_BOUND ( 'NONE', #28839, .T. ) ;
#22977 = CARTESIAN_POINT ( 'NONE',  ( -0.05634304521267782806, -2.731847993664263218E-15, -0.4588823192046729837 ) ) ;
#22979 = FACE_OUTER_BOUND ( 'NONE', #21468, .T. ) ;
#22980 = ORIENTED_EDGE ( 'NONE', *, *, #10314, .F. ) ;
#22981 = CALENDAR_DATE ( 2026, 13, 10 ) ;
#22982 = CARTESIAN_POINT ( 'NONE',  ( 0.01548846960707524721, 0.5198120922912040642, 0.07362328916749247276 ) ) ;
#22983 = EDGE_LOOP ( 'NONE', ( #37589, #28678, #6595, #37205, #36007, #6450 ) ) ;
#22984 = CARTESIAN_POINT ( 'NONE',  ( 0.04882066477899291851, -0.5577723668033041093, 0.2454755323597881955 ) ) ;
#22986 = CARTESIAN_POINT ( 'NONE',  ( 0.2018873067935590404, -0.6340018868387371498, 0.3403718512341859515 ) ) ;
#22985 = CARTESIAN_POINT ( 'NONE',  ( 0.06568576414414206699, -0.7783668077490022430, 0.02890612836029912355 ) ) ;
#22987 = DIRECTION ( 'NONE',  ( 7.771561172376107616E-16, -7.170354002788761615E-17, 1.000000000000000000 ) ) ;
#22988 = VERTEX_POINT ( 'NONE', #24151 ) ;
#22989 = VERTEX_POINT ( 'NONE', #36673 ) ;
#22990 = CARTESIAN_POINT ( 'NONE',  ( 0.4163860380882642431, -1.242336163338821464, 0.5827596682515493454 ) ) ;
#22991 = CARTESIAN_POINT ( 'NONE',  ( 0.1282033164738295428, -0.6133254681109230333, 0.3496213826538958624 ) ) ;
#22992 = ORIENTED_EDGE ( 'NONE', *, *, #5418, .F. ) ;
#22993 = CARTESIAN_POINT ( 'NONE',  ( 0.3841185810962554070, -1.843835201582077810, -0.5188048874333898164 ) ) ;
#22994 = CARTESIAN_POINT ( 'NONE',  ( 0.03643058821096724353, -0.4544345964805293625, 0.2356993163711000594 ) ) ;
#22995 = EDGE_CURVE ( 'NONE', #18407, #25557, #4673, .T. ) ;
#22996 = CARTESIAN_POINT ( 'NONE',  ( 0.1858438793772869690, -0.7993314817513539339, 0.1881562487493555480 ) ) ;
#22997 = ORIENTED_EDGE ( 'NONE', *, *, #13923, .T. ) ;
#22998 = CARTESIAN_POINT ( 'NONE',  ( 0.3621582553283898553, -1.735977488954054904, 0.6111894207627336373 ) ) ;
#22999 = CARTESIAN_POINT ( 'NONE',  ( 0.08596614173211629406, -0.8123625242870818886, 0.06126983391297252668 ) ) ;
#23000 = ADVANCED_FACE ( 'NONE', ( #17136, #29687 ), #1530, .F. ) ;
#23001 = CARTESIAN_POINT ( 'NONE',  ( 0.5961566725213064410, -1.266700452128206367, 0.8733730542187856383 ) ) ;
#23002 = EDGE_CURVE ( 'NONE', #28698, #18572, #10592, .T. ) ;
#23003 = CARTESIAN_POINT ( 'NONE',  ( 0.3996906523120555832, -1.748698433108215822, -0.4855307030469387941 ) ) ;
#23004 = CARTESIAN_POINT ( 'NONE',  ( 0.02999999999997886302, -2.107936428766274073, -0.7005084057759867200 ) ) ;
#23005 = DIRECTION ( 'NONE',  ( -1.000000000000000000, -2.280301054154495132E-31, 1.664003471950577689E-31 ) ) ;
#23006 = DATE_AND_TIME ( #10444, #39089 ) ;
#23007 = EDGE_CURVE ( 'NONE', #10513, #3992, #34574, .T. ) ;
#23008 = ADVANCED_FACE ( 'NONE', ( #40149 ), #18354, .T. ) ;
#23009 = B_SPLINE_CURVE_WITH_KNOTS ( 'NONE', 3,
 ( #39111, #1888, #36016, #16905, #20392, #23686, #33331, #19990, #4730, #29854, #14399, #29447, #14213, #8024, #20603, #5138 ),
 .UNSPECIFIED., .F., .F.,
 ( 4, 2, 2, 2, 2, 2, 2, 4 ),
 ( 0.000000000000000000, 0.0004900782238211935865, 0.0009801564476423871731, 0.001470234671463580651, 0.001960312895284774346, 0.002940469342927169976, 0.003430547566748366490, 0.003920625790569563437 ),
 .UNSPECIFIED. ) ;
#23010 = CARTESIAN_POINT ( 'NONE',  ( 0.6284438268168236474, -1.513958728249438668, -0.6343483574234501932 ) ) ;
#23011 = CARTESIAN_POINT ( 'NONE',  ( 0.04047170147976884153, 0.3430616206016774417, 0.3654769923554775923 ) ) ;
#23012 = DIRECTION ( 'NONE',  ( -7.000205099780314469E-17, -1.000000000000000000, 6.590151126658399604E-16 ) ) ;
#23013 = ADVANCED_FACE ( 'NONE', ( #12582 ), #30641, .F. ) ;
#23014 = CARTESIAN_POINT ( 'NONE',  ( 0.6960133515994678666, -1.427157319712460959, 0.5654899826020431952 ) ) ;
#23015 = LINE ( 'NONE', #25691, #288 ) ;
#23016 = B_SPLINE_CURVE_WITH_KNOTS ( 'NONE', 3,
 ( #14088, #5025, #29941, #20470, #26662, #8107, #4807, #17591, #39580, #20687, #11411, #7709, #38979, #1963, #20276, #32798, #29520, #23981, #33000, #1357, #1564, #17173, #26854, #39195 ),
 .UNSPECIFIED., .F., .F.,
 ( 4, 2, 2, 2, 2, 2, 2, 2, 2, 2, 2, 4 ),
 ( 0.000000000000000000, 0.001374078136085094080, 0.002061117204127640469, 0.002748156272170186858, 0.004122234408255279203, 0.005496312544340371115, 0.008244468816510554937, 0.01099262508868074049, 0.01374078136085092432, 0.01648893763302110640, 0.01923709390519129023, 0.02198525017736147058 ),
 .UNSPECIFIED. ) ;
#23017 = CARTESIAN_POINT ( 'NONE',  ( 0.001061621656357588511, -0.7083572002807602130, 0.2962098885571950446 ) ) ;
#23018 = CARTESIAN_POINT ( 'NONE',  ( 0.5939569629664056549, -1.553735267838222134, -0.5704756277538377551 ) ) ;
#23019 = CARTESIAN_POINT ( 'NONE',  ( -2.134683096299215379E-14, -2.097675824466504135, -0.2588528740066096678 ) ) ;
#23020 = DIRECTION ( 'NONE',  ( 0.8660512985181134660, 0.4999551463232372872, 0.000000000000000000 ) ) ;
#23021 = CARTESIAN_POINT ( 'NONE',  ( 0.02999999999997886302, -2.097675824466503691, -0.2907077406111384099 ) ) ;
#23022 = ORIENTED_EDGE ( 'NONE', *, *, #40637, .T. ) ;
#23023 = ORIENTED_EDGE ( 'NONE', *, *, #26606, .F. ) ;
#23024 = EDGE_CURVE ( 'NONE', #32680, #12748, #8894, .T. ) ;
#23025 = CARTESIAN_POINT ( 'NONE',  ( 0.4970273525888077026, -1.079783658718535877, 0.3157417262808778213 ) ) ;
#23026 = ORIENTED_EDGE ( 'NONE', *, *, #3181, .T. ) ;
#23027 = CARTESIAN_POINT ( 'NONE',  ( -0.3000000000000000999, -3.334889855281614857, -0.6641625420049475093 ) ) ;
#23028 = CARTESIAN_POINT ( 'NONE',  ( 0.4242133616548364183, -1.734366925052854391, -0.4397180493288433967 ) ) ;
#23029 = CARTESIAN_POINT ( 'NONE',  ( 0.4164969987651618299, -1.171307339976814799, 0.7723814282107528406 ) ) ;
#23030 = TOROIDAL_SURFACE ( 'NONE', #24343, 0.06434668806854092205, 0.005000000000000000104 ) ;
#23032 = ORIENTED_EDGE ( 'NONE', *, *, #1491, .F. ) ;
#23031 = CARTESIAN_POINT ( 'NONE',  ( -0.2399999999999999079, -3.840189043187996809, -0.1239867222638698224 ) ) ;
#23033 = CARTESIAN_POINT ( 'NONE',  ( 0.1860214731903934160, -0.7916887388224913558, 0.2098883466634208494 ) ) ;
#23034 = CARTESIAN_POINT ( 'NONE',  ( 0.3451885137985100105, -1.726073941889417096, -0.5819068695184340667 ) ) ;
#23035 = VERTEX_POINT ( 'NONE', #5796 ) ;
#23036 = FACE_OUTER_BOUND ( 'NONE', #1745, .T. ) ;
#23037 = EDGE_LOOP ( 'NONE', ( #40519, #3422, #1845, #13106 ) ) ;
#23038 = AXIS2_PLACEMENT_3D ( 'NONE', #25970, #509, #32118 ) ;
#23039 = CARTESIAN_POINT ( 'NONE',  ( 0.3262830249888155620, -1.638891270961440272, 0.5636674631656366508 ) ) ;
#23041 = CARTESIAN_POINT ( 'NONE',  ( -0.03664605387828207689, -0.2484618661253097660, 0.4118464167359232597 ) ) ;
#23040 = CARTESIAN_POINT ( 'NONE',  ( 0.03113248654051816583, 0.1428018198284763673, -0.1638325989215043410 ) ) ;
#23042 = CARTESIAN_POINT ( 'NONE',  ( 0.05567535398968421340, -1.335339640988971288, 0.4687417262808780127 ) ) ;
#23043 = CARTESIAN_POINT ( 'NONE',  ( 0.05999999999999990757, 0.6410130462957083219, -0.4300623794142590661 ) ) ;
#23044 = ORIENTED_EDGE ( 'NONE', *, *, #30840, .F. ) ;
#23045 = CARTESIAN_POINT ( 'NONE',  ( 0.3211485391366948883, -1.297382044030143344, 0.5018407269173935648 ) ) ;
#23046 = CARTESIAN_POINT ( 'NONE',  ( 0.1880962557479734509, -0.9163805599553175307, 0.2154166370166123168 ) ) ;
#23047 = FACE_OUTER_BOUND ( 'NONE', #35335, .T. ) ;
#23048 = DIRECTION ( 'NONE',  ( 1.000000000000000000, 0.000000000000000000, 0.000000000000000000 ) ) ;
#23049 = CARTESIAN_POINT ( 'NONE',  ( 0.2226181049683592650, -0.9993126311397080297, 0.7099361533374629607 ) ) ;
#23050 = CARTESIAN_POINT ( 'NONE',  ( 0.05236818520811117178, -0.8281183987458714535, 0.6957665626363849221 ) ) ;
#23051 = CARTESIAN_POINT ( 'NONE',  ( 0.1590165108039097164, -1.390942544176572371, -0.5155029497116575543 ) ) ;
#23052 = DIRECTION ( 'NONE',  ( 0.000000000000000000, 0.000000000000000000, -1.000000000000000000 ) ) ;
#23053 = ADVANCED_FACE ( 'NONE', ( #28426 ), #772, .F. ) ;
#23054 = DIRECTION ( 'NONE',  ( 1.000000000000000000, 2.341930812374887555E-31, -1.664003471950578127E-31 ) ) ;
#23055 = CARTESIAN_POINT ( 'NONE',  ( -0.05464101615137795936, -1.518907846805490403, -0.1889969338327479598 ) ) ;
#23056 = CYLINDRICAL_SURFACE ( 'NONE', #29219, 0.4615209409081864611 ) ;
#23057 =( LENGTH_UNIT ( ) NAMED_UNIT ( * ) SI_UNIT ( $, .METRE. ) );
#23058 = EDGE_CURVE ( 'NONE', #1932, #11795, #30302, .T. ) ;
#23059 = CIRCLE ( 'NONE', #18423, 0.06000000000000038636 ) ;
#23060 = CARTESIAN_POINT ( 'NONE',  ( 0.05838938100891326310, -1.295898982425970125, 0.6424779078687598011 ) ) ;
#23061 = EDGE_CURVE ( 'NONE', #35558, #553, #2930, .T. ) ;
#23062 = CARTESIAN_POINT ( 'NONE',  ( 0.1766140053765036799, -0.4884607529735562892, 0.1457336358543773192 ) ) ;
#23063 = CARTESIAN_POINT ( 'NONE',  ( 0.1013956804831029068, -1.380631438172658543, 0.6556088357230328567 ) ) ;
#23064 = AXIS2_PLACEMENT_3D ( 'NONE', #31875, #19721, #16431 ) ;
#23065 = ORIENTED_EDGE ( 'NONE', *, *, #12716, .F. ) ;
#23066 = CARTESIAN_POINT ( 'NONE',  ( -0.2399999999999999079, -2.511040369707300268, -0.4948468226404901804 ) ) ;
#23067 = CARTESIAN_POINT ( 'NONE',  ( -0.06908312040360534145, -0.09959325338431372632, 0.3602693341844387942 ) ) ;
#23068 = CIRCLE ( 'NONE', #32879, 0.03000000000000000583 ) ;
#23069 = CARTESIAN_POINT ( 'NONE',  ( 0.3086540466703007191, -1.716681333513715657, 0.8049923379735365314 ) ) ;
#23070 = DIRECTION ( 'NONE',  ( 8.881784197001246407E-16, -2.361472542561082612E-16, 1.000000000000000000 ) ) ;
#23071 = ORIENTED_EDGE ( 'NONE', *, *, #22661, .T. ) ;
#23072 = EDGE_CURVE ( 'NONE', #14616, #34947, #27825, .T. ) ;
#23073 = EDGE_CURVE ( 'NONE', #6462, #29455, #38166, .T. ) ;
#23074 = DIRECTION ( 'NONE',  ( 0.000000000000000000, -0.8159412518334726583, -0.5781348229923756188 ) ) ;
#23075 = ORIENTED_EDGE ( 'NONE', *, *, #7909, .T. ) ;
#23076 = LINE ( 'NONE', #25552, #10537 ) ;
#23077 = ADVANCED_FACE ( 'NONE', ( #15485 ), #40566, .F. ) ;
#23078 = CARTESIAN_POINT ( 'NONE',  ( 0.6027046940806113362, -1.482916138156018748, 0.5916400363227261039 ) ) ;
#23080 = VERTEX_POINT ( 'NONE', #37468 ) ;
#23079 = CARTESIAN_POINT ( 'NONE',  ( 0.4950886493683288037, -1.678532471121934044, -0.4215530961782456010 ) ) ;
#23081 = EDGE_CURVE ( 'NONE', #16986, #2123, #11246, .T. ) ;
#23083 = ORIENTED_EDGE ( 'NONE', *, *, #40605, .F. ) ;
#23082 = ORIENTED_EDGE ( 'NONE', *, *, #39169, .T. ) ;
#23084 = CARTESIAN_POINT ( 'NONE',  ( 0.6539706967335917609, -1.516592165152658822, 0.7560619644851708232 ) ) ;
#23085 = EDGE_LOOP ( 'NONE', ( #15691, #34549 ) ) ;
#23086 = FACE_OUTER_BOUND ( 'NONE', #24642, .T. ) ;
#23087 = FACE_OUTER_BOUND ( 'NONE', #40426, .T. ) ;
#23088 = CARTESIAN_POINT ( 'NONE',  ( -0.2399999999999999079, -2.853330612949663170, -0.7088139570729240502 ) ) ;
#23089 = DATE_AND_TIME ( #3934, #35268 ) ;
#23090 = CIRCLE ( 'NONE', #25726, 0.07999999999999996003 ) ;
#23091 = CARTESIAN_POINT ( 'NONE',  ( 0.001266334362739574958, -0.6339827964191881993, -0.06462206035643804081 ) ) ;
#23093 = VERTEX_POINT ( 'NONE', #25144 ) ;
#23092 = ORIENTED_EDGE ( 'NONE', *, *, #3963, .F. ) ;
#23094 = VECTOR ( 'NONE', #17861, 39.37007874015748143 ) ;
#23095 = CARTESIAN_POINT ( 'NONE',  ( 0.09694425764873422502, -0.8015933583696732700, 0.3191342905503998240 ) ) ;
#23096 = CARTESIAN_POINT ( 'NONE',  ( -0.3000000000000000999, -2.861028283584748699, -0.4103205306338890690 ) ) ;
#23097 = CIRCLE ( 'NONE', #24412, 0.1020173459747799466 ) ;
#23098 = CARTESIAN_POINT ( 'NONE',  ( 0.1102974682193811340, -0.5579282852749359867, 0.2100915847438293294 ) ) ;
#23099 = VERTEX_POINT ( 'NONE', #22081 ) ;
#23100 = CARTESIAN_POINT ( 'NONE',  ( -0.2399999999999999079, -2.853330612949663170, -0.6088139570729240724 ) ) ;
#23101 = CYLINDRICAL_SURFACE ( 'NONE', #10004, 2.001674066779353556 ) ;
#23102 = AXIS2_PLACEMENT_3D ( 'NONE', #29132, #7515, #38994 ) ;
#23103 = DIRECTION ( 'NONE',  ( 0.4999551463232372317, -0.8660512985181135770, 0.000000000000000000 ) ) ;
#23104 = AXIS2_PLACEMENT_3D ( 'NONE', #10245, #28759, #26096 ) ;
#23105 = CARTESIAN_POINT ( 'NONE',  ( 0.4092943692574704251, -1.708139270546744415, 0.4222004656856017113 ) ) ;
#23106 = CARTESIAN_POINT ( 'NONE',  ( 0.3916862212415726519, -1.581131361642308608, -0.7187326247832954706 ) ) ;
#23107 = DIRECTION ( 'NONE',  ( -8.881784197001246407E-16, 2.361472542561082612E-16, -1.000000000000000000 ) ) ;
#23108 = CARTESIAN_POINT ( 'NONE',  ( -1.990949339309697573E-32, -3.491513147198971704E-33, 0.4614999999999880864 ) ) ;
#23109 = DIRECTION ( 'NONE',  ( 8.881784197001246407E-16, -2.361472542561082612E-16, 1.000000000000000000 ) ) ;
#23110 = CARTESIAN_POINT ( 'NONE',  ( 0.01175246436738983276, -0.6702937331852513170, -0.1131883302235354855 ) ) ;
#23111 = CARTESIAN_POINT ( 'NONE',  ( 0.5246674523321896988, -1.372085926420510971, 0.7928523263102306151 ) ) ;
#23112 =( NAMED_UNIT ( * ) SI_UNIT ( $, .STERADIAN. ) SOLID_ANGLE_UNIT ( ) );
#23113 = EDGE_CURVE ( 'NONE', #6212, #28462, #19355, .T. ) ;
#23114 = DIRECTION ( 'NONE',  ( 0.000000000000000000, -0.5877852522924689183, -0.8090169943749506709 ) ) ;
#23115 = AXIS2_PLACEMENT_3D ( 'NONE', #29753, #20505, #33039 ) ;
#23116 = CARTESIAN_POINT ( 'NONE',  ( 0.4667255516235201407, -1.094999438749613363, -0.3992978201560059559 ) ) ;
#23117 = ADVANCED_FACE ( 'NONE', ( #16483 ), #22472, .T. ) ;
#23118 = CARTESIAN_POINT ( 'NONE',  ( -0.003124719664520032511, -0.8057675726412022454, 0.1130684494947832019 ) ) ;
#23119 = CARTESIAN_POINT ( 'NONE',  ( 0.3472154721327633808, -0.9812419721698063535, 0.6178014265861627718 ) ) ;
#23120 = APPROVAL_DATE_TIME ( #39526, #28254 ) ;
#23121 = CIRCLE ( 'NONE', #5338, 0.5400000000000004796 ) ;
#23122 = CARTESIAN_POINT ( 'NONE',  ( 0.6929208297549553919, -1.429122597532291650, 0.5682417262808779901 ) ) ;
#23123 = CARTESIAN_POINT ( 'NONE',  ( -0.01548846960707477016, 0.3772621329472714558, -0.3651003739303416706 ) ) ;
#23124 = CIRCLE ( 'NONE', #26403, 0.2000000000000000666 ) ;
#23125 = ORIENTED_EDGE ( 'NONE', *, *, #26982, .F. ) ;
#23126 = DIRECTION ( 'NONE',  ( -0.4999551463232372317, 0.8660512985181135770, -0.000000000000000000 ) ) ;
#23127 = CARTESIAN_POINT ( 'NONE',  ( 0.01117138305292090204, -0.5571624402049411007, 0.2649020760849408185 ) ) ;
#23128 = AXIS2_PLACEMENT_3D ( 'NONE', #31321, #3129, #15668 ) ;
#23129 = CARTESIAN_POINT ( 'NONE',  ( 0.6466186708443523168, -1.438673711944949307, -0.6250000000000000000 ) ) ;
#23130 = VERTEX_POINT ( 'NONE', #35409 ) ;
#23131 = EDGE_CURVE ( 'NONE', #38042, #40606, #34227, .T. ) ;
#23132 = CARTESIAN_POINT ( 'NONE',  ( 0.3323167458231998661, -1.749637683294404056, 0.4593311801905495262 ) ) ;
#23133 = CARTESIAN_POINT ( 'NONE',  ( 0.5893014856854912331, -1.253657609334210665, 0.7958531859040811618 ) ) ;
#23135 = ORIENTED_EDGE ( 'NONE', *, *, #37835, .F. ) ;
#23134 = ORIENTED_EDGE ( 'NONE', *, *, #23073, .F. ) ;
#23136 = DIRECTION ( 'NONE',  ( 0.1109881770483700930, -0.4429139914152930846, -0.8896678148410526177 ) ) ;
#23137 = VERTEX_POINT ( 'NONE', #4128 ) ;
#23138 = CARTESIAN_POINT ( 'NONE',  ( 0.04293694706340183548, -0.07181688488226646572, -0.4893579783150012186 ) ) ;
#23139 = CARTESIAN_POINT ( 'NONE',  ( 0.3809420377884416564, -1.709537094523409628, -0.3376603513304489157 ) ) ;
#23140 = CARTESIAN_POINT ( 'NONE',  ( -0.01548846960707434342, 0.5203207976467951745, -0.08861466064782075325 ) ) ;
#23141 = ORIENTED_EDGE ( 'NONE', *, *, #25842, .F. ) ;
#23142 = FACE_OUTER_BOUND ( 'NONE', #15939, .T. ) ;
#23143 = CARTESIAN_POINT ( 'NONE',  ( 0.08789236658728763474, -0.6851542995134042302, 0.1774356670165384287 ) ) ;
#23144 = CARTESIAN_POINT ( 'NONE',  ( 0.01825373427587153111, -0.5918760537899200314, 0.5452743738062094669 ) ) ;
#23145 = CARTESIAN_POINT ( 'NONE',  ( 0.1049701980345018326, -0.6534432861451462404, 0.4406655119813854826 ) ) ;
#23147 = CARTESIAN_POINT ( 'NONE',  ( -0.1088121136105147380, -0.4964308608213456875, 0.09999999999999989453 ) ) ;
#23146 = CARTESIAN_POINT ( 'NONE',  ( 0.1145253369699427703, -0.4958736430966769193, -0.001267178298959518697 ) ) ;
#23148 = CARTESIAN_POINT ( 'NONE',  ( 0.2135674535618494740, -1.112065761644619233, 0.6472873446657533281 ) ) ;
#23149 = ORIENTED_EDGE ( 'NONE', *, *, #16842, .F. ) ;
#23150 = EDGE_LOOP ( 'NONE', ( #20811, #25856 ) ) ;
#23151 = AXIS2_PLACEMENT_3D ( 'NONE', #22817, #9633, #16405 ) ;
#23152 = DIRECTION ( 'NONE',  ( 0.8406598760563539496, 0.5415634522278213181, 1.230192937850935930E-12 ) ) ;
#23153 = CARTESIAN_POINT ( 'NONE',  ( 0.1159518160055648672, -0.4567671116231432071, 0.2228320516541739127 ) ) ;
#23154 = CARTESIAN_POINT ( 'NONE',  ( -0.3000000000000000999, -2.289343986263487896, -0.7686455968847020204 ) ) ;
#23155 = AXIS2_PLACEMENT_3D ( 'NONE', #20407, #32940, #4745 ) ;
#23156 = AXIS2_PLACEMENT_3D ( 'NONE', #17484, #2466, #33104 ) ;
#23157 = CARTESIAN_POINT ( 'NONE',  ( -0.05187277790672314981, -0.4529838172322686041, -0.1283400749691716025 ) ) ;
#23158 = CONICAL_SURFACE ( 'NONE', #21840, 0.01999999999999924061, 1.047197551196600962 ) ;
#23159 = EDGE_CURVE ( 'NONE', #1199, #28968, #16507, .T. ) ;
#23160 = DIRECTION ( 'NONE',  ( -1.000000000000000000, -6.779273404243070203E-32, -4.314083075427407763E-32 ) ) ;
#23161 = DIRECTION ( 'NONE',  ( 0.4999551463232372317, -0.8660512985181135770, 0.000000000000000000 ) ) ;
#23162 = CARTESIAN_POINT ( 'NONE',  ( 0.1906247196645203257, -0.5843772811062373229, 0.1513679272151527977 ) ) ;
#23163 = CARTESIAN_POINT ( 'NONE',  ( 0.4133723901694114633, -1.141160002464131962, 0.4339463194546827607 ) ) ;
#23164 = CARTESIAN_POINT ( 'NONE',  ( 0.007518266030304054416, -0.8543892252648230823, 0.3273543424587478379 ) ) ;
#23165 = DIRECTION ( 'NONE',  ( 1.498801083243964091E-15, 2.706744618697167655E-15, 1.000000000000000000 ) ) ;
#23166 = CARTESIAN_POINT ( 'NONE',  ( 0.5534668029622461516, -1.624932764085767367, -0.5687721870468918084 ) ) ;
#23167 = ORIENTED_EDGE ( 'NONE', *, *, #25584, .T. ) ;
#23168 = CARTESIAN_POINT ( 'NONE',  ( 0.2579846408969476701, -0.9486487916598037584, 0.7016806324682074436 ) ) ;
#23169 = CARTESIAN_POINT ( 'NONE',  ( 0.04154009738085443632, -0.2622554993748571484, 0.3904256972020325733 ) ) ;
#23170 = CARTESIAN_POINT ( 'NONE',  ( -0.05137569054208727948, -0.2590973494995065796, -0.3946951280584622967 ) ) ;
#23171 = B_SPLINE_CURVE_WITH_KNOTS ( 'NONE', 3,
 ( #686, #22884, #31917, #28828, #35212, #1091 ),
 .UNSPECIFIED., .F., .F.,
 ( 4, 2, 4 ),
 ( 0.000000000000000000, 0.0003405513792915484993, 0.0006811027585830969986 ),
 .UNSPECIFIED. ) ;
#23172 = ORIENTED_EDGE ( 'NONE', *, *, #31529, .F. ) ;
#23173 = CARTESIAN_POINT ( 'NONE',  ( -0.02000000000000000042, -2.183180860297908144, -0.3917586832283071474 ) ) ;
#23174 = CARTESIAN_POINT ( 'NONE',  ( -0.05634304521267782806, -2.731847993664263218E-15, -0.4588823192046729837 ) ) ;
#23175 = VECTOR ( 'NONE', #161, 39.37007874015748143 ) ;
#23176 = DIRECTION ( 'NONE',  ( 1.000000000000000000, 2.280301054154495132E-31, -1.664003471950577689E-31 ) ) ;
#23177 = CARTESIAN_POINT ( 'NONE',  ( 0.2059273467974227778, -1.283046334493782359, -0.7137159211901564770 ) ) ;
#23178 = CARTESIAN_POINT ( 'NONE',  ( 0.1669756386256049108, -1.085067953939178764, 0.7439077123735935437 ) ) ;
#23179 = ORIENTED_EDGE ( 'NONE', *, *, #15343, .T. ) ;
#23180 = CARTESIAN_POINT ( 'NONE',  ( -0.04154009738085488734, -0.2622554993748581476, -0.3904256972020316296 ) ) ;
#23181 = AXIS2_PLACEMENT_3D ( 'NONE', #4268, #20323, #4862 ) ;
#23182 = AXIS2_PLACEMENT_3D ( 'NONE', #6024, #2967, #328 ) ;
#23183 = CARTESIAN_POINT ( 'NONE',  ( 0.03474878377840755206, 0.07233677907409778729, 0.5114521822558344422 ) ) ;
#23184 = CARTESIAN_POINT ( 'NONE',  ( 0.04308558661660893963, -0.4845714764516787509, -0.09763621268895587846 ) ) ;
#23185 = DIRECTION ( 'NONE',  ( 1.000000000000000000, 0.000000000000000000, 0.000000000000000000 ) ) ;
#23186 = AXIS2_PLACEMENT_3D ( 'NONE', #9857, #18937, #6977 ) ;
#23187 = CARTESIAN_POINT ( 'NONE',  ( 0.4039508790787581516, -1.152909626704288204, 0.7080790044088270951 ) ) ;
#23188 = EDGE_CURVE ( 'NONE', #10339, #1246, #38888, .T. ) ;
#23190 = CARTESIAN_POINT ( 'NONE',  ( -0.02000000000000000042, -2.070343076906777213, -0.2454056712452573896 ) ) ;
#23189 = DIRECTION ( 'NONE',  ( -1.000000000000000000, -2.341930812374887555E-31, 1.664003471950578127E-31 ) ) ;
#23191 = CARTESIAN_POINT ( 'NONE',  ( 0.2870562969094627714, -0.9697506529368410400, 0.5438065585693926396 ) ) ;
#23192 = ORIENTED_EDGE ( 'NONE', *, *, #38880, .T. ) ;
#23193 = FACE_OUTER_BOUND ( 'NONE', #38737, .T. ) ;
#23194 = EDGE_LOOP ( 'NONE', ( #14446, #27586, #35132, #30059 ) ) ;
#23195 = CARTESIAN_POINT ( 'NONE',  ( 0.3268282208471015582, -1.379742495938673930, 0.8813508202197246622 ) ) ;
#23196 = CIRCLE ( 'NONE', #38289, 0.01750000000000001554 ) ;
#23198 = CARTESIAN_POINT ( 'NONE',  ( 0.2005880444173030741, -0.7283351547258000158, 0.3314209756853015443 ) ) ;
#23197 = CARTESIAN_POINT ( 'NONE',  ( 0.08863201702724371467, -0.6115582155368344264, 0.04856835249286290540 ) ) ;
#23199 = CARTESIAN_POINT ( 'NONE',  ( 0.1217997580153728360, -1.296604091693217553, 0.4993402295728919804 ) ) ;
#23200 = ORIENTED_EDGE ( 'NONE', *, *, #32605, .F. ) ;
#23201 = ORIENTED_EDGE ( 'NONE', *, *, #32880, .T. ) ;
#23202 = CARTESIAN_POINT ( 'NONE',  ( -0.02000000000000000042, -2.180619779672576364, -0.3917908354455199582 ) ) ;
#23203 = CARTESIAN_POINT ( 'NONE',  ( 0.5159274993618521155, -1.411867277967620238, 0.7865152916356047408 ) ) ;
#23204 = VERTEX_POINT ( 'NONE', #32121 ) ;
#23205 = CARTESIAN_POINT ( 'NONE',  ( 0.5089189524854907942, -1.641769820029543192, -0.4121086472089234842 ) ) ;
#23206 = CARTESIAN_POINT ( 'NONE',  ( 0.02953079040094766169, -0.5250338024619503052, 0.07436286310882213313 ) ) ;
#23207 = B_SPLINE_CURVE_WITH_KNOTS ( 'NONE', 3,
 ( #4053, #22824, #7329, #35144 ),
 .UNSPECIFIED., .F., .F.,
 ( 4, 4 ),
 ( 1.748223473168675632E-18, 0.001015713385322552413 ),
 .UNSPECIFIED. ) ;
#23208 = CARTESIAN_POINT ( 'NONE',  ( 0.6328777722953394802, -1.566953138837623882, 0.4182417262808777458 ) ) ;
#23209 = CARTESIAN_POINT ( 'NONE',  ( 0.1422768683044231819, -1.284954004962210128, 0.4310363220745050405 ) ) ;
#23210 = CONICAL_SURFACE ( 'NONE', #4150, 0.1346589359789736318, 1.047197551196598742 ) ;
#23211 = CARTESIAN_POINT ( 'NONE',  ( 0.008270684066414063854, -0.5292528935463532980, 0.1457206007561614447 ) ) ;
#23212 = CARTESIAN_POINT ( 'NONE',  ( 0.03309059653085733022, -0.08822156176787505910, 0.5132714489379874845 ) ) ;
#23213 = DIRECTION ( 'NONE',  ( 0.000000000000000000, -0.2513338844154411333, 0.9679004486746792812 ) ) ;
#23214 = CIRCLE ( 'NONE', #39629, 0.5156329413417597429 ) ;
#23215 = CIRCLE ( 'NONE', #14641, 0.1033070866141734129 ) ;
#23216 = CARTESIAN_POINT ( 'NONE',  ( -0.08408070219615712548, -0.09959325338431362917, 0.1000000000000008799 ) ) ;
#23217 = CARTESIAN_POINT ( 'NONE',  ( -0.02000000000000000042, -2.240869484095992181, -0.4096358986825019977 ) ) ;
#23218 = APPROVAL_ROLE ( '' ) ;
#23219 = AXIS2_PLACEMENT_3D ( 'NONE', #18067, #34850, #39659 ) ;
#23220 = FACE_BOUND ( 'NONE', #15381, .T. ) ;
#23221 = CARTESIAN_POINT ( 'NONE',  ( 0.04285640132273772773, 0.3459922227646676229, 0.3537374076363822839 ) ) ;
#23222 = CARTESIAN_POINT ( 'NONE',  ( 0.1847224921572867273, -0.8249592463731384440, 0.04913026459056606815 ) ) ;
#23223 = CYLINDRICAL_SURFACE ( 'NONE', #19875, 0.1946589359789742957 ) ;
#23224 = CARTESIAN_POINT ( 'NONE',  ( 0.1180873783825124868, -1.300942055715428758, 0.4272205016256891419 ) ) ;
#23225 =( GEOMETRIC_REPRESENTATION_CONTEXT ( 3 ) GLOBAL_UNCERTAINTY_ASSIGNED_CONTEXT ( ( #35466 ) ) GLOBAL_UNIT_ASSIGNED_CONTEXT ( ( #11616, #18377, #30925 ) ) REPRESENTATION_CONTEXT ( 'NONE', 'WORKASPACE' ) );
#23226 = CARTESIAN_POINT ( 'NONE',  ( 0.2142493868227219878, -1.379310565402303457, 1.003739045973664368 ) ) ;
#23227 = CARTESIAN_POINT ( 'NONE',  ( 0.5956979983064725204, -1.550072859360259070, -0.5756593981205863075 ) ) ;
#23228 = CARTESIAN_POINT ( 'NONE',  ( 0.000000000000000000, -0.02999999999999995379, 0.000000000000000000 ) ) ;
#23229 = DIRECTION ( 'NONE',  ( -0.9848077530122080203, -0.1736481776669303589, 2.792475675812634297E-17 ) ) ;
#23230 = CARTESIAN_POINT ( 'NONE',  ( -0.04945776359515208220, -0.3082555652855825112, 0.3644343153303030713 ) ) ;
#23231 = ORIENTED_EDGE ( 'NONE', *, *, #17805, .T. ) ;
#23232 = ORIENTED_EDGE ( 'NONE', *, *, #17430, .T. ) ;
#23233 = CARTESIAN_POINT ( 'NONE',  ( 0.05583995664670776682, -1.335624775257321817, 0.3157417262808777658 ) ) ;
#23234 = ORIENTED_EDGE ( 'NONE', *, *, #22732, .T. ) ;
#23235 = FACE_OUTER_BOUND ( 'NONE', #28541, .T. ) ;
#23236 = CARTESIAN_POINT ( 'NONE',  ( 0.2059273467974225835, -1.283046334493782137, -0.6485234391946320676 ) ) ;
#23237 = VECTOR ( 'NONE', #38732, 39.37007874015748854 ) ;
#23238 = CARTESIAN_POINT ( 'NONE',  ( 0.3636646492274219766, -1.094494851808226699, 0.7706032642260752796 ) ) ;
#23240 = VERTEX_POINT ( 'NONE', #29029 ) ;
#23239 = DIRECTION ( 'NONE',  ( -6.106226635438322318E-15, 2.142487232963740814E-14, 1.000000000000000000 ) ) ;
#23241 = CARTESIAN_POINT ( 'NONE',  ( 0.3816662009041032477, -0.9823246188028521564, 0.6672886469660396225 ) ) ;
#23242 = DIRECTION ( 'NONE',  ( 7.771561172376107616E-16, -7.170354002788761615E-17, 1.000000000000000000 ) ) ;
#23243 = ORIENTED_EDGE ( 'NONE', *, *, #12837, .T. ) ;
#23244 = CARTESIAN_POINT ( 'NONE',  ( 0.5910253966860438135, -1.487811233934940081, -0.6023409643032461291 ) ) ;
#23245 = EDGE_CURVE ( 'NONE', #31435, #22141, #29663, .T. ) ;
#23246 = AXIS2_PLACEMENT_3D ( 'NONE', #36568, #3030, #8371 ) ;
#23247 = AXIS2_PLACEMENT_3D ( 'NONE', #39643, #3035, #25452 ) ;
#23248 = CARTESIAN_POINT ( 'NONE',  ( 0.3305191838506285618, -1.637725477021584553, 0.6377116139030889475 ) ) ;
#23250 = CARTESIAN_POINT ( 'NONE',  ( -0.02231181081520691722, -0.5045902076536115111, 0.09028112709016047899 ) ) ;
#23249 = CARTESIAN_POINT ( 'NONE',  ( 0.2625973931889362678, -0.6796768235205253861, 0.1477649966949237115 ) ) ;
#23251 = DIRECTION ( 'NONE',  ( 0.4849077135392313997, -0.8745653259477845776, 0.000000000000000000 ) ) ;
#23252 = EDGE_CURVE ( 'NONE', #29445, #4305, #39484, .T. ) ;
#23253 = CARTESIAN_POINT ( 'NONE',  ( 0.1183779203685188658, -1.376060927314119553, -0.3271212237852036409 ) ) ;
#23254 = ORIENTED_EDGE ( 'NONE', *, *, #5688, .F. ) ;
#23255 = EDGE_CURVE ( 'NONE', #29395, #12860, #7203, .T. ) ;
#23256 = LINE ( 'NONE', #36177, #319 ) ;
#23257 = CARTESIAN_POINT ( 'NONE',  ( -0.1157923916715208196, -0.5295015842444287246, 0.3181161673586317962 ) ) ;
#23258 = CARTESIAN_POINT ( 'NONE',  ( 0.02869942827333513830, 0.4892109928530955498, 0.09550568247005990219 ) ) ;
#23259 = AXIS2_PLACEMENT_3D ( 'NONE', #32948, #23109, #33162 ) ;
#23260 = CARTESIAN_POINT ( 'NONE',  ( 0.1814429951780466566, -0.9296868405956840720, 0.6374604447006659846 ) ) ;
#23261 = CARTESIAN_POINT ( 'NONE',  ( 0.01155947731736221493, -0.5664951642967490653, 0.2915036740642469870 ) ) ;
#23262 = CARTESIAN_POINT ( 'NONE',  ( 0.4673063575290828386, -1.111595057335264647, 0.5567563882193511393 ) ) ;
#23263 = CARTESIAN_POINT ( 'NONE',  ( -0.1574156176409247099, 0.4885425907994572214, 0.3417174393643599428 ) ) ;
#23264 = CARTESIAN_POINT ( 'NONE',  ( 0.6632248500530988355, -1.473733142766466386, 0.4224342954051147347 ) ) ;
#23265 = CARTESIAN_POINT ( 'NONE',  ( 0.05634307799789359250, 0.4395998308137160637, 0.1320249839695993577 ) ) ;
#23266 = EDGE_CURVE ( 'NONE', #31025, #30141, #27022, .T. ) ;
#23267 = DIRECTION ( 'NONE',  ( 1.000000000000000000, -0.000000000000000000, -0.000000000000000000 ) ) ;
#23268 = CARTESIAN_POINT ( 'NONE',  ( 0.05999999999999990757, -0.1022126893003200560, -0.2231384537392532841 ) ) ;
#23269 = APPROVAL ( #16521, 'UNSPECIFIED' ) ;
#23270 = CIRCLE ( 'NONE', #28503, 0.005000000000000014849 ) ;
#23271 = CARTESIAN_POINT ( 'NONE',  ( 0.01088233830205680326, -1.005040962621902345, 0.5452311825355896646 ) ) ;
#23272 = CARTESIAN_POINT ( 'NONE',  ( 0.1637488714925408873, -0.5994898440788770655, 0.1932149833450298726 ) ) ;
#23273 = PRODUCT_DEFINITION_CONTEXT ( 'detailed design', #10342, 'design' ) ;
#23274 = FACE_OUTER_BOUND ( 'NONE', #13343, .T. ) ;
#23275 = AXIS2_PLACEMENT_3D ( 'NONE', #23123, #17130, #26015 ) ;
#23276 = AXIS2_PLACEMENT_3D ( 'NONE', #12092, #9397, #40050 ) ;
#23277 = ORIENTED_EDGE ( 'NONE', *, *, #36700, .T. ) ;
#23278 = PRODUCT_DEFINITION_SHAPE ( 'NONE', 'NONE',  #40655 ) ;
#23279 = DIRECTION ( 'NONE',  ( -7.771561172376107616E-16, 7.170354002788761615E-17, -1.000000000000000000 ) ) ;
#23280 = CARTESIAN_POINT ( 'NONE',  ( 0.4529143664019396609, -1.108999136783218153, 0.5738870192722926866 ) ) ;
#23281 = LINE ( 'NONE', #7194, #34992 ) ;
#23282 = DIRECTION ( 'NONE',  ( 0.4999551463232372317, -0.8660512985181135770, 0.000000000000000000 ) ) ;
#23283 = CIRCLE ( 'NONE', #4857, 0.1600000000000006140 ) ;
#23284 = ORIENTED_EDGE ( 'NONE', *, *, #40365, .F. ) ;
#23285 = AXIS2_PLACEMENT_3D ( 'NONE', #25069, #22402, #22004 ) ;
#23286 = CARTESIAN_POINT ( 'NONE',  ( 0.1776121323683093056, -0.4901272394318858527, 0.1210201606631986920 ) ) ;
#23287 = VERTEX_POINT ( 'NONE', #10328 ) ;
#23288 = CARTESIAN_POINT ( 'NONE',  ( 0.2580628395236652106, -1.678234314258598925, 0.5461929056667225169 ) ) ;
#23289 = CARTESIAN_POINT ( 'NONE',  ( 0.3750645785205684035, -1.122292824651612397, 0.8025833334800251961 ) ) ;
#23291 = ORIENTED_EDGE ( 'NONE', *, *, #4868, .F. ) ;
#23290 = CARTESIAN_POINT ( 'NONE',  ( 0.006933825066843425124, -0.8076031261048381982, 0.04254292565515345459 ) ) ;
#23293 = ORIENTED_EDGE ( 'NONE', *, *, #26543, .F. ) ;
#23292 = ORIENTED_EDGE ( 'NONE', *, *, #4175, .F. ) ;
#23294 = CARTESIAN_POINT ( 'NONE',  ( 0.5547152119369697099, -1.589750697506561616, -0.5166151207188711680 ) ) ;
#23295 = ADVANCED_FACE ( 'NONE', ( #22891 ), #1464, .T. ) ;
#23296 = CARTESIAN_POINT ( 'NONE',  ( -0.006114502025653725630, -0.6147594159447776763, 0.4101266738532061695 ) ) ;
#23298 = DIRECTION ( 'NONE',  ( -1.000000000000000000, 0.000000000000000000, 0.000000000000000000 ) ) ;
#23297 = LINE ( 'NONE', #6653, #33831 ) ;
#23299 = DIRECTION ( 'NONE',  ( 1.188678714063518227E-15, -1.000000000000000000, -3.263080277421930985E-16 ) ) ;
#23300 = CALENDAR_DATE ( 2026, 13, 10 ) ;
#23301 = CIRCLE ( 'NONE', #37753, 0.06250000000000001388 ) ;
#23302 = ADVANCED_FACE ( 'NONE', ( #34999 ), #39035, .F. ) ;
#23303 = CARTESIAN_POINT ( 'NONE',  ( 0.001051957896761219601, -0.5275076572294767896, -0.06462206035643838775 ) ) ;
#23305 = ORIENTED_EDGE ( 'NONE', *, *, #37637, .F. ) ;
#23304 = ORIENTED_EDGE ( 'NONE', *, *, #34631, .F. ) ;
#23306 = EDGE_CURVE ( 'NONE', #12532, #24285, #12897, .T. ) ;
#23307 = CARTESIAN_POINT ( 'NONE',  ( 0.1399519254280139069, -0.8623850441597388228, 0.4929895343781093842 ) ) ;
#23308 = CIRCLE ( 'NONE', #12773, 0.01499999999999995087 ) ;
#23309 = CARTESIAN_POINT ( 'NONE',  ( 0.1213787196452971867, -0.7177200554198521765, 0.5360780237648733459 ) ) ;
#23310 = AXIS2_PLACEMENT_3D ( 'NONE', #196, #16205, #10225 ) ;
#23311 = CARTESIAN_POINT ( 'NONE',  ( 0.1100557636787395099, -0.5505741347682650000, 0.1801202379966963252 ) ) ;
#23312 = CARTESIAN_POINT ( 'NONE',  ( 0.2923286432308245808, -1.660243258845594649, -0.3370932271639339728 ) ) ;
#23313 = CARTESIAN_POINT ( 'NONE',  ( 0.05999999999999990757, 0.01983442501260774746, 0.03516089415102874316 ) ) ;
#23314 = AXIS2_PLACEMENT_3D ( 'NONE', #34630, #2314, #25957 ) ;
#23315 = CARTESIAN_POINT ( 'NONE',  ( 0.6615779634392502384, -1.540590691117124322, 0.4334491422028962648 ) ) ;
#23316 = CARTESIAN_POINT ( 'NONE',  ( 0.3293809238194490563, -1.753471329581329119, 0.5621866716956569476 ) ) ;
#23317 = CARTESIAN_POINT ( 'NONE',  ( 0.6937322149078435363, -1.428803319834411001, 0.5909098324580162043 ) ) ;
#23318 = CIRCLE ( 'NONE', #36412, 0.03000000000000000583 ) ;
#23319 = CARTESIAN_POINT ( 'NONE',  ( 0.4906998715583268944, -1.589006395870980359, -0.5745131788651638427 ) ) ;
#23320 = DIRECTION ( 'NONE',  ( -1.725633230170958726E-31, -0.8983234858819668656, 0.4393346272636288186 ) ) ;
#23321 = CARTESIAN_POINT ( 'NONE',  ( 0.01548846960707528191, 0.2306506793134049660, -0.4716198300880325434 ) ) ;
#23322 = CIRCLE ( 'NONE', #20016, 0.5399999999999999245 ) ;
#23323 = CARTESIAN_POINT ( 'NONE',  ( 0.01180359879124304526, -0.6193534279860481995, -0.1047011498718341121 ) ) ;
#23324 = EDGE_CURVE ( 'NONE', #21906, #13009, #16531, .T. ) ;
#23325 = CARTESIAN_POINT ( 'NONE',  ( 0.09245883518616107577, -0.6465694857495450920, 0.4344858352814658375 ) ) ;
#23326 = DIRECTION ( 'NONE',  ( 0.000000000000000000, 1.821231995776163252E-15, -1.000000000000000000 ) ) ;
#23327 = LINE ( 'NONE', #36239, #35029 ) ;
#23328 = CARTESIAN_POINT ( 'NONE',  ( -0.0004320282599767403219, -0.9107381779821550616, 0.3274798035714688860 ) ) ;
#23329 = CARTESIAN_POINT ( 'NONE',  ( 0.4924424051965485827, -1.082438949443123688, 0.5780025781777323735 ) ) ;
#23330 = DATE_AND_TIME ( #10974, #35194 ) ;
#23331 = CARTESIAN_POINT ( 'NONE',  ( 0.3390826044135689665, -0.8321809361840178942, 0.7462327844847882474 ) ) ;
#23332 = AXIS2_PLACEMENT_3D ( 'NONE', #24010, #11043, #17800 ) ;
#23333 = AXIS2_PLACEMENT_3D ( 'NONE', #34418, #25577, #12605 ) ;
#23334 = CARTESIAN_POINT ( 'NONE',  ( 0.3699999999999786793, -2.097675824466503691, -0.5196396315034578217 ) ) ;
#23335 = CARTESIAN_POINT ( 'NONE',  ( 0.3084895503185087207, -1.760900578822133467, 0.5693513805774124137 ) ) ;
#23336 = B_SPLINE_CURVE_WITH_KNOTS ( 'NONE', 3,
 ( #10386, #16360, #20265, #7885, #20455, #28896, #32787, #14075, #7699, #32593, #13856, #29102, #19649, #3804 ),
 .UNSPECIFIED., .F., .F.,
 ( 4, 2, 2, 2, 2, 2, 4 ),
 ( 0.008198847749948421498, 0.008708900428346920755, 0.009218953106745421747, 0.009729005785143921003, 0.01023905846354242200, 0.01125916382033939796, 0.01227926917713637392 ),
 .UNSPECIFIED. ) ;
#23337 = CIRCLE ( 'NONE', #2301, 0.04749999999977556897 ) ;
#23338 = ORIENTED_EDGE ( 'NONE', *, *, #4579, .T. ) ;
#23339 = CARTESIAN_POINT ( 'NONE',  ( -0.01548846960707504251, -0.3772621329472741758, 0.3651003739303441131 ) ) ;
#23340 = LOCAL_TIME ( 0, 53, 7.000000000000000000, #6136 ) ;
#23341 = DIRECTION ( 'NONE',  ( 0.000000000000000000, 0.000000000000000000, 1.000000000000000000 ) ) ;
#23342 = CARTESIAN_POINT ( 'NONE',  ( 0.2059273467974228333, -1.283046334493783247, -0.6445565283433527526 ) ) ;
#23343 = ORIENTED_EDGE ( 'NONE', *, *, #33369, .F. ) ;
#23344 = CARTESIAN_POINT ( 'NONE',  ( 0.06486042810549992599, -1.341249661891149803, 0.5682417262808776570 ) ) ;
#23345 = AXIS2_PLACEMENT_3D ( 'NONE', #17021, #36133, #4647 ) ;
#23346 = CARTESIAN_POINT ( 'NONE',  ( 0.5385451171429854744, -1.174625208511617114, 0.8096455807874475274 ) ) ;
#23348 = VERTEX_POINT ( 'NONE', #3820 ) ;
#23347 = ORIENTED_EDGE ( 'NONE', *, *, #4454, .T. ) ;
#23349 = CARTESIAN_POINT ( 'NONE',  ( 0.02650569172316860275, -1.591189904831632029, -0.6662411422194330912 ) ) ;
#23350 = EDGE_CURVE ( 'NONE', #478, #40377, #4709, .T. ) ;
#23351 = ORIENTED_EDGE ( 'NONE', *, *, #31320, .T. ) ;
#23352 = ORIENTED_EDGE ( 'NONE', *, *, #10704, .T. ) ;
#23353 = CARTESIAN_POINT ( 'NONE',  ( 0.3573784231975513093, -1.820466169614756158, -0.5023318515619766833 ) ) ;
#23354 = LINE ( 'NONE', #14662, #28533 ) ;
#23355 = EDGE_CURVE ( 'NONE', #16485, #7866, #20469, .T. ) ;
#23356 = CARTESIAN_POINT ( 'NONE',  ( -0.04211812644076891321, 0.4433543613217477697, -0.1530385388104362199 ) ) ;
#23357 = ORIENTED_EDGE ( 'NONE', *, *, #10546, .F. ) ;
#23358 = CARTESIAN_POINT ( 'NONE',  ( 0.05153374671598465878, -0.6956169804826777270, 0.7932021015506084405 ) ) ;
#23359 = CARTESIAN_POINT ( 'NONE',  ( 0.1445017185149053141, -0.7748226788906442675, 0.5206329989080951126 ) ) ;
#23360 = CARTESIAN_POINT ( 'NONE',  ( 0.1921532005765090867, -1.222151250233040942, 1.020715813206927614 ) ) ;
#23361 = CARTESIAN_POINT ( 'NONE',  ( 0.4713144649729504865, -1.557651269372687608, 0.6044819294908458929 ) ) ;
#23363 = CARTESIAN_POINT ( 'NONE',  ( 0.2687203115727492264, -1.674044157977605529, 0.5754666865148680976 ) ) ;
#23362 = CARTESIAN_POINT ( 'NONE',  ( 0.2398555970347700794, -1.530130166554039439, 0.9080419457258624982 ) ) ;
#23364 = CARTESIAN_POINT ( 'NONE',  ( 0.2565301720564582832, -1.029081863103397554, 0.6124915876908022527 ) ) ;
#23365 = ORIENTED_EDGE ( 'NONE', *, *, #6675, .T. ) ;
#23366 = ADVANCED_FACE ( 'NONE', ( #34888 ), #13237, .T. ) ;
#23367 = ORIENTED_EDGE ( 'NONE', *, *, #17306, .T. ) ;
#23368 = AXIS2_PLACEMENT_3D ( 'NONE', #7426, #3760, #524 ) ;
#23369 = DIRECTION ( 'NONE',  ( 0.000000000000000000, 0.000000000000000000, -1.000000000000000000 ) ) ;
#23370 = CARTESIAN_POINT ( 'NONE',  ( 0.1907289319405431338, -0.5457051035001712069, 0.2140866037401576716 ) ) ;
#23371 = AXIS2_PLACEMENT_3D ( 'NONE', #11754, #27596, #36836 ) ;
#23372 = CARTESIAN_POINT ( 'NONE',  ( -0.04308745346420421451, 0.2425953941929087643, -0.4306799763758774602 ) ) ;
#23373 = APPROVAL_PERSON_ORGANIZATION ( #7237, #33040, #28865 ) ;
#23374 = LINE ( 'NONE', #32791, #6133 ) ;
#23375 = ADVANCED_FACE ( 'NONE', ( #14890 ), #12473, .T. ) ;
#23376 = APPLIED_DATE_AND_TIME_ASSIGNMENT ( #10519, #38901, ( #3089 ) ) ;
#23377 = CARTESIAN_POINT ( 'NONE',  ( 0.1909286924077255587, -1.257064795538239022, -0.6919843404141109433 ) ) ;
#23378 = EDGE_CURVE ( 'NONE', #23675, #29082, #31604, .T. ) ;
#23379 = B_SPLINE_CURVE_WITH_KNOTS ( 'NONE', 3,
 ( #2040, #7594, #29608, #20169, #26745, #10900, #7988, #1854, #14180, #14369, #38854, #11097, #8202, #39274, #23258, #7793, #23472, #23657 ),
 .UNSPECIFIED., .F., .F.,
 ( 4, 2, 2, 2, 2, 2, 2, 2, 4 ),
 ( -0.002633528389679591110, -0.001975271857855645692, -0.001317015326031700274, -0.0006587587942077548567, -5.022623838094389392E-07, 0.0006577542694401359788, 0.001316010801264081397, 0.001974267333088026814, 0.002632523864911972232 ),
 .UNSPECIFIED. ) ;
#23380 = VECTOR ( 'NONE', #10490, 39.37007874015748854 ) ;
#23381 = CARTESIAN_POINT ( 'NONE',  ( 0.1175190731393374044, -1.414871271504619221, 0.5257910806408424564 ) ) ;
#23382 = CARTESIAN_POINT ( 'NONE',  ( 0.5536319580448211264, -1.193555294463456873, 0.7337749688435845075 ) ) ;
#23383 = DIRECTION ( 'NONE',  ( 1.188678714063518227E-15, -1.000000000000000000, -3.263080277421930985E-16 ) ) ;
#23384 = CARTESIAN_POINT ( 'NONE',  ( 0.02317288298003269270, -0.9573509765991652376, 0.6276687800861534550 ) ) ;
#23385 = DIRECTION ( 'NONE',  ( 1.000000000000000000, 0.000000000000000000, 0.000000000000000000 ) ) ;
#23386 = CARTESIAN_POINT ( 'NONE',  ( 0.3245308759113119113, -1.295391163961464365, 0.5682442948123348492 ) ) ;
#23387 = ORIENTED_EDGE ( 'NONE', *, *, #33344, .F. ) ;
#23388 = CARTESIAN_POINT ( 'NONE',  ( 0.3351423068873352062, -1.099926675622169725, 0.7404414555003379084 ) ) ;
#23389 = CARTESIAN_POINT ( 'NONE',  ( 0.03662792686184425384, 0.04111994379180462789, 0.4792679903722379953 ) ) ;
#23390 = CARTESIAN_POINT ( 'NONE',  ( -0.05268850283020126007, -0.2717122958104509767, -0.3818262463465889600 ) ) ;
#23391 = VERTEX_POINT ( 'NONE', #37562 ) ;
#23392 = CARTESIAN_POINT ( 'NONE',  ( -0.2399999999999999079, -2.427691829037316396, -0.9241619397096791921 ) ) ;
#23393 = CARTESIAN_POINT ( 'NONE',  ( 0.01548846960707511190, -0.5198120922912051745, -0.07362328916749329155 ) ) ;
#23394 = CARTESIAN_POINT ( 'NONE',  ( 0.3601132046754574323, -1.751178885491700532, -0.4776197548361051370 ) ) ;
#23395 = CARTESIAN_POINT ( 'NONE',  ( -0.02000000000000000042, -1.622350287959229087, -0.08960079202753243321 ) ) ;
#23396 = CIRCLE ( 'NONE', #17469, 0.01499999999999995955 ) ;
#23397 = AXIS2_PLACEMENT_3D ( 'NONE', #33543, #21224, #33761 ) ;
#23398 = DIMENSIONAL_EXPONENTS ( 1.000000000000000000, 0.000000000000000000, 0.000000000000000000, 0.000000000000000000, 0.000000000000000000, 0.000000000000000000, 0.000000000000000000 ) ;
#23399 = CARTESIAN_POINT ( 'NONE',  ( 0.06321419030197487909, -0.8491159278358076934, 0.3547255550195697049 ) ) ;
#23400 = ORIENTED_EDGE ( 'NONE', *, *, #10337, .T. ) ;
#23401 = CARTESIAN_POINT ( 'NONE',  ( -0.1688425317846180274, 0.4915896084592928372, 0.3245441658521737716 ) ) ;
#23402 = CARTESIAN_POINT ( 'NONE',  ( 0.03643058821097343303, 0.08373535757664200829, 0.5050280785339766876 ) ) ;
#23403 = LOCAL_TIME ( 0, 53, 7.000000000000000000, #682 ) ;
#23404 = CARTESIAN_POINT ( 'NONE',  ( -0.08408070219616067820, -0.09959325338431368468, 0.08499999999999965916 ) ) ;
#23405 = CARTESIAN_POINT ( 'NONE',  ( 0.05999999999999990757, 0.1997995745459845707, -0.008951536808938237097 ) ) ;
#23406 = CARTESIAN_POINT ( 'NONE',  ( 0.4799179709319398857, -1.259100254504656569, 0.5857027040861966238 ) ) ;
#23407 = EDGE_CURVE ( 'NONE', #394, #10240, #9299, .T. ) ;
#23409 = DIRECTION ( 'NONE',  ( -1.654489825136719548E-31, 0.9510565162951568619, 0.3090169943749375703 ) ) ;
#23408 = LINE ( 'NONE', #36111, #18674 ) ;
#23410 = CARTESIAN_POINT ( 'NONE',  ( 0.1885390680155161480, -0.9156976364345736918, 0.1977769869421455440 ) ) ;
#23411 = ORIENTED_EDGE ( 'NONE', *, *, #36333, .F. ) ;
#23412 = EDGE_CURVE ( 'NONE', #3229, #13737, #31658, .T. ) ;
#23413 = CIRCLE ( 'NONE', #32563, 0.04500000000000044242 ) ;
#23414 = CARTESIAN_POINT ( 'NONE',  ( 0.2209260011871197193, -1.309027873449325918, -0.4125659523519145666 ) ) ;
#23415 = ORIENTED_EDGE ( 'NONE', *, *, #13551, .T. ) ;
#23416 = CARTESIAN_POINT ( 'NONE',  ( 0.01188899208819103881, -0.5504388812625971017, -0.07422846483693842923 ) ) ;
#23417 = CARTESIAN_POINT ( 'NONE',  ( 0.4146543403318773691, -1.589641078845216882, 0.5897920107734272444 ) ) ;
#23418 = CARTESIAN_POINT ( 'NONE',  ( 0.06900019283952113502, -0.5439056195324916132, 0.1104857819084973242 ) ) ;
#23419 = CARTESIAN_POINT ( 'NONE',  ( -0.1167294259372883281, -0.5331983348239501819, 0.3032895567580801144 ) ) ;
#23420 = ORIENTED_EDGE ( 'NONE', *, *, #18023, .T. ) ;
#23421 = VERTEX_POINT ( 'NONE', #13088 ) ;
#23422 = DIRECTION ( 'NONE',  ( 1.188678714063518227E-15, -1.000000000000000000, -3.263080277421930985E-16 ) ) ;
#23423 = CARTESIAN_POINT ( 'NONE',  ( 0.5423765350489757608, -1.450385248195758647, 0.7501209832966719837 ) ) ;
#23424 = ORIENTED_EDGE ( 'NONE', *, *, #9032, .F. ) ;
#23425 = CARTESIAN_POINT ( 'NONE',  ( -0.2399999999999999079, -2.845511416290244622, -0.3415338532332813926 ) ) ;
#23426 = CARTESIAN_POINT ( 'NONE',  ( 0.03672447062657525213, -0.4430265621404764209, 0.1868507191434652936 ) ) ;
#23427 = CARTESIAN_POINT ( 'NONE',  ( 0.3959772125322972292, -1.738667461359298283, -0.4364921393681684414 ) ) ;
#23428 = CARTESIAN_POINT ( 'NONE',  ( 0.2246977112670445476, -1.237341369623786269, 0.4719027293363190489 ) ) ;
#23429 = CARTESIAN_POINT ( 'NONE',  ( 0.4002945600007836169, -1.748174799945819924, -0.4981529668752289752 ) ) ;
#23430 = CARTESIAN_POINT ( 'NONE',  ( 0.1399999999999994582, 1.942890293094024131E-17, 0.04999999999999998890 ) ) ;
#23431 = CIRCLE ( 'NONE', #16831, 0.1500000000000009936 ) ;
#23432 = CARTESIAN_POINT ( 'NONE',  ( 0.1952857665188987568, -0.5148003437455072051, 0.3467747870930740217 ) ) ;
#23433 = CARTESIAN_POINT ( 'NONE',  ( 0.000000000000000000, -0.01499999999999997689, 0.000000000000000000 ) ) ;
#23434 = CARTESIAN_POINT ( 'NONE',  ( 0.04154009738085462367, -0.2902754972779521547, -0.3700679770908125166 ) ) ;
#23435 = LOCAL_TIME ( 0, 53, 7.000000000000000000, #30512 ) ;
#23436 = CARTESIAN_POINT ( 'NONE',  ( 0.6119035909732429834, -1.554882900545723423, -0.6235685469894116650 ) ) ;
#23437 = CARTESIAN_POINT ( 'NONE',  ( 0.01899496522501941537, 0.3622296354306406285, 0.3730445619378072730 ) ) ;
#23438 = CARTESIAN_POINT ( 'NONE',  ( 0.1849765250084728363, -0.7825370905210525807, 0.005108896899734703331 ) ) ;
#23439 = DIRECTION ( 'NONE',  ( 0.000000000000000000, 0.7071067811865474617, 0.7071067811865475727 ) ) ;
#23440 = AXIS2_PLACEMENT_3D ( 'NONE', #31959, #16136, #26008 ) ;
#23441 = DIRECTION ( 'NONE',  ( 0.000000000000000000, 0.000000000000000000, -1.000000000000000000 ) ) ;
#23442 = CARTESIAN_POINT ( 'NONE',  ( 0.01602427940967538628, -0.5690816651727684805, 0.5319142476028417832 ) ) ;
#23443 = CARTESIAN_POINT ( 'NONE',  ( 0.5646341918047996788, -1.583084905584069224, -0.5428242601959012426 ) ) ;
#23444 = CARTESIAN_POINT ( 'NONE',  ( -0.3000000000000000999, -1.962518963160043706, -0.3791801492432049225 ) ) ;
#23445 = CARTESIAN_POINT ( 'NONE',  ( 0.5848508152300195828, -1.486263022089187036, 0.6467108361231791447 ) ) ;
#23446 = CARTESIAN_POINT ( 'NONE',  ( -0.02242905165738659501, -0.2417642932583371762, 0.4517135660370446559 ) ) ;
#23447 = ORIENTED_EDGE ( 'NONE', *, *, #2091, .T. ) ;
#23448 = ORIENTED_EDGE ( 'NONE', *, *, #29904, .T. ) ;
#23449 = CARTESIAN_POINT ( 'NONE',  ( 0.1091517887402940062, -1.415340451669741872, 0.5420629516186480368 ) ) ;
#23450 = CYLINDRICAL_SURFACE ( 'NONE', #11849, 0.4615209409081864611 ) ;
#23451 = ORIENTED_EDGE ( 'NONE', *, *, #8220, .F. ) ;
#23452 = SPHERICAL_SURFACE ( 'NONE', #31588, 0.01499999999999999944 ) ;
#23453 = FACE_OUTER_BOUND ( 'NONE', #36248, .T. ) ;
#23454 = CARTESIAN_POINT ( 'NONE',  ( 0.5572041907646198000, -1.389387165738231067, 0.7048252436811164312 ) ) ;
#23456 = EDGE_LOOP ( 'NONE', ( #28270, #28130 ) ) ;
#23455 = DIRECTION ( 'NONE',  ( -1.000000000000000000, -6.779273404243070203E-32, -4.314083075427408311E-32 ) ) ;
#23457 = CARTESIAN_POINT ( 'NONE',  ( 0.3223305689799217388, -0.9241512680936796453, 0.6167986945225242268 ) ) ;
#23458 = VECTOR ( 'NONE', #28514, 39.37007874015748143 ) ;
#23459 = DIRECTION ( 'NONE',  ( 0.4999551463232373427, -0.8660512985181134660, 0.000000000000000000 ) ) ;
#23460 = VERTEX_POINT ( 'NONE', #25646 ) ;
#23461 = FACE_OUTER_BOUND ( 'NONE', #15594, .T. ) ;
#23462 =( BOUNDED_SURFACE ( )  B_SPLINE_SURFACE ( 3, 2, ( 
 ( #8393, #20964, #1651 ),
 ( #30416, #14786, #14363 ),
 ( #23852, #33291, #14566 ),
 ( #10893, #18071, #7787 ),
 ( #27347, #17465, #32877 ),
 ( #36377, #33484, #36774 ),
 ( #4899, #7981, #8196 ),
 ( #17257, #20557, #30018 ),
 ( #20768, #2448, #33091 ),
 ( #20356, #26738, #33692 ),
 ( #30623, #39878, #14986 ),
 ( #26927, #11091, #23651 ),
 ( #30204, #5100, #39067 ),
 ( #2035, #5506, #27133 ),
 ( #39664, #24252, #8587 ),
 ( #12494, #34102, #5905 ),
 ( #12, #27734, #25051 ),
 ( #28147, #2640, #2839 ),
 ( #11886, #18277, #27948 ),
 ( #9201, #21384, #33920 ),
 ( #5719, #40269, #25260 ),
 ( #21580, #37199, #24452 ),
 ( #22195, #31626, #6515 ),
 ( #19087, #37802, #3441 ),
 ( #27539, #18895, #30820 ),
 ( #6110, #9621, #6322 ),
 ( #34710, #40060, #36985 ),
 ( #24671, #12698, #15391 ),
 ( #15176, #9019, #12105 ),
 ( #21984, #18466, #40486 ),
 ( #34512, #31019, #8806 ),
 ( #12312, #24868, #21770 ),
 ( #37388, #34303, #31433 ),
 ( #15785, #18677, #31240 ),
 ( #3056, #37585, #15601 ),
 ( #9407, #3239, #28335 ),
 ( #206, #16394, #19891 ),
 ( #3653, #12915, #26274 ),
 ( #25882, #16214, #35721 ),
 ( #3837, #15999, #28749 ),
 ( #7117, #38790, #22384 ),
 ( #28547, #35124, #31837 ) ),
 .UNSPECIFIED., .F., .F., .T. ) 
 B_SPLINE_SURFACE_WITH_KNOTS ( ( 4, 2, 2, 2, 2, 2, 2, 2, 2, 2, 2, 2, 2, 2, 2, 2, 2, 2, 2, 2, 4 ),
 ( 3, 3 ),
 ( 0.005950481707744588282, 0.006716259263195396498, 0.007482036818646203846, 0.008247814374097012929, 0.009013591929547820278, 0.009396480707273224819, 0.009779369484998627626, 0.01016225826272403217, 0.01054514704044943671, 0.01131092459590024579, 0.01207670215135105314, 0.01284247970680186049, 0.01360825726225266957, 0.01399114603997807238, 0.01437403481770347692, 0.01513981237315428427, 0.01590558992860509335, 0.01628847870633049616, 0.01667136748405589897, 0.01743714503950670805, 0.01820292259495751713 ),
 ( 0.1244524664081657073, 1.000000000000000000 ),
 .UNSPECIFIED. ) 
 GEOMETRIC_REPRESENTATION_ITEM ( )  RATIONAL_B_SPLINE_SURFACE ( (
 ( 0.9499063442391089129, 0.7987438208070558598, 1.000000000000000000),
 ( 0.9499101753461761666, 0.7987592126557592209, 1.000000000000000000),
 ( 0.9498996626311451141, 0.7987169767911981300, 1.000000000000000000),
 ( 0.9498647205990344844, 0.7985765937472975029, 1.000000000000000000),
 ( 0.9498406268971775201, 0.7984797949350583846, 1.000000000000000000),
 ( 0.9497859433926709727, 0.7982600985879926281, 1.000000000000000000),
 ( 0.9497549696405049868, 0.7981356584982937097, 1.000000000000000000),
 ( 0.9496882370548647145, 0.7978675537850399291, 1.000000000000000000),
 ( 0.9496520408222892673, 0.7977221318676597228, 1.000000000000000000),
 ( 0.9495915405754780103, 0.7974790661874149311, 1.000000000000000000),
 ( 0.9495703971913793673, 0.7973941205663723775, 1.000000000000000000),
 ( 0.9495268132974180597, 0.7972190179942053589, 1.000000000000000000),
 ( 0.9495042694130420013, 0.7971284457258256406, 1.000000000000000000),
 ( 0.9494576496633018170, 0.7969411463050679600, 1.000000000000000000),
 ( 0.9494335756765570622, 0.7968444267002283699, 1.000000000000000000),
 ( 0.9493838834922390113, 0.7966447834719645460, 1.000000000000000000),
 ( 0.9493581158244890350, 0.7965412593374354699, 1.000000000000000000),
 ( 0.9492798676385878487, 0.7962268895697659499, 1.000000000000000000),
 ( 0.9492263787684320775, 0.7960119927834690134, 1.000000000000000000),
 ( 0.9491168155290150565, 0.7955718117144263690, 1.000000000000000000),
 ( 0.9490603055549355904, 0.7953447773465653903, 1.000000000000000000),
 ( 0.9489483632414097425, 0.7948950381137618315, 1.000000000000000000),
 ( 0.9488921165716348582, 0.7946690615967901827, 1.000000000000000000),
 ( 0.9487835679013090218, 0.7942329566586614487, 1.000000000000000000),
 ( 0.9487309736807549854, 0.7940216542149569623, 1.000000000000000000),
 ( 0.9486547899165758135, 0.7937155784641993783, 1.000000000000000000),
 ( 0.9486297387484154964, 0.7936149329371018357, 1.000000000000000000),
 ( 0.9485816243033379225, 0.7934216284311081946, 1.000000000000000000),
 ( 0.9485584661661164985, 0.7933285883416276718, 1.000000000000000000),
 ( 0.9484916720352057906, 0.7930602363642083041, 1.000000000000000000),
 ( 0.9484506837745732000, 0.7928955620037245744, 1.000000000000000000),
 ( 0.9483757353755084551, 0.7925944494535770435, 1.000000000000000000),
 ( 0.9483428265590246875, 0.7924622350530370340, 1.000000000000000000),
 ( 0.9482982329828737456, 0.7922830759835624015, 1.000000000000000000),
 ( 0.9482841625340747704, 0.7922265465743627555, 1.000000000000000000),
 ( 0.9482574280669420208, 0.7921191382284120674, 1.000000000000000000),
 ( 0.9482447675118421682, 0.7920682732055432940, 1.000000000000000000),
 ( 0.9482098218232999365, 0.7919278754715699531, 1.000000000000000000),
 ( 0.9481899903031330012, 0.7918482003926456958, 1.000000000000000000),
 ( 0.9481627597725135193, 0.7917387990629434213, 1.000000000000000000),
 ( 0.9481555257785727608, 0.7917097357822004966, 1.000000000000000000),
 ( 0.9481610290116149198, 0.7917318455611419559, 1.000000000000000000) ) ) 
 REPRESENTATION_ITEM ( '' )  SURFACE ( )  );
#23463 = CARTESIAN_POINT ( 'NONE',  ( 0.02395668684128875181, -0.5542051941014292105, 0.2488759775346758019 ) ) ;
#23465 = DIRECTION ( 'NONE',  ( 0.8660512985181133550, 0.4999551463232372872, 0.000000000000000000 ) ) ;
#23464 = CARTESIAN_POINT ( 'NONE',  ( 0.6845627961534704875, -1.503898997149517580, 0.4557198836646339513 ) ) ;
#23466 = SPHERICAL_SURFACE ( 'NONE', #37879, 0.01499999999999999944 ) ;
#23467 = APPLIED_APPROVAL_ASSIGNMENT ( #37929, ( #3089 ) ) ;
#23468 = CARTESIAN_POINT ( 'NONE',  ( 0.03824833094100624220, -1.739503649588687750, -0.3347792643966959747 ) ) ;
#23469 = ORIENTED_EDGE ( 'NONE', *, *, #4199, .F. ) ;
#23470 = AXIS2_PLACEMENT_3D ( 'NONE', #34714, #22598, #25474 ) ;
#23471 = CARTESIAN_POINT ( 'NONE',  ( 0.5033392876442730479, -1.584769073138426299, -0.5496476129754243045 ) ) ;
#23472 = CARTESIAN_POINT ( 'NONE',  ( 0.01895884884825219455, 0.5124024296374549703, 0.08888335629180021957 ) ) ;
#23473 = CARTESIAN_POINT ( 'NONE',  ( 0.3806020551634139437, -1.255922899846727558, 0.6160997750454292321 ) ) ;
#23474 = CARTESIAN_POINT ( 'NONE',  ( 0.5923740993416417577, -1.483515408114672418, 0.6326167027179712132 ) ) ;
#23475 = CARTESIAN_POINT ( 'NONE',  ( 0.4940945688342389119, -1.677685676440951790, -0.6095800757797251723 ) ) ;
#23476 = CARTESIAN_POINT ( 'NONE',  ( -0.1710642717598274409, 0.4986889574319069429, 0.3078512670230414972 ) ) ;
#23477 = CARTESIAN_POINT ( 'NONE',  ( -0.2399999999999999079, -2.909786385774835171, -0.3705357231075770419 ) ) ;
#23478 = CARTESIAN_POINT ( 'NONE',  ( 0.4266844285874258902, -1.124162052474312334, 0.5132868267961471220 ) ) ;
#23479 = DIRECTION ( 'NONE',  ( 0.8614903136912356318, 0.5077740042737285409, 1.079459829625176262E-11 ) ) ;
#23480 = PERSON_AND_ORGANIZATION ( #28500, #32463 ) ;
#23481 = CIRCLE ( 'NONE', #12952, 0.1033070866141734129 ) ;
#23482 = CARTESIAN_POINT ( 'NONE',  ( 0.4009842110195314113, -1.137333063945437095, 0.4310421439394608312 ) ) ;
#23483 = CARTESIAN_POINT ( 'NONE',  ( 0.4138729472876766513, -1.128955312352843965, 0.5470489658417444501 ) ) ;
#23484 = FACE_OUTER_BOUND ( 'NONE', #11840, .T. ) ;
#23485 = CARTESIAN_POINT ( 'NONE',  ( -2.112273405726188513E-14, -2.183180860297921466, -0.4937760292030871079 ) ) ;
#23486 = CARTESIAN_POINT ( 'NONE',  ( 0.5989748564488622806, -1.469694812953115548, 0.6043986940112930917 ) ) ;
#23487 = CARTESIAN_POINT ( 'NONE',  ( 0.1798183621851980052, -1.228826535827538757, 1.015400663858992081 ) ) ;
#23488 = LINE ( 'NONE', #17497, #29661 ) ;
#23489 = EDGE_CURVE ( 'NONE', #1703, #35767, #22835, .T. ) ;
#23490 = ORIENTED_EDGE ( 'NONE', *, *, #22498, .T. ) ;
#23491 = ORIENTED_EDGE ( 'NONE', *, *, #6996, .F. ) ;
#23492 = CARTESIAN_POINT ( 'NONE',  ( 0.1755412408656793488, -0.5236575430993549718, 0.09909328031171654727 ) ) ;
#23493 = VERTEX_POINT ( 'NONE', #22572 ) ;
#23494 = CARTESIAN_POINT ( 'NONE',  ( -0.2746410161513776482, -3.941790907013290823, -0.4709369376873030477 ) ) ;
#23496 = ORIENTED_EDGE ( 'NONE', *, *, #30846, .T. ) ;
#23495 = CARTESIAN_POINT ( 'NONE',  ( 0.6020063251545132443, -1.483136369781559383, 0.5737255376849879074 ) ) ;
#23498 = VERTEX_POINT ( 'NONE', #28313 ) ;
#23497 = CARTESIAN_POINT ( 'NONE',  ( -0.0001984217570695264842, -0.7096501419610361516, -0.02101570025487809953 ) ) ;
#23499 = ORIENTED_EDGE ( 'NONE', *, *, #36363, .F. ) ;
#23500 = CARTESIAN_POINT ( 'NONE',  ( 0.1153472973656773787, -0.4465945704133856831, 0.1832744267750886502 ) ) ;
#23501 = EDGE_LOOP ( 'NONE', ( #11895, #9014, #36273, #36065 ) ) ;
#23502 = EDGE_CURVE ( 'NONE', #5888, #32180, #23771, .T. ) ;
#23503 = CARTESIAN_POINT ( 'NONE',  ( 0.004648077331195073561, -0.6786668696663772371, 0.5213953154864034989 ) ) ;
#23505 = DIRECTION ( 'NONE',  ( -1.000000000000000000, 0.000000000000000000, 0.000000000000000000 ) ) ;
#23504 = DIRECTION ( 'NONE',  ( -0.9379438357983841401, -0.2431488234232593582, 0.2472650613323660318 ) ) ;
#23506 = PRODUCT_RELATED_PRODUCT_CATEGORY ( 'detail', '', ( #13386 ) ) ;
#23507 = LINE ( 'NONE', #23088, #31215 ) ;
#23508 = ITEM_DEFINED_TRANSFORMATION ( 'NONE', 'NONE', #10158,  #27819 ) ;
#23509 = CARTESIAN_POINT ( 'NONE',  ( 0.004042983189834512686, -0.6339827964191876442, 0.09509064842808945262 ) ) ;
#23511 = ORIENTED_EDGE ( 'NONE', *, *, #28029, .T. ) ;
#23510 = ORIENTED_EDGE ( 'NONE', *, *, #17720, .F. ) ;
#23512 = CARTESIAN_POINT ( 'NONE',  ( 0.08690321595024325108, -0.7908715706426733272, 0.2150688980104960291 ) ) ;
#23513 = CARTESIAN_POINT ( 'NONE',  ( 0.03292036658315200537, -0.9539746468707878124, 0.6379772252982135461 ) ) ;
#23514 = CARTESIAN_POINT ( 'NONE',  ( 0.07425324393167602455, -0.5797589466047996520, 0.2935359610363197369 ) ) ;
#23515 = CARTESIAN_POINT ( 'NONE',  ( 0.4275179515708005251, -1.300593502282117564, 0.8352946709572205419 ) ) ;
#23516 = CARTESIAN_POINT ( 'NONE',  ( 0.05301051884385669932, -1.209477745581631680, 0.6633383430279803372 ) ) ;
#23517 = LINE ( 'NONE', #915, #27748 ) ;
#23518 = CARTESIAN_POINT ( 'NONE',  ( 0.06936654275850007156, -1.327133429011322141, 0.5458395137742464431 ) ) ;
#23519 = CARTESIAN_POINT ( 'NONE',  ( 0.4097635862714068544, -1.729374185699168232, -0.4282187442611350425 ) ) ;
#23520 = CARTESIAN_POINT ( 'NONE',  ( 0.6867864222940462948, -1.415806215839816140, 0.6057417262805012692 ) ) ;
#23521 = AXIS2_PLACEMENT_3D ( 'NONE', #31558, #31772, #26175 ) ;
#23522 = CARTESIAN_POINT ( 'NONE',  ( 0.07043814880410806389, -1.334972480813829021, 0.5056242588139847616 ) ) ;
#23523 = DIRECTION ( 'NONE',  ( 0.000000000000000000, -5.463695987328525648E-15, -1.000000000000000000 ) ) ;
#23524 = CARTESIAN_POINT ( 'NONE',  ( -0.0001820817997102400665, -0.8409590828520395744, -0.05113895155038358786 ) ) ;
#23525 = CARTESIAN_POINT ( 'NONE',  ( 0.4776172972151280782, -1.293649847444084289, 0.8149156285371210728 ) ) ;
#23526 = LINE ( 'NONE', #32749, #28632 ) ;
#23527 = CARTESIAN_POINT ( 'NONE',  ( -0.1172100234506837091, -0.4874937943216617331, 0.3357378396897056083 ) ) ;
#23528 = EDGE_CURVE ( 'NONE', #29395, #18399, #15242, .T. ) ;
#23529 = CARTESIAN_POINT ( 'NONE',  ( 0.05848126963139189949, -0.9969932945501481791, 0.7623047753129613691 ) ) ;
#23530 = CARTESIAN_POINT ( 'NONE',  ( 0.4927680500253098783, -1.082617619565096723, 0.5740975660237009892 ) ) ;
#23531 = EDGE_CURVE ( 'NONE', #10991, #8795, #13903, .T. ) ;
#23532 = PERSON_AND_ORGANIZATION ( #28500, #32463 ) ;
#23533 = CARTESIAN_POINT ( 'NONE',  ( 0.2020777887685438201, -0.5385241820806814239, 0.3979124043150588097 ) ) ;
#23534 = ADVANCED_FACE ( 'NONE', ( #22782 ), #13289, .F. ) ;
#23535 = EDGE_CURVE ( 'NONE', #16052, #26041, #19819, .T. ) ;
#23536 = CARTESIAN_POINT ( 'NONE',  ( -3.757258772823647403E-22, 0.06117178301711218014, -0.1249999999999999029 ) ) ;
#23537 = EDGE_CURVE ( 'NONE', #25449, #2897, #763, .T. ) ;
#23538 = DIRECTION ( 'NONE',  ( 0.4379975771764356707, -0.8989761522908004121, 0.000000000000000000 ) ) ;
#23539 = ORIENTED_EDGE ( 'NONE', *, *, #26401, .F. ) ;
#23540 = CARTESIAN_POINT ( 'NONE',  ( 0.03333333333331219700, -2.097675824466503691, -0.7286991843995640483 ) ) ;
#23541 = CARTESIAN_POINT ( 'NONE',  ( 0.03395086281050493232, -0.7332833338886608487, 0.5887985628043005404 ) ) ;
#23542 = CARTESIAN_POINT ( 'NONE',  ( 0.1136746601619137848, -1.290010351664979016, 0.4385763861344814663 ) ) ;
#23544 = EDGE_LOOP ( 'NONE', ( #15604, #38120, #40429 ) ) ;
#23543 = CARTESIAN_POINT ( 'NONE',  ( 0.3874305626238240263, -1.778265208088890104, -0.4824895240968558596 ) ) ;
#23545 = CARTESIAN_POINT ( 'NONE',  ( 0.3253942984295454255, -1.752804437849984076, 0.4715143984075212402 ) ) ;
#23546 = CARTESIAN_POINT ( 'NONE',  ( 0.5484444682544461491, -1.189958873811490347, 0.8086343185444866410 ) ) ;
#23548 = EDGE_LOOP ( 'NONE', ( #10886, #29200, #14482, #3530 ) ) ;
#23547 = VERTEX_POINT ( 'NONE', #17937 ) ;
#23549 = CARTESIAN_POINT ( 'NONE',  ( 0.009515880660224757676, -1.737226041143324684, -0.6384574844869379540 ) ) ;
#23550 = ORIENTED_EDGE ( 'NONE', *, *, #39431, .T. ) ;
#23551 = CARTESIAN_POINT ( 'NONE',  ( 0.3568217579247562887, -1.837974685081549708, -0.5015348115105691118 ) ) ;
#23552 = EDGE_CURVE ( 'NONE', #16489, #15152, #6004, .T. ) ;
#23553 = CARTESIAN_POINT ( 'NONE',  ( -0.1710642718812828145, 0.4986889572247755198, 0.3749999999999990008 ) ) ;
#23554 = CARTESIAN_POINT ( 'NONE',  ( -0.03877220711930485370, 0.4416859332762665402, -0.1784371778270208153 ) ) ;
#23555 = VERTEX_POINT ( 'NONE', #38378 ) ;
#23556 = CYLINDRICAL_SURFACE ( 'NONE', #38966, 0.04249999999999995448 ) ;
#23557 = CARTESIAN_POINT ( 'NONE',  ( 0.08875147084456934399, -0.6445117467991269278, 0.1562688198774206394 ) ) ;
#23558 = CARTESIAN_POINT ( 'NONE',  ( 0.2811027414035134897, -1.594431497873851189, 0.9549070678298874348 ) ) ;
#23559 = CARTESIAN_POINT ( 'NONE',  ( 0.4989807694161794704, -1.541666567615755490, 0.6106768752493882957 ) ) ;
#23561 = FACE_OUTER_BOUND ( 'NONE', #9867, .T. ) ;
#23560 = CARTESIAN_POINT ( 'NONE',  ( 0.1139602419629163615, -0.5599708880517814125, -0.05895036679083177911 ) ) ;
#23562 = CARTESIAN_POINT ( 'NONE',  ( 0.07287665493537502648, -1.000988532525567631, 0.5315438341818862211 ) ) ;
#23563 = VERTEX_POINT ( 'NONE', #30494 ) ;
#23564 = VERTEX_POINT ( 'NONE', #25860 ) ;
#23565 = CARTESIAN_POINT ( 'NONE',  ( 0.3303481907406706219, -1.638360797784888190, 0.5482645839017932232 ) ) ;
#23566 = CARTESIAN_POINT ( 'NONE',  ( 0.2248424822466164874, -0.6656341711533926286, 0.4617182395505510795 ) ) ;
#23567 = CARTESIAN_POINT ( 'NONE',  ( 0.4441836334028864686, -1.145505455753590196, -0.6481113851292223949 ) ) ;
#23568 =( BOUNDED_SURFACE ( )  B_SPLINE_SURFACE ( 3, 2, ( 
 ( #31174, #12630, #34652 ),
 ( #24600, #30757, #36921 ),
 ( #31378, #37738, #2988 ),
 ( #40003, #15539, #28272 ),
 ( #11825, #34040, #27883 ),
 ( #18402, #9559, #21314 ),
 ( #40420, #34449, #24386 ),
 ( #8736, #28090, #15112 ),
 ( #15723, #6262, #21920 ),
 ( #2778, #33851, #40617 ),
 ( #12248, #2576, #6048 ),
 ( #22137, #18834, #37517 ),
 ( #18000, #30559, #3182 ),
 ( #40204, #24985, #37328 ),
 ( #37135, #18616, #9138 ),
 ( #137, #34238, #2382 ),
 ( #9339, #27478, #18208 ),
 ( #21704, #30954, #27672 ),
 ( #8949, #21523, #38549 ),
 ( #26217, #22938, #6652 ),
 ( #22739, #7255, #15928 ),
 ( #28476, #23139, #3791 ),
 ( #13650, #37945, #558 ),
 ( #31769, #952, #19026 ),
 ( #38739, #10564, #6455 ),
 ( #31556, #3373, #10171 ),
 ( #12852, #35055, #10375 ),
 ( #35453, #351, #25414 ) ),
 .UNSPECIFIED., .F., .F., .T. ) 
 B_SPLINE_SURFACE_WITH_KNOTS ( ( 4, 2, 2, 2, 2, 2, 2, 2, 2, 2, 2, 2, 2, 4 ),
 ( 3, 3 ),
 ( 0.03544507920328695411, 0.03595486840377590254, 0.03646465760426484404, 0.03748423600524272703, 0.03952339280719850689, 0.04156254960915428676, 0.04360170641111006662, 0.04462128481208795655, 0.04564086321306584648, 0.04768002001502162635, 0.04869959841599951628, 0.04971917681697740621, 0.05073875521795528920, 0.05175833361893317913 ),
 ( 0.000000000000000000, 1.000000000000000000 ),
 .UNSPECIFIED. ) 
 GEOMETRIC_REPRESENTATION_ITEM ( )  RATIONAL_B_SPLINE_SURFACE ( (
 ( 1.000000000000000000, 0.7061763356917282186, 1.000000000000000000),
 ( 1.000000000000000000, 0.7080421523057279787, 1.000000000000000000),
 ( 1.000000000000000000, 0.7088516299600189363, 1.000000000000000000),
 ( 1.000000000000000000, 0.7099244856010646920, 1.000000000000000000),
 ( 1.000000000000000000, 0.7101378557341009312, 1.000000000000000000),
 ( 1.000000000000000000, 0.7103445576143324613, 1.000000000000000000),
 ( 1.000000000000000000, 0.7098994762787453894, 1.000000000000000000),
 ( 1.000000000000000000, 0.7079279405282516979, 1.000000000000000000),
 ( 1.000000000000000000, 0.7057284653322816181, 1.000000000000000000),
 ( 1.000000000000000000, 0.7007157790497101635, 1.000000000000000000),
 ( 1.000000000000000000, 0.6978342510162478529, 1.000000000000000000),
 ( 1.000000000000000000, 0.6916754492645889041, 1.000000000000000000),
 ( 1.000000000000000000, 0.6883795134656507386, 1.000000000000000000),
 ( 1.000000000000000000, 0.6835032746938722870, 1.000000000000000000),
 ( 1.000000000000000000, 0.6818926907723115161, 1.000000000000000000),
 ( 1.000000000000000000, 0.6788412388327624836, 1.000000000000000000),
 ( 1.000000000000000000, 0.6773936298796268130, 1.000000000000000000),
 ( 1.000000000000000000, 0.6736810316134190790, 1.000000000000000000),
 ( 1.000000000000000000, 0.6720343155085293230, 1.000000000000000000),
 ( 1.000000000000000000, 0.6725111439841665595, 1.000000000000000000),
 ( 1.000000000000000000, 0.6731816333784381712, 1.000000000000000000),
 ( 1.000000000000000000, 0.6757599976966006672, 1.000000000000000000),
 ( 1.000000000000000000, 0.6776668555841935948, 1.000000000000000000),
 ( 1.000000000000000000, 0.6829223581646010066, 1.000000000000000000),
 ( 1.000000000000000000, 0.6862934035413943423, 1.000000000000000000),
 ( 1.000000000000000000, 0.6945721712650553270, 1.000000000000000000),
 ( 1.000000000000000000, 0.6994068901145207295, 1.000000000000000000),
 ( 1.000000000000000000, 0.7048795877316381686, 1.000000000000000000) ) ) 
 REPRESENTATION_ITEM ( '' )  SURFACE ( )  );
#23569 = CARTESIAN_POINT ( 'NONE',  ( -0.03674260963082443682, -0.4681940304452939516, -0.1092801147583400689 ) ) ;
#23570 = CARTESIAN_POINT ( 'NONE',  ( 0.07300061029741421181, -1.320382841123569628, 0.5080970089286546143 ) ) ;
#23571 = DIRECTION ( 'NONE',  ( -1.000000000000000000, -0.000000000000000000, -0.000000000000000000 ) ) ;
#23572 = CARTESIAN_POINT ( 'NONE',  ( 0.6159793682513172719, -1.299209393623256492, 0.5257027981018284057 ) ) ;
#23573 = EDGE_CURVE ( 'NONE', #507, #24616, #34087, .T. ) ;
#23574 = CARTESIAN_POINT ( 'NONE',  ( -0.1155415985277065405, -0.5283611291160981160, 0.1337613384747777245 ) ) ;
#23575 = EDGE_CURVE ( 'NONE', #10025, #35098, #30980, .T. ) ;
#23576 = DIRECTION ( 'NONE',  ( 0.8660254037844391517, 0.4259456949666812209, 0.2618592464270645404 ) ) ;
#23577 = CARTESIAN_POINT ( 'NONE',  ( 0.4382015218937659884, -1.612541052972227940, -0.6615483979663951963 ) ) ;
#23578 = CARTESIAN_POINT ( 'NONE',  ( -0.05283719472145156915, -0.03966590960886421519, -0.4666299489511761545 ) ) ;
#23579 = EDGE_CURVE ( 'NONE', #7024, #7215, #12593, .T. ) ;
#23580 = CARTESIAN_POINT ( 'NONE',  ( -0.02238765564325697829, -0.2417679119117833453, -0.4518160092940294859 ) ) ;
#23581 = VERTEX_POINT ( 'NONE', #29342 ) ;
#23582 = ADVANCED_FACE ( 'NONE', ( #5375 ), #10214, .T. ) ;
#23583 = CARTESIAN_POINT ( 'NONE',  ( 0.4475429125754209481, -1.047523227676938173, 0.7185146543629753468 ) ) ;
#23584 = CARTESIAN_POINT ( 'NONE',  ( 0.03113248654051816583, 0.7171888913565960255, -0.2950238883388468514 ) ) ;
#23585 = CARTESIAN_POINT ( 'NONE',  ( -0.02953079040095652960, 0.3810518745593862167, -0.3687679460475775106 ) ) ;
#23586 = CARTESIAN_POINT ( 'NONE',  ( 0.2791220714032659478, -1.321220139306267471, 0.5682417262808748815 ) ) ;
#23587 = EDGE_LOOP ( 'NONE', ( #38232, #1056, #6907, #40529 ) ) ;
#23588 = CARTESIAN_POINT ( 'NONE',  ( -0.1969433606228600808, 0.5138636982738217229, 0.1528658435937000626 ) ) ;
#23589 = EDGE_CURVE ( 'NONE', #2842, #2874, #39515, .T. ) ;
#23590 = CARTESIAN_POINT ( 'NONE',  ( 0.6603083091704677887, -1.500180305189478425, -0.4119820518570970758 ) ) ;
#23591 = CARTESIAN_POINT ( 'NONE',  ( -0.2399999999999999079, -2.761122741982423801, -0.2878817176880067996 ) ) ;
#23592 = ADVANCED_FACE ( 'NONE', ( #35703 ), #14042, .F. ) ;
#23593 = DIRECTION ( 'NONE',  ( 2.157041537713701966E-32, -0.8709776783778060416, 0.4913225862583635584 ) ) ;
#23594 = CARTESIAN_POINT ( 'NONE',  ( 0.4540954970294862059, -1.215799341954577395, 0.6428014875294941755 ) ) ;
#23596 = DIRECTION ( 'NONE',  ( 7.771561172376107616E-16, -7.170354002788761615E-17, 1.000000000000000000 ) ) ;
#23595 = CARTESIAN_POINT ( 'NONE',  ( 0.05999999999999990757, -0.3458405862425447119, -0.1052451372150005060 ) ) ;
#23597 = CARTESIAN_POINT ( 'NONE',  ( -0.03650581953630641779, -0.2290855126858369062, -0.4575806651622373877 ) ) ;
#23598 = VERTEX_POINT ( 'NONE', #14866 ) ;
#23599 = EDGE_CURVE ( 'NONE', #12802, #16220, #22482, .T. ) ;
#23600 = CARTESIAN_POINT ( 'NONE',  ( 0.5860257985473389386, -1.592810714289445650, 0.4182417262808776903 ) ) ;
#23601 = ORIENTED_EDGE ( 'NONE', *, *, #12838, .T. ) ;
#23602 = CARTESIAN_POINT ( 'NONE',  ( -0.2399999999999999079, -4.289222312108804225, -0.5708809693675255259 ) ) ;
#23603 = ADVANCED_FACE ( 'NONE', ( #33986 ), #4039, .F. ) ;
#23604 = CARTESIAN_POINT ( 'NONE',  ( 0.4144077979564601555, -1.589676522203103959, 0.5854317008102997155 ) ) ;
#23606 = CARTESIAN_POINT ( 'NONE',  ( 0.4806378395295555772, -1.105637800341301880, -0.6194292131661299772 ) ) ;
#23605 = CARTESIAN_POINT ( 'NONE',  ( 0.06873388849150627311, -0.5537460360556609729, 0.08262749772200221610 ) ) ;
#23607 = FACE_OUTER_BOUND ( 'NONE', #20538, .T. ) ;
#23608 = ORIENTED_EDGE ( 'NONE', *, *, #14806, .T. ) ;
#23609 = ORIENTED_EDGE ( 'NONE', *, *, #24842, .T. ) ;
#23610 = CYLINDRICAL_SURFACE ( 'NONE', #25422, 0.5400000000000019229 ) ;
#23611 = CARTESIAN_POINT ( 'NONE',  ( 0.3556566238030725580, -1.130358669023453722, 0.8129044222785481999 ) ) ;
#23612 = VERTEX_POINT ( 'NONE', #24329 ) ;
#23613 = FACE_OUTER_BOUND ( 'NONE', #5644, .T. ) ;
#23614 = CARTESIAN_POINT ( 'NONE',  ( 0.03174060074381315766, -0.4701996045334360663, 0.2325360656122961167 ) ) ;
#23615 = CARTESIAN_POINT ( 'NONE',  ( 0.3744966970941377982, -1.755388072428740065, -0.4336563827106933444 ) ) ;
#23616 = CARTESIAN_POINT ( 'NONE',  ( 0.2037257193243683095, -1.237902000685740633, 0.4623145460830584974 ) ) ;
#23617 = CARTESIAN_POINT ( 'NONE',  ( -0.1696282724551531063, 0.4941130859153644028, 0.1349535128744439594 ) ) ;
#23618 = CARTESIAN_POINT ( 'NONE',  ( 0.3895925628365914939, -1.758298928368249525, -0.4737392274988301288 ) ) ;
#23619 = CARTESIAN_POINT ( 'NONE',  ( 0.6565177652365870031, -1.363219716956428407, 0.8083140950016142190 ) ) ;
#23620 = DIRECTION ( 'NONE',  ( -1.387778780781449423E-15, 6.545052484820649979E-16, -1.000000000000000000 ) ) ;
#23621 = SPHERICAL_SURFACE ( 'NONE', #23861, 0.01499999999999999944 ) ;
#23622 = EDGE_CURVE ( 'NONE', #1137, #29592, #32966, .T. ) ;
#23623 = CARTESIAN_POINT ( 'NONE',  ( 0.6175558182517195682, -1.622344311396844097, -0.4976589326200486219 ) ) ;
#23624 = CARTESIAN_POINT ( 'NONE',  ( 0.2326005804937198163, -1.348008995865297432, 0.5133468128822303855 ) ) ;
#23625 = CARTESIAN_POINT ( 'NONE',  ( 0.1844128417485024762, -0.6074837269968395015, -0.01383500138692834829 ) ) ;
#23626 = EDGE_CURVE ( 'NONE', #36543, #12532, #28033, .T. ) ;
#23627 = CARTESIAN_POINT ( 'NONE',  ( 0.3690965330173307524, -1.099411688709415413, 0.5182417262812423209 ) ) ;
#23628 = DIRECTION ( 'NONE',  ( -1.000000000000000000, -0.000000000000000000, -0.000000000000000000 ) ) ;
#23629 = CARTESIAN_POINT ( 'NONE',  ( 0.002083146443013504916, -0.4777046557262296100, 0.1457185332388684640 ) ) ;
#23630 = CARTESIAN_POINT ( 'NONE',  ( 0.5852709255473115268, -1.480800356531663198, -0.6004500878436644928 ) ) ;
#23631 = LINE ( 'NONE', #16423, #19305 ) ;
#23632 = CARTESIAN_POINT ( 'NONE',  ( 0.5977452740392612540, -1.597648098397363547, 0.4278779530986268620 ) ) ;
#23633 = CARTESIAN_POINT ( 'NONE',  ( -0.05489899477340625528, -0.2921074789649947823, 0.3589041746640633246 ) ) ;
#23634 = ORIENTED_EDGE ( 'NONE', *, *, #17491, .T. ) ;
#23635 = ORIENTED_EDGE ( 'NONE', *, *, #34653, .T. ) ;
#23636 = DIRECTION ( 'NONE',  ( 0.4999551463232372317, -0.8660512985181135770, 0.000000000000000000 ) ) ;
#23637 = CARTESIAN_POINT ( 'NONE',  ( 0.3207919832889619127, -1.182535135427784878, 0.4177417262808780229 ) ) ;
#23638 = ORIENTED_EDGE ( 'NONE', *, *, #12490, .F. ) ;
#23639 = FACE_OUTER_BOUND ( 'NONE', #49, .T. ) ;
#23640 = CARTESIAN_POINT ( 'NONE',  ( 0.01899496522502858512, 0.2428513482851171745, -0.4597779644694632295 ) ) ;
#23641 = CARTESIAN_POINT ( 'NONE',  ( 0.5550199683367226244, -1.387812963830668211, 0.6052661460963145723 ) ) ;
#23642 = B_SPLINE_CURVE_WITH_KNOTS ( 'NONE', 3,
 ( #38725, #32155, #13828, #23334 ),
 .UNSPECIFIED., .F., .F.,
 ( 4, 4 ),
 ( 0.000000000000000000, 0.001818400350217978930 ),
 .UNSPECIFIED. ) ;
#23644 = ORIENTED_EDGE ( 'NONE', *, *, #4525, .T. ) ;
#23643 = CARTESIAN_POINT ( 'NONE',  ( -0.1673869564144402633, 0.4868872877193594073, 0.1265580611896349461 ) ) ;
#23645 = CARTESIAN_POINT ( 'NONE',  ( 0.1971950993027475063, -0.8036775079564704161, 0.3187204964795984363 ) ) ;
#23646 = DIRECTION ( 'NONE',  ( -0.8660512985181135770, -0.4999551463232371207, 0.000000000000000000 ) ) ;
#23647 = VERTEX_POINT ( 'NONE', #18553 ) ;
#23648 = DIRECTION ( 'NONE',  ( 0.9378410757839518164, -0.1072489841977738861, -0.3300784330442475545 ) ) ;
#23649 = CARTESIAN_POINT ( 'NONE',  ( 0.02340052157832292826, -0.5442089205427294019, 0.2181755822959388913 ) ) ;
#23651 = CARTESIAN_POINT ( 'NONE',  ( 0.1141259082751814175, -0.5391003347981141447, -0.04436171186494073521 ) ) ;
#23650 = CARTESIAN_POINT ( 'NONE',  ( 0.6570310456701250468, -1.541036513631718785, 0.4253474239190344064 ) ) ;
#23652 = CARTESIAN_POINT ( 'NONE',  ( 0.3207919832889619127, -1.182535135427784878, 0.4177417262808780229 ) ) ;
#23653 = CARTESIAN_POINT ( 'NONE',  ( -0.08000000000000000167, -2.551729310907437043, -0.4286726180052709001 ) ) ;
#23654 = ORIENTED_EDGE ( 'NONE', *, *, #27391, .F. ) ;
#23655 = CARTESIAN_POINT ( 'NONE',  ( 0.000000000000000000, 0.000000000000000000, 0.000000000000000000 ) ) ;
#23656 = CARTESIAN_POINT ( 'NONE',  ( 0.6984663268742642428, -1.558725849730709934, -0.5155029497116575543 ) ) ;
#23657 = CARTESIAN_POINT ( 'NONE',  ( 0.01548846960712797240, 0.5203207976466739382, 0.08861466064782476393 ) ) ;
#23658 = CARTESIAN_POINT ( 'NONE',  ( 0.08269480835304590660, -0.8371205904093916850, 0.2823278632619380391 ) ) ;
#23659 = CARTESIAN_POINT ( 'NONE',  ( 0.1832580928828051736, -1.261492888555858505, -0.3231111295750616619 ) ) ;
#23660 = CARTESIAN_POINT ( 'NONE',  ( 0.4867251962510119045, -1.680960026995096612, -0.6125153944539966089 ) ) ;
#23661 = CARTESIAN_POINT ( 'NONE',  ( 0.3203156827224240555, -1.053479473948887080, 0.6335618240576057492 ) ) ;
#23662 = CARTESIAN_POINT ( 'NONE',  ( -0.1211791774340214151, -0.5069275750892356935, 0.1468366819525818712 ) ) ;
#23663 = FACE_BOUND ( 'NONE', #32827, .T. ) ;
#23664 = FACE_OUTER_BOUND ( 'NONE', #37201, .T. ) ;
#23665 = LINE ( 'NONE', #16883, #5533 ) ;
#23666 = APPROVAL_ROLE ( '' ) ;
#23667 = CARTESIAN_POINT ( 'NONE',  ( 0.009587871238832338869, -0.9974913955574146174, 0.5289707807213344104 ) ) ;
#23668 = CARTESIAN_POINT ( 'NONE',  ( 0.5594945947431219091, -1.182971886111896964, 0.6057417262809814407 ) ) ;
#23669 = PRODUCT_DEFINITION_CONTEXT ( 'detailed design', #17419, 'design' ) ;
#23670 = DIRECTION ( 'NONE',  ( -0.5963781153887844910, -0.3442778833694402074, -0.7251247358268644305 ) ) ;
#23671 = CARTESIAN_POINT ( 'NONE',  ( 0.3655440060901842259, -1.768235641947720094, -0.5860794697665872022 ) ) ;
#23672 = CARTESIAN_POINT ( 'NONE',  ( 0.1142751706468553285, -0.9924943110554562686, 0.9292056703508084770 ) ) ;
#23673 = AXIS2_PLACEMENT_3D ( 'NONE', #16429, #25921, #19719 ) ;
#23674 = DIRECTION ( 'NONE',  ( 1.000000000000000000, -0.000000000000000000, -0.000000000000000000 ) ) ;
#23675 = VERTEX_POINT ( 'NONE', #31110 ) ;
#23676 = ORIENTED_EDGE ( 'NONE', *, *, #4989, .F. ) ;
#23677 = CARTESIAN_POINT ( 'NONE',  ( 0.1870046356540934207, -0.5056247393092100362, 0.1384337335614591047 ) ) ;
#23678 = VERTEX_POINT ( 'NONE', #37463 ) ;
#23679 = B_SPLINE_CURVE_WITH_KNOTS ( 'NONE', 3,
 ( #1322, #7452, #25590, #7052, #35036, #3777, #32348, #31751, #3570, #38932, #35253, #16138, #28870, #19426, #28676, #543, #20027, #25801 ),
 .UNSPECIFIED., .F., .F.,
 ( 4, 2, 2, 2, 2, 2, 2, 2, 4 ),
 ( -0.002633528389679722949, -0.001975271857855722454, -0.001317015326031721958, -0.0006587587942077214632, -5.022623837209680420E-07, 0.0006577542694402795272, 0.001316010801264280022, 0.001974267333088280084, 0.002632523864912281013 ),
 .UNSPECIFIED. ) ;
#23680 = CARTESIAN_POINT ( 'NONE',  ( 0.4768848212686893073, -1.682051206446435465, -0.4156371400837834407 ) ) ;
#23682 = ORIENTED_EDGE ( 'NONE', *, *, #5622, .T. ) ;
#23681 = CARTESIAN_POINT ( 'NONE',  ( 0.6013823673879303833, -1.482980318010622911, 0.5610683146295102341 ) ) ;
#23684 = ORIENTED_EDGE ( 'NONE', *, *, #1446, .F. ) ;
#23683 = CARTESIAN_POINT ( 'NONE',  ( -0.001060993694459935396, -0.7858254716106745086, 0.01975934941180707005 ) ) ;
#23685 = VERTEX_POINT ( 'NONE', #36855 ) ;
#23686 = CARTESIAN_POINT ( 'NONE',  ( 0.3084843299837661257, -1.189417664086780846, 0.5254903229641211260 ) ) ;
#23687 = ORIENTED_EDGE ( 'NONE', *, *, #38499, .T. ) ;
#23688 = CARTESIAN_POINT ( 'NONE',  ( 0.2616305944698923969, -1.623119320148453726, 0.8135356459590667999 ) ) ;
#23690 = CARTESIAN_POINT ( 'NONE',  ( 0.4356662251172991329, -1.610775558009423847, -0.3686272921855576756 ) ) ;
#23689 = CARTESIAN_POINT ( 'NONE',  ( 0.01548846960707524721, 0.000000000000000000, 0.000000000000000000 ) ) ;
#23691 = CARTESIAN_POINT ( 'NONE',  ( 0.6379434534673991131, -1.610984557855128951, -0.4725373547503501359 ) ) ;
#23692 = CONTEXT_DEPENDENT_SHAPE_REPRESENTATION ( #9012, #14061 ) ;
#23693 = CARTESIAN_POINT ( 'NONE',  ( -0.1603938765018562418, 0.4636889572247986369, 0.3382895567582878127 ) ) ;
#23695 = VERTEX_POINT ( 'NONE', #12380 ) ;
#23694 = VERTEX_POINT ( 'NONE', #5590 ) ;
#23696 = DIRECTION ( 'NONE',  ( -1.000000000000000000, 0.000000000000000000, 0.000000000000000000 ) ) ;
#23697 = CARTESIAN_POINT ( 'NONE',  ( 0.07318559350598305424, -1.141632816824696750, 0.7599663268781896575 ) ) ;
#23698 = CARTESIAN_POINT ( 'NONE',  ( 0.07117412038449888456, -0.5606254895656045401, 0.2415125051803064526 ) ) ;
#23699 = CARTESIAN_POINT ( 'NONE',  ( 0.5523264011633536308, -1.510993508513732930, 0.5610637926937284137 ) ) ;
#23700 = CARTESIAN_POINT ( 'NONE',  ( 0.1837552442763759619, -0.5219052425814498797, 0.2609841535793563927 ) ) ;
#23701 = CARTESIAN_POINT ( 'NONE',  ( -0.07908070219616114560, -0.09959325338431368468, 0.1178658435936986715 ) ) ;
#23702 = FACE_OUTER_BOUND ( 'NONE', #1108, .T. ) ;
#23703 = CARTESIAN_POINT ( 'NONE',  ( 0.3786975293126830788, -1.707670322493268111, -0.4135462521370839029 ) ) ;
#23704 = CARTESIAN_POINT ( 'NONE',  ( 0.6982435741820434139, -1.438800902438351459, 0.5626105661469322783 ) ) ;
#23705 = CARTESIAN_POINT ( 'NONE',  ( 0.3830059406587226767, -1.662912566754132015, -0.6203890335291190050 ) ) ;
#23706 = DIRECTION ( 'NONE',  ( 0.000000000000000000, 0.000000000000000000, -1.000000000000000000 ) ) ;
#23707 = CIRCLE ( 'NONE', #9211, 0.2200000000000000566 ) ;
#23708 = DIRECTION ( 'NONE',  ( -2.465190328815661892E-32, -1.000000000000000000, -6.656013887802287108E-31 ) ) ;
#23709 = CARTESIAN_POINT ( 'NONE',  ( 0.4107682604834280715, -1.110406771794815395, 0.6170034175396635900 ) ) ;
#23710 = DIRECTION ( 'NONE',  ( 0.8660512985181134660, 0.4999551463232371762, 0.000000000000000000 ) ) ;
#23711 = AXIS2_PLACEMENT_3D ( 'NONE', #34248, #14730, #39826 ) ;
#23712 = CARTESIAN_POINT ( 'NONE',  ( 0.4567198261210261845, -1.219045092035883293, 0.5856983068965102568 ) ) ;
#23713 = CARTESIAN_POINT ( 'NONE',  ( 0.002392376194700432737, -0.7211561054371403712, 0.3442605867753443794 ) ) ;
#23714 = CARTESIAN_POINT ( 'NONE',  ( 0.4922096163030106331, -1.082311226180449504, 0.5799505941865350511 ) ) ;
#23715 = APPROVAL_ROLE ( '' ) ;
#23716 = CARTESIAN_POINT ( 'NONE',  ( 0.2114022633412600827, -0.5658596150412534831, 0.4491712673773823883 ) ) ;
#23717 = APPROVAL ( #28539, 'UNKNOWN' ) ;
#23718 = CARTESIAN_POINT ( 'NONE',  ( 0.06045346506656550795, 0.05436763897581790156, -0.1249999999999999029 ) ) ;
#23719 = CARTESIAN_POINT ( 'NONE',  ( 0.3061274744420098282, -1.759189183208312413, 0.5682166201788007021 ) ) ;
#23720 = ORIENTED_EDGE ( 'NONE', *, *, #28489, .F. ) ;
#23721 = CARTESIAN_POINT ( 'NONE',  ( -0.2399999999999999079, -2.139295658456680904, -0.3624034539465684213 ) ) ;
#23722 = CARTESIAN_POINT ( 'NONE',  ( 0.1171733338514413247, -1.124504233628559779, 0.8957213136541929410 ) ) ;
#23723 = CIRCLE ( 'NONE', #5969, 0.9237847906030155487 ) ;
#23724 = DIRECTION ( 'NONE',  ( -0.3468893892380672250, 0.3199132558031694828, -0.8816593788961000211 ) ) ;
#23726 = ORIENTED_EDGE ( 'NONE', *, *, #34113, .F. ) ;
#23725 = CARTESIAN_POINT ( 'NONE',  ( 0.3842204440267534826, -1.812485869991422804, -0.5233031296161457790 ) ) ;
#23727 = CARTESIAN_POINT ( 'NONE',  ( 0.1323926191616460191, 0.05688556330967539654, -0.02068925706491322666 ) ) ;
#23728 = APPLICATION_CONTEXT ( 'configuration controlled 3d designs of mechanical parts and assemblies' ) ;
#23729 = CARTESIAN_POINT ( 'NONE',  ( 0.6117231882494743589, -1.284912631992666254, 0.6460020013211499323 ) ) ;
#23731 = ORIENTED_EDGE ( 'NONE', *, *, #36298, .F. ) ;
#23730 = ORIENTED_EDGE ( 'NONE', *, *, #22276, .F. ) ;
#23732 = CARTESIAN_POINT ( 'NONE',  ( 0.05254288559145195436, -1.595463313323315369, -0.6695117733422313311 ) ) ;
#23733 = CONICAL_SURFACE ( 'NONE', #14523, 0.1600000000000006417, 1.047197551196599408 ) ;
#23734 = ORIENTED_EDGE ( 'NONE', *, *, #35783, .T. ) ;
#23735 = EDGE_CURVE ( 'NONE', #5937, #24586, #18149, .T. ) ;
#23736 = CARTESIAN_POINT ( 'NONE',  ( 0.6576035064516577711, -1.449376941801497454, -0.4138723806928110704 ) ) ;
#23737 = PLANE ( 'NONE',  #19996 ) ;
#23738 = PERSON_AND_ORGANIZATION ( #28003, #37829 ) ;
#23739 = AXIS2_PLACEMENT_3D ( 'NONE', #30901, #28221, #30708 ) ;
#23740 = CARTESIAN_POINT ( 'NONE',  ( -2.070754768975505034, -0.09959325338431362917, 0.3749999999999976130 ) ) ;
#23741 = ORIENTED_EDGE ( 'NONE', *, *, #2960, .F. ) ;
#23742 = DIRECTION ( 'NONE',  ( 5.551115123125790098E-17, -3.676620095425088700E-16, -1.000000000000000000 ) ) ;
#23743 = CARTESIAN_POINT ( 'NONE',  ( 0.2317368684993577621, -0.9096491609996487648, 0.6759228893237037017 ) ) ;
#23744 = EDGE_CURVE ( 'NONE', #31843, #28184, #9983, .T. ) ;
#23745 = CARTESIAN_POINT ( 'NONE',  ( 0.1346410849617742378, -1.067092216287955697, 0.9652224197926299043 ) ) ;
#23746 = CARTESIAN_POINT ( 'NONE',  ( 0.4970208778649962134, -1.542363045560136037, 0.5660616863803898946 ) ) ;
#23748 = CARTESIAN_POINT ( 'NONE',  ( -0.1142976700078418423, -0.5226524673290435796, 0.1219895833617483799 ) ) ;
#23747 = CARTESIAN_POINT ( 'NONE',  ( 0.2580594912783656381, -1.598602451500839683, 0.8570735393225172860 ) ) ;
#23749 = CARTESIAN_POINT ( 'NONE',  ( 0.1941099092474980470, -0.9693953940917349188, 0.5071542142353313576 ) ) ;
#23750 = ORIENTED_EDGE ( 'NONE', *, *, #34045, .F. ) ;
#23751 = VERTEX_POINT ( 'NONE', #6201 ) ;
#23752 = EDGE_CURVE ( 'NONE', #19390, #1288, #14553, .T. ) ;
#23753 = ADVANCED_FACE ( 'NONE', ( #28216 ), #83, .F. ) ;
#23754 = CARTESIAN_POINT ( 'NONE',  ( 0.02953079040095673430, -0.5250338024619269905, -0.07436286310882420092 ) ) ;
#23755 = CIRCLE ( 'NONE', #34929, 0.01000000000000001582 ) ;
#23756 = CARTESIAN_POINT ( 'NONE',  ( 0.2578022185847296810, -0.7392430535719961560, 0.5549718881115695002 ) ) ;
#23757 = ADVANCED_FACE ( 'NONE', ( #18968 ), #27426, .F. ) ;
#23758 = B_SPLINE_CURVE_WITH_KNOTS ( 'NONE', 3,
 ( #21784, #33933, #5732, #18290, #30830 ),
 .UNSPECIFIED., .F., .F.,
 ( 4, 1, 4 ),
 ( 0.003975523017580754465, 0.004090739973965718326, 0.004205956930350682188 ),
 .UNSPECIFIED. ) ;
#23759 = CARTESIAN_POINT ( 'NONE',  ( -0.1443375672974067936, 0.08000000000000023759, 0.000000000000000000 ) ) ;
#23760 = CARTESIAN_POINT ( 'NONE',  ( -0.05269191099235819714, -0.4470515771378631431, -0.1405532101198447847 ) ) ;
#23761 = AXIS2_PLACEMENT_3D ( 'NONE', #23949, #33387, #5191 ) ;
#23762 = DIRECTION ( 'NONE',  ( -1.000000000000000000, -0.000000000000000000, -0.000000000000000000 ) ) ;
#23763 = CARTESIAN_POINT ( 'NONE',  ( 0.3950375043453270285, -1.756612718480099034, -0.7128469446588594494 ) ) ;
#23764 = AXIS2_PLACEMENT_3D ( 'NONE', #12344, #3695, #9450 ) ;
#23765 = DIRECTION ( 'NONE',  ( 0.4999551463232371762, -0.8660512985181134660, 0.000000000000000000 ) ) ;
#23766 = CARTESIAN_POINT ( 'NONE',  ( 0.3392765801623501276, -0.9012043381553855870, 0.6651284465457234507 ) ) ;
#23767 = AXIS2_PLACEMENT_3D ( 'NONE', #4241, #35715, #26466 ) ;
#23768 = DIRECTION ( 'NONE',  ( 0.000000000000000000, 0.000000000000000000, -1.000000000000000000 ) ) ;
#23769 = EDGE_CURVE ( 'NONE', #27736, #2583, #275, .T. ) ;
#23770 = APPLIED_PERSON_AND_ORGANIZATION_ASSIGNMENT ( #10312, #29620, ( #4217 ) ) ;
#23771 = CIRCLE ( 'NONE', #27722, 0.04330708661417322775 ) ;
#23772 = CARTESIAN_POINT ( 'NONE',  ( 0.02953079040094805374, 0.5250338024619489730, -0.07436286310882397887 ) ) ;
#23773 = CARTESIAN_POINT ( 'NONE',  ( 0.1499999999999994671, 0.5203207976467936202, 0.08861466064782093366 ) ) ;
#23774 = EDGE_LOOP ( 'NONE', ( #13609, #16161, #964, #24345 ) ) ;
#23775 = CARTESIAN_POINT ( 'NONE',  ( 0.01548846960707511190, -0.5198120922912051745, -0.07362328916749329155 ) ) ;
#23776 = CARTESIAN_POINT ( 'NONE',  ( 0.2456699162554547011, -1.579418306085378143, -0.3207381830095928921 ) ) ;
#23777 = ORIENTED_EDGE ( 'NONE', *, *, #11400, .T. ) ;
#23778 = CARTESIAN_POINT ( 'NONE',  ( 0.3199600894486596125, -0.9236621663148832928, 0.6127110118620351376 ) ) ;
#23779 = LINE ( 'NONE', #36297, #37049 ) ;
#23780 = AXIS2_PLACEMENT_3D ( 'NONE', #40435, #12054, #14937 ) ;
#23781 = CARTESIAN_POINT ( 'NONE',  ( 0.08749854297545196780, -0.9854861971012113253, 0.6823029913621244669 ) ) ;
#23782 = ORIENTED_EDGE ( 'NONE', *, *, #29831, .F. ) ;
#23783 = CARTESIAN_POINT ( 'NONE',  ( 0.04293701532779510555, 0.3457382709204490090, 0.3536859687696371490 ) ) ;
#23784 = CARTESIAN_POINT ( 'NONE',  ( 0.4110399549994251389, -1.609958759213365953, -0.3626335216686736862 ) ) ;
#23785 = CARTESIAN_POINT ( 'NONE',  ( 0.5382307432915078849, -1.161159458769174257, 0.5682417262808779901 ) ) ;
#23786 = FACE_OUTER_BOUND ( 'NONE', #37350, .T. ) ;
#23787 = CARTESIAN_POINT ( 'NONE',  ( 0.3774258077853776538, -1.121343430727174795, 0.7058894445193834022 ) ) ;
#23788 = CIRCLE ( 'NONE', #19809, 0.07749999999977555398 ) ;
#23790 = CARTESIAN_POINT ( 'NONE',  ( 0.3174226411910346934, -1.752965763378658393, 0.5310945280258847490 ) ) ;
#23789 = CARTESIAN_POINT ( 'NONE',  ( -0.2746410161513779258, -2.139295658456680904, -0.2024034539465678073 ) ) ;
#23791 = CARTESIAN_POINT ( 'NONE',  ( 0.2098534808732534784, -0.9273921219866952947, 0.3620977009047463002 ) ) ;
#23792 = ORIENTED_EDGE ( 'NONE', *, *, #9532, .T. ) ;
#23793 = B_SPLINE_CURVE_WITH_KNOTS ( 'NONE', 3,
 ( #27306, #14740, #17624, #39233, #8548, #29759, #17422, #11454, #39834, #2199 ),
 .UNSPECIFIED., .F., .F.,
 ( 4, 2, 2, 2, 4 ),
 ( 0.000000000000000000, 0.0007867799123170480082, 0.001573559824634096016, 0.002360339736951139796, 0.003147119649268183793 ),
 .UNSPECIFIED. ) ;
#23794 = CARTESIAN_POINT ( 'NONE',  ( 0.5926726610113466354, -1.589034138814389374, 0.4182417262808776903 ) ) ;
#23795 = ORIENTED_EDGE ( 'NONE', *, *, #38693, .F. ) ;
#23796 = EDGE_CURVE ( 'NONE', #25380, #22378, #37891, .T. ) ;
#23797 = VECTOR ( 'NONE', #663, 39.37007874015748143 ) ;
#23798 =( BOUNDED_SURFACE ( )  B_SPLINE_SURFACE ( 3, 2, ( 
 ( #36230, #8044, #23518 ),
 ( #33156, #20828, #4961 ),
 ( #36444, #1904, #14416 ),
 ( #26978, #27193, #23913 ) ),
 .UNSPECIFIED., .F., .F., .F. ) 
 B_SPLINE_SURFACE_WITH_KNOTS ( ( 4, 4 ),
 ( 3, 3 ),
 ( -1.546505978833323525E-15, 0.0005696895415557860689 ),
 ( 0.000000000000000000, 1.000000000000000000 ),
 .UNSPECIFIED. ) 
 GEOMETRIC_REPRESENTATION_ITEM ( )  RATIONAL_B_SPLINE_SURFACE ( (
 ( 1.000000000000000000, 0.7101913118100382505, 1.000000000000000000),
 ( 1.000000000000000000, 0.7102645811962934319, 1.000000000000000000),
 ( 1.000000000000000000, 0.7103277044789075845, 1.000000000000000000),
 ( 1.000000000000000000, 0.7103763540285419342, 1.000000000000000000) ) ) 
 REPRESENTATION_ITEM ( '' )  SURFACE ( )  );
#23799 = CARTESIAN_POINT ( 'NONE',  ( -0.3000000000000000999, -2.377058624452622393, -0.8919706583825134372 ) ) ;
#23800 = AXIS2_PLACEMENT_3D ( 'NONE', #28817, #7002, #7602 ) ;
#23801 = CARTESIAN_POINT ( 'NONE',  ( 0.1377409401209249984, -0.8452087646918974295, 0.6880418428642343098 ) ) ;
#23803 = CARTESIAN_POINT ( 'NONE',  ( 0.1897655176910530150, -0.7785539449726521788, 0.2985823049966282450 ) ) ;
#23802 = CARTESIAN_POINT ( 'NONE',  ( 0.08759928954965089110, -0.6793946942812071343, 0.02269552198566341175 ) ) ;
#23804 = CARTESIAN_POINT ( 'NONE',  ( 0.1459220268477366689, -1.282677086676273337, 0.4807434598447087870 ) ) ;
#23805 = ORIENTED_EDGE ( 'NONE', *, *, #40593, .T. ) ;
#23806 = AXIS2_PLACEMENT_3D ( 'NONE', #1579, #8527, #35918 ) ;
#23807 = EDGE_CURVE ( 'NONE', #34947, #27531, #11952, .T. ) ;
#23808 = VERTEX_POINT ( 'NONE', #10108 ) ;
#23809 = DIRECTION ( 'NONE',  ( -8.881784197001246407E-16, 2.361472542561082612E-16, -1.000000000000000000 ) ) ;
#23810 = EDGE_CURVE ( 'NONE', #3794, #7197, #15208, .T. ) ;
#23811 = CARTESIAN_POINT ( 'NONE',  ( 0.2982777979521030742, -1.009191457843666040, 0.7688872764601440979 ) ) ;
#23812 = ORIENTED_EDGE ( 'NONE', *, *, #9495, .F. ) ;
#23813 = DIRECTION ( 'NONE',  ( 0.4999551463232372317, -0.8660512985181135770, 0.000000000000000000 ) ) ;
#23814 = CARTESIAN_POINT ( 'NONE',  ( 0.02953079040095346608, -0.4684706630666200522, 0.2484463060367382847 ) ) ;
#23815 = CARTESIAN_POINT ( 'NONE',  ( 0.3694954200858134863, -1.765954564873332355, -0.4302357760272142451 ) ) ;
#23816 = CARTESIAN_POINT ( 'NONE',  ( 0.1941405844127271907, -1.254956905737245609, 0.4467041655102085840 ) ) ;
#23817 = CARTESIAN_POINT ( 'NONE',  ( -0.1687956829044073848, 0.4914472887403515400, 0.1310621546645155122 ) ) ;
#23818 = CARTESIAN_POINT ( 'NONE',  ( 0.3939846702892026986, -1.751817380748406539, -0.4710255994886535236 ) ) ;
#23819 = CARTESIAN_POINT ( 'NONE',  ( 0.6491914112794352487, -1.351404041023776204, 0.8153926641961858346 ) ) ;
#23820 = DIRECTION ( 'NONE',  ( 0.000000000000000000, 0.000000000000000000, -1.000000000000000000 ) ) ;
#23821 = EDGE_CURVE ( 'NONE', #24506, #34622, #29021, .T. ) ;
#23822 = DIRECTION ( 'NONE',  ( 1.000000000000000000, -0.000000000000000000, -0.000000000000000000 ) ) ;
#23823 = CIRCLE ( 'NONE', #39528, 0.07999999999999996003 ) ;
#23824 = CARTESIAN_POINT ( 'NONE',  ( 0.6115442966349228238, -1.578889019291040530, -0.5746358093662063959 ) ) ;
#23825 = CARTESIAN_POINT ( 'NONE',  ( 0.05561310505367080687, 0.2541457526436888825, 0.3845267872006546961 ) ) ;
#23826 = CARTESIAN_POINT ( 'NONE',  ( 0.5727340295961615979, -1.614449106656711708, 0.5626663476171955836 ) ) ;
#23827 = CARTESIAN_POINT ( 'NONE',  ( -0.02000000000000000042, -2.070343076906777213, -0.2454056712452573896 ) ) ;
#23828 = CARTESIAN_POINT ( 'NONE',  ( 0.1060996949738549772, -1.304465968667597675, 0.4400741763124171313 ) ) ;
#23829 = AXIS2_PLACEMENT_3D ( 'NONE', #11343, #20827, #2086 ) ;
#23830 = CIRCLE ( 'NONE', #24497, 0.1000000000000000194 ) ;
#23831 = CARTESIAN_POINT ( 'NONE',  ( 0.2920835003669574048, -1.623987781970284594, 0.9481157836879084977 ) ) ;
#23832 = CARTESIAN_POINT ( 'NONE',  ( 0.5726340570884991266, -1.543972946347143882, -0.4961447500887076201 ) ) ;
#23833 = CARTESIAN_POINT ( 'NONE',  ( -0.2399999999999999079, -1.891808285041389093, -0.4498908273618595910 ) ) ;
#23834 = CARTESIAN_POINT ( 'NONE',  ( 0.3048131552638332353, -1.756863458444712700, 0.5686633310820135012 ) ) ;
#23835 = CARTESIAN_POINT ( 'NONE',  ( -0.05187277790672315675, -0.2620383623028431641, 0.3911539469301649752 ) ) ;
#23837 = ORIENTED_EDGE ( 'NONE', *, *, #29419, .T. ) ;
#23836 = B_SPLINE_SURFACE_WITH_KNOTS ( 'NONE', 3, 3, ( 
 ( #546, #338, #7241, #19817 ),
 ( #12842, #32351, #29290, #1138 ),
 ( #26205, #14649, #4381, #1741 ),
 ( #38936, #36056, #29480, #36467 ),
 ( #5178, #36249, #20641, #8282 ),
 ( #32566, #16939, #2113, #23540 ),
 ( #8067, #13831, #29683, #20426 ) ),
 .UNSPECIFIED., .F., .F., .F.,
 ( 4, 1, 1, 1, 4 ),
 ( 4, 4 ),
 ( 0.000000000000000000, 0.2500000000000000000, 0.5000000000000000000, 0.7500000000000000000, 1.000000000000000000 ),
 ( 0.000000000000000000, 1.000000000000000000 ),
 .UNSPECIFIED. ) ;
#23838 = CARTESIAN_POINT ( 'NONE',  ( 0.4733616728321626832, -1.077395945196840010, -0.6087806452432535931 ) ) ;
#23839 = CARTESIAN_POINT ( 'NONE',  ( 0.4093611158985690501, -1.131941421409890403, 0.5197417262808780025 ) ) ;
#23840 = DIRECTION ( 'NONE',  ( 0.8660512985181133550, 0.4999551463232371207, 0.000000000000000000 ) ) ;
#23841 = CARTESIAN_POINT ( 'NONE',  ( -0.1684323895664520399, 0.5231977504174887272, 0.3032895567580809471 ) ) ;
#23842 = CARTESIAN_POINT ( 'NONE',  ( 0.5042534145799544287, -1.300931244380588714, 0.7003810967224629591 ) ) ;
#23844 = ORIENTED_EDGE ( 'NONE', *, *, #20575, .T. ) ;
#23843 = CARTESIAN_POINT ( 'NONE',  ( -0.05083665881509057127, 0.4630607685881610869, 0.09936361682460814748 ) ) ;
#23845 = CARTESIAN_POINT ( 'NONE',  ( 0.3550363906115478474, -0.9559691138050746551, 0.6482402363088731745 ) ) ;
#23846 = CARTESIAN_POINT ( 'NONE',  ( 0.005339406051279861967, -1.804346059958628068, -0.3571184395977468062 ) ) ;
#23847 = ORIENTED_EDGE ( 'NONE', *, *, #10752, .T. ) ;
#23848 = DIRECTION ( 'NONE',  ( 0.000000000000000000, 0.000000000000000000, -1.000000000000000000 ) ) ;
#23849 = EDGE_LOOP ( 'NONE', ( #35173, #15920 ) ) ;
#23850 = CARTESIAN_POINT ( 'NONE',  ( 0.3578840571904184364, -1.622517175314822202, 0.6005136135349141702 ) ) ;
#23852 = CARTESIAN_POINT ( 'NONE',  ( 0.1882261734610965742, -0.5202158445490479011, 0.1262989087885288408 ) ) ;
#23851 = CARTESIAN_POINT ( 'NONE',  ( 0.6889712424111062994, -1.498443914574956848, 0.4645504256959663847 ) ) ;
#23853 = CARTESIAN_POINT ( 'NONE',  ( 0.01548846960712783535, -0.5203207976466778240, -0.08861466064782558272 ) ) ;
#23854 = AXIS2_PLACEMENT_3D ( 'NONE', #25335, #31089, #31490 ) ;
#23855 = ADVANCED_FACE ( 'NONE', ( #35213 ), #25354, .F. ) ;
#23856 = CARTESIAN_POINT ( 'NONE',  ( 0.05999999999999990757, 0.2463462108298974940, -0.03520871226632921180 ) ) ;
#23857 = ORIENTED_EDGE ( 'NONE', *, *, #13643, .F. ) ;
#23858 = VERTEX_POINT ( 'NONE', #32302 ) ;
#23859 = CARTESIAN_POINT ( 'NONE',  ( -1.651713865843977279E-05, -2.061678968352038233, -0.6852225792402809601 ) ) ;
#23860 = FACE_OUTER_BOUND ( 'NONE', #32116, .T. ) ;
#23861 = AXIS2_PLACEMENT_3D ( 'NONE', #1821, #14337, #26900 ) ;
#23862 = CIRCLE ( 'NONE', #33021, 0.05330708661417321581 ) ;
#23863 = CARTESIAN_POINT ( 'NONE',  ( 0.1863649894376638305, -1.020275744783735838, 0.7192912599071568103 ) ) ;
#23864 = CARTESIAN_POINT ( 'NONE',  ( 0.3540817610093318635, -1.633452470505663667, 0.5182417262812423209 ) ) ;
#23865 = CIRCLE ( 'NONE', #14642, 0.01999999999999927530 ) ;
#23866 = DIRECTION ( 'NONE',  ( -8.881784197001246407E-16, 2.361472542561082612E-16, -1.000000000000000000 ) ) ;
#23867 = B_SPLINE_CURVE_WITH_KNOTS ( 'NONE', 3,
 ( #15185, #30827, #17860, #33700 ),
 .UNSPECIFIED., .F., .F.,
 ( 4, 4 ),
 ( 1.734723475976807094E-18, 0.0003603784013037980918 ),
 .UNSPECIFIED. ) ;
#23868 = CARTESIAN_POINT ( 'NONE',  ( 0.1501646858415086605, -0.9504056024928764224, 0.4235331231779344008 ) ) ;
#23869 = CARTESIAN_POINT ( 'NONE',  ( -0.1163549140004290217, -0.5320595946631634376, 0.1429098354138644833 ) ) ;
#23870 = FACE_OUTER_BOUND ( 'NONE', #30959, .T. ) ;
#23871 = CARTESIAN_POINT ( 'NONE',  ( 0.7215184893803678889, -1.528098279142000804, -0.6250000000000000000 ) ) ;
#23872 = DIRECTION ( 'NONE',  ( -1.000000000000000000, -0.000000000000000000, -0.000000000000000000 ) ) ;
#23873 = COORDINATED_UNIVERSAL_TIME_OFFSET ( 0, 0, .AHEAD. ) ;
#23874 = ADVANCED_FACE ( 'NONE', ( #10324 ), #16689, .F. ) ;
#23875 = APPLIED_DATE_AND_TIME_ASSIGNMENT ( #18570, #35616, ( #18145 ) ) ;
#23876 = EDGE_CURVE ( 'NONE', #13895, #3745, #1092, .T. ) ;
#23877 = CARTESIAN_POINT ( 'NONE',  ( 0.01555240294579989489, -1.032170008678823470, 0.5911815370100742539 ) ) ;
#23878 = CARTESIAN_POINT ( 'NONE',  ( -0.05464101615137773038, -2.626773565144302935, -0.1926934094652516249 ) ) ;
#23879 = CARTESIAN_POINT ( 'NONE',  ( -0.2746410161513776482, -4.289222312108804225, -0.5708809693675255259 ) ) ;
#23880 = CARTESIAN_POINT ( 'NONE',  ( 0.0003443436031621042938, -0.4626201699786359756, 0.03852669977424470066 ) ) ;
#23881 = CARTESIAN_POINT ( 'NONE',  ( 0.3999999999999787059, -2.097675824466503691, -0.5196396315034578217 ) ) ;
#23882 = FACE_OUTER_BOUND ( 'NONE', #1598, .T. ) ;
#23883 = CARTESIAN_POINT ( 'NONE',  ( 0.2284923717121198627, -1.304659949875474068, -0.5155029497116575543 ) ) ;
#23884 = VERTEX_POINT ( 'NONE', #10503 ) ;
#23885 = AXIS2_PLACEMENT_3D ( 'NONE', #34735, #7144, #34941 ) ;
#23886 = VERTEX_POINT ( 'NONE', #15873 ) ;
#23887 = VECTOR ( 'NONE', #9227, 39.37007874015748143 ) ;
#23888 = CARTESIAN_POINT ( 'NONE',  ( 0.1871418833521726888, -0.5093494604625196098, 0.1906562654118973132 ) ) ;
#23889 = ORIENTED_EDGE ( 'NONE', *, *, #22800, .T. ) ;
#23890 = CARTESIAN_POINT ( 'NONE',  ( 0.4822598830809305959, -1.683537768409984592, -0.5984293649392239400 ) ) ;
#23891 = CARTESIAN_POINT ( 'NONE',  ( -0.2746410161513770931, -3.220869926774937664, -0.5656276768926112863 ) ) ;
#23893 = ORIENTED_EDGE ( 'NONE', *, *, #6693, .F. ) ;
#23892 = CARTESIAN_POINT ( 'NONE',  ( 0.0003935148711146671356, -0.6434531841869496338, -0.01657467902959560910 ) ) ;
#23894 = VECTOR ( 'NONE', #14295, 39.37007874015748143 ) ;
#23895 = VERTEX_POINT ( 'NONE', #31500 ) ;
#23896 = CARTESIAN_POINT ( 'NONE',  ( 0.5070565638186045332, -1.226247237694178427, 0.9020276881305223649 ) ) ;
#23897 = EDGE_LOOP ( 'NONE', ( #29745, #14201, #17339, #33124 ) ) ;
#23898 = AXIS2_PLACEMENT_3D ( 'NONE', #38970, #13859, #26436 ) ;
#23899 = CARTESIAN_POINT ( 'NONE',  ( 0.1990087807486831672, -1.411128265896168799, 0.9384327408913899493 ) ) ;
#23901 = CARTESIAN_POINT ( 'NONE',  ( 0.1831969519479068331, -1.238078994650575249, 0.5906457657967459918 ) ) ;
#23900 = CARTESIAN_POINT ( 'NONE',  ( 0.5934537061017988169, -1.599883771062468041, 0.4225983487168387120 ) ) ;
#23902 = CARTESIAN_POINT ( 'NONE',  ( 0.3999999999999786504, -1.973385418564556293, -0.6834611762463905782 ) ) ;
#23903 = CALENDAR_DATE ( 2026, 13, 10 ) ;
#23904 = ADVANCED_FACE ( 'NONE', ( #7014 ), #3824, .T. ) ;
#23905 = DIRECTION ( 'NONE',  ( -2.465190328815661892E-32, -1.000000000000000000, -6.656013887802287108E-31 ) ) ;
#23907 = VERTEX_POINT ( 'NONE', #1281 ) ;
#23906 = ORIENTED_EDGE ( 'NONE', *, *, #37063, .T. ) ;
#23908 = CARTESIAN_POINT ( 'NONE',  ( 0.01165244542177405231, -0.7705269947053657864, -0.09957348361509645029 ) ) ;
#23909 = CARTESIAN_POINT ( 'NONE',  ( 0.09220195039318782038, -1.256385609540978443, 0.7507312887929911138 ) ) ;
#23910 = CARTESIAN_POINT ( 'NONE',  ( 0.09649107927482511449, -0.5884850972898393318, 0.3050835042885340354 ) ) ;
#23911 = CARTESIAN_POINT ( 'NONE',  ( 0.01141274522673730620, -0.9470863358862970927, 0.2134741291574251409 ) ) ;
#23912 = CARTESIAN_POINT ( 'NONE',  ( -2.119743302583864240E-14, -2.097675824466504135, -0.7286991843995639373 ) ) ;
#23913 = CARTESIAN_POINT ( 'NONE',  ( 0.06843884545124433172, -1.327631889387169473, 0.5684120120348994387 ) ) ;
#23914 = CONICAL_SURFACE ( 'NONE', #21945, 0.2609684784060898322, 0.1745329251994329756 ) ;
#23915 = CARTESIAN_POINT ( 'NONE',  ( 0.4634712904840411762, -1.711704060178987241, -0.5155029497116575543 ) ) ;
#23916 = CARTESIAN_POINT ( 'NONE',  ( 0.4189043378923988925, -1.737431724743732753, -0.5872665585884508932 ) ) ;
#23917 = CARTESIAN_POINT ( 'NONE',  ( 0.3782552467915779593, -1.656602296218481207, -0.6321311662414380583 ) ) ;
#23918 = CIRCLE ( 'NONE', #14024, 0.7750185148639454624 ) ;
#23919 = DIRECTION ( 'NONE',  ( 0.01455087615875041117, 0.9998941303973198913, 0.000000000000000000 ) ) ;
#23920 = DIRECTION ( 'NONE',  ( -4.410796239770424606E-15, -0.4393346272636315941, 0.8983234858819654223 ) ) ;
#23921 = VECTOR ( 'NONE', #19725, 39.37007874015748143 ) ;
#23922 = CARTESIAN_POINT ( 'NONE',  ( 0.3965913301904485655, -1.111811593118467778, 0.6217369508112342569 ) ) ;
#23923 = CARTESIAN_POINT ( 'NONE',  ( 0.3832670810558529984, -1.653853153454119873, -0.3970663464927791098 ) ) ;
#23924 = DIRECTION ( 'NONE',  ( -1.000000000000000000, -0.000000000000000000, -0.000000000000000000 ) ) ;
#23925 = CARTESIAN_POINT ( 'NONE',  ( 0.05992416651567116642, -0.8828589634183678925, 0.7642515975180658172 ) ) ;
#23926 = AXIS2_PLACEMENT_3D ( 'NONE', #31992, #12648, #34669 ) ;
#23927 = CARTESIAN_POINT ( 'NONE',  ( 0.1856290495283919040, -0.8698730627085041744, 0.1722928722954065184 ) ) ;
#23928 = CALENDAR_DATE ( 2026, 13, 10 ) ;
#23929 = CARTESIAN_POINT ( 'NONE',  ( 0.1878356035704684124, -0.4698003021450733452, 0.2206963598966235063 ) ) ;
#23930 = AXIS2_PLACEMENT_3D ( 'NONE', #16306, #9340, #22898 ) ;
#23931 = ORIENTED_EDGE ( 'NONE', *, *, #16568, .T. ) ;
#23932 = EDGE_CURVE ( 'NONE', #16401, #33009, #20409, .T. ) ;
#23933 = CARTESIAN_POINT ( 'NONE',  ( 0.3822380469604623743, -1.608340248901213965, -0.6174813857019513241 ) ) ;
#23934 = CARTESIAN_POINT ( 'NONE',  ( 0.04575106512774701484, -0.06504741310981120017, -0.4827780559048409637 ) ) ;
#23935 = EDGE_LOOP ( 'NONE', ( #14202, #6445, #23638, #32428 ) ) ;
#23936 = DIRECTION ( 'NONE',  ( -8.881784197001245421E-16, 2.361472542561082612E-16, -1.000000000000000000 ) ) ;
#23937 = CARTESIAN_POINT ( 'NONE',  ( 0.1570928595072558498, -1.231659055714347417, 0.9252356148029357019 ) ) ;
#23938 = AXIS2_PLACEMENT_3D ( 'NONE', #7156, #10462, #16641 ) ;
#23940 = ORIENTED_EDGE ( 'NONE', *, *, #661, .T. ) ;
#23939 = FACE_OUTER_BOUND ( 'NONE', #12357, .T. ) ;
#23941 = CARTESIAN_POINT ( 'NONE',  ( 0.06619202177789897112, -1.328973388337416406, 0.5682286961285595295 ) ) ;
#23942 = CARTESIAN_POINT ( 'NONE',  ( 0.2055745749294108637, -0.6303510842867390274, 0.3631342511460070033 ) ) ;
#23944 = EDGE_LOOP ( 'NONE', ( #38144, #31510, #27126, #33735, #34203 ) ) ;
#23943 = ORIENTED_EDGE ( 'NONE', *, *, #27361, .F. ) ;
#23945 = CARTESIAN_POINT ( 'NONE',  ( 0.03990608087475910198, -1.702714339505654095, -0.6675373308980625531 ) ) ;
#23946 = AXIS2_PLACEMENT_3D ( 'NONE', #21514, #27663, #24590 ) ;
#23947 = VERTEX_POINT ( 'NONE', #29846 ) ;
#23948 = AXIS2_PLACEMENT_3D ( 'NONE', #3226, #15775, #31824 ) ;
#23949 = CARTESIAN_POINT ( 'NONE',  ( 0.1499999999999994671, -0.5230810839623352138, -0.1699593469062213591 ) ) ;
#23950 = APPROVAL_PERSON_ORGANIZATION ( #12723, #40334, #2861 ) ;
#23951 = PRODUCT_DEFINITION_SHAPE ( 'NONE', 'NONE',  #40654 ) ;
#23952 = LINE ( 'NONE', #17356, #13440 ) ;
#23953 = DATE_AND_TIME ( #21475, #12246 ) ;
#23954 = CARTESIAN_POINT ( 'NONE',  ( -0.04047161733260127431, 0.4536038223829612082, -0.2133268955647374676 ) ) ;
#23955 = VERTEX_POINT ( 'NONE', #20190 ) ;
#23956 = CARTESIAN_POINT ( 'NONE',  ( 0.1293727182780175788, -1.251705868455923243, 0.6057490510025627106 ) ) ;
#23957 = CARTESIAN_POINT ( 'NONE',  ( 0.2094105298161792195, -0.8866733143744640611, 0.6435963268220464828 ) ) ;
#23958 = CIRCLE ( 'NONE', #7503, 0.01499999999999995608 ) ;
#23959 = CARTESIAN_POINT ( 'NONE',  ( 0.2857211247607547855, -1.599410745080646956, 0.9638650573196021476 ) ) ;
#23960 = CARTESIAN_POINT ( 'NONE',  ( 0.09909590748669688809, -0.5670311656315165649, 0.2451387329811758886 ) ) ;
#23961 = AXIS2_PLACEMENT_3D ( 'NONE', #35993, #1079, #13589 ) ;
#23963 = DIRECTION ( 'NONE',  ( -1.000000000000000000, -1.448788479720435680E-15, 8.315531510821436104E-16 ) ) ;
#23962 = CARTESIAN_POINT ( 'NONE',  ( 0.1141128553655777061, -0.5404361383069915536, -0.04587327521813978209 ) ) ;
#23964 = CARTESIAN_POINT ( 'NONE',  ( 0.08997777199038561879, -1.272785463024103558, 0.6309002601239589447 ) ) ;
#23965 = ORIENTED_EDGE ( 'NONE', *, *, #11155, .T. ) ;
#23966 = ORIENTED_EDGE ( 'NONE', *, *, #17544, .F. ) ;
#23967 = CARTESIAN_POINT ( 'NONE',  ( 0.04293701532779490432, -0.4875995331660219478, -0.08291810260646698127 ) ) ;
#23968 = CARTESIAN_POINT ( 'NONE',  ( 0.2783458387688289570, -0.7789938178757523923, 0.5967641912780569102 ) ) ;
#23969 = DIRECTION ( 'NONE',  ( 0.8660512985181139101, 0.4999551463232366766, 0.000000000000000000 ) ) ;
#23970 = CARTESIAN_POINT ( 'NONE',  ( 0.3699999999999786793, -2.097675824466503691, -0.4856910779487875196 ) ) ;
#23971 = CARTESIAN_POINT ( 'NONE',  ( -0.05634115714581421769, -0.4348133112253127486, -0.1467699930803220698 ) ) ;
#23972 = DIRECTION ( 'NONE',  ( 0.4999551463232377313, -0.8660512985181132439, 0.000000000000000000 ) ) ;
#23973 = CARTESIAN_POINT ( 'NONE',  ( 0.4125827319849673658, -1.718883513293331555, -0.4950489522355766003 ) ) ;
#23974 = CARTESIAN_POINT ( 'NONE',  ( 0.3193812180522301869, -1.183103643414081807, 0.4697888944849939463 ) ) ;
#23975 = CARTESIAN_POINT ( 'NONE',  ( 0.4795791402848185725, -1.087578995800233095, 0.7487995513514865698 ) ) ;
#23976 = CIRCLE ( 'NONE', #18706, 0.1000000000000000194 ) ;
#23977 = SECURITY_CLASSIFICATION_LEVEL ( 'unclassified' ) ;
#23978 = AXIS2_PLACEMENT_3D ( 'NONE', #21922, #38137, #37739 ) ;
#23979 = CARTESIAN_POINT ( 'NONE',  ( 0.1499999999999994671, 0.3688619771572926309, -0.3775276577326977523 ) ) ;
#23980 = APPROVAL_PERSON_ORGANIZATION ( #37113, #20757, #8928 ) ;
#23981 = CARTESIAN_POINT ( 'NONE',  ( 0.03396956254496814182, -1.810633036012876618, -0.3262169007243910235 ) ) ;
#23982 = CARTESIAN_POINT ( 'NONE',  ( -2.070754768975509919, -0.09959325338431655739, 0.1000000000000005745 ) ) ;
#23983 = EDGE_CURVE ( 'NONE', #17499, #9507, #39299, .T. ) ;
#23984 = CARTESIAN_POINT ( 'NONE',  ( -0.3000000000000000999, -2.945416957892569521, -0.4639726661791638840 ) ) ;
#23985 = CARTESIAN_POINT ( 'NONE',  ( 0.5739612213088449710, -1.639306779899527555, 0.5182417262812423209 ) ) ;
#23986 = EDGE_CURVE ( 'NONE', #21612, #19731, #27686, .T. ) ;
#23987 = AXIS2_PLACEMENT_3D ( 'NONE', #40449, #31201, #34475 ) ;
#23988 = CARTESIAN_POINT ( 'NONE',  ( -0.04308745346420565087, -0.3346348984074261068, -0.3638093623074884486 ) ) ;
#23989 = EDGE_LOOP ( 'NONE', ( #21329, #34901, #37733, #27276 ) ) ;
#23990 = CARTESIAN_POINT ( 'NONE',  ( 0.3720834698793197837, -0.9620146622799481406, 0.6738924748705610313 ) ) ;
#23991 = EDGE_CURVE ( 'NONE', #36862, #38078, #29590, .T. ) ;
#23992 = DIRECTION ( 'NONE',  ( 0.8660512985181135770, 0.4999551463232372317, 0.000000000000000000 ) ) ;
#23993 = EDGE_CURVE ( 'NONE', #24718, #4481, #33324, .T. ) ;
#23994 = CARTESIAN_POINT ( 'NONE',  ( 0.1849629421863227541, -1.262760559472479116, 0.7247380077052344438 ) ) ;
#23995 = ORIENTED_EDGE ( 'NONE', *, *, #22058, .T. ) ;
#23996 = CARTESIAN_POINT ( 'NONE',  ( 0.03654364704248850432, 0.2290829176602898198, 0.4574690890339227489 ) ) ;
#23997 = PLANE ( 'NONE',  #31583 ) ;
#23998 = CARTESIAN_POINT ( 'NONE',  ( 0.3731443575968244608, -1.763008880570848147, -0.4358735606183953837 ) ) ;
#23999 = CARTESIAN_POINT ( 'NONE',  ( 0.1890666733121571796, -1.695896060689630946, -0.3290518381478249599 ) ) ;
#24000 = CARTESIAN_POINT ( 'NONE',  ( 0.4501467687945732710, -1.211961921974989753, 0.6678290789428007468 ) ) ;
#24002 = DIRECTION ( 'NONE',  ( 1.000000000000000000, -0.000000000000000000, -0.000000000000000000 ) ) ;
#24001 = DIRECTION ( 'NONE',  ( -1.000000000000000000, -2.403560570595279103E-31, 1.725633230170969455E-31 ) ) ;
#24003 = CARTESIAN_POINT ( 'NONE',  ( -0.02953079040095693900, -0.3810518745593889922, -0.3687679460475752902 ) ) ;
#24004 = ORIENTED_EDGE ( 'NONE', *, *, #17936, .F. ) ;
#24005 = AXIS2_PLACEMENT_3D ( 'NONE', #23154, #17373, #14077 ) ;
#24006 = ORIENTED_EDGE ( 'NONE', *, *, #3625, .T. ) ;
#24007 = CARTESIAN_POINT ( 'NONE',  ( 0.3764383192846859627, -1.163784862039349388, 0.4182417262808778569 ) ) ;
#24008 = VERTEX_POINT ( 'NONE', #39701 ) ;
#24009 = AXIS2_PLACEMENT_3D ( 'NONE', #5641, #27660, #3171 ) ;
#24010 = CARTESIAN_POINT ( 'NONE',  ( -0.02000000000000000042, -1.646519645934556131, -0.1171471737359304072 ) ) ;
#24011 = CARTESIAN_POINT ( 'NONE',  ( 0.4060240284916718512, -1.489574581569751199, 0.8154449424633511967 ) ) ;
#24012 = EDGE_CURVE ( 'NONE', #5937, #10562, #39424, .T. ) ;
#24014 = CARTESIAN_POINT ( 'NONE',  ( 0.1945633475659577505, -0.8045315353305676487, 0.2954283631093154727 ) ) ;
#24013 = CARTESIAN_POINT ( 'NONE',  ( 0.6754688192570067473, -1.566413995319801522, 0.6053351715126479293 ) ) ;
#24015 = CARTESIAN_POINT ( 'NONE',  ( 0.5763712271873797643, -1.496301764669956569, 0.4854925386805672427 ) ) ;
#24016 = PRODUCT_DEFINITION_FORMATION_WITH_SPECIFIED_SOURCE ( 'ANY', '', #29493, .NOT_KNOWN. ) ;
#24017 = APPROVAL ( #2633, 'UNSPECIFIED' ) ;
#24018 = VERTEX_POINT ( 'NONE', #17883 ) ;
#24019 = ORIENTED_EDGE ( 'NONE', *, *, #37818, .F. ) ;
#24020 = CARTESIAN_POINT ( 'NONE',  ( 0.3878952717463541866, -1.820239213664927691, -0.5225022260212327518 ) ) ;
#24021 = CARTESIAN_POINT ( 'NONE',  ( 0.5738576967776770621, -1.499251410920260152, 0.5722528306968517331 ) ) ;
#24022 = CIRCLE ( 'NONE', #23345, 0.009999999999999960310 ) ;
#24023 = CARTESIAN_POINT ( 'NONE',  ( 0.3853411735687863326, -1.756807109041631509, -0.4499573014711771846 ) ) ;
#24024 = CARTESIAN_POINT ( 'NONE',  ( 0.3621729297631758326, -1.619675390324748498, 0.6057417262804762892 ) ) ;
#24025 = CARTESIAN_POINT ( 'NONE',  ( 0.6510214958982905031, -1.549214841228496065, 0.4232660966085758369 ) ) ;
#24026 = CARTESIAN_POINT ( 'NONE',  ( 0.1669810943094347522, -1.270657801378861418, 0.4327140572190054102 ) ) ;
#24027 = DIRECTION ( 'NONE',  ( 0.4999551463232372317, -0.8660512985181133550, 0.000000000000000000 ) ) ;
#24028 = CARTESIAN_POINT ( 'NONE',  ( 0.3900349134625270553, -1.754097501170372775, -0.4603090518067394221 ) ) ;
#24029 = CARTESIAN_POINT ( 'NONE',  ( 0.7167626400851214719, -1.479603991551655895, 0.4558490598962456342 ) ) ;
#24030 = DIRECTION ( 'NONE',  ( 0.4999551463232373427, -0.8660512985181134660, 0.000000000000000000 ) ) ;
#24031 = CARTESIAN_POINT ( 'NONE',  ( -0.0004424791507732762593, -0.9367167129038181939, 0.1457185332388704069 ) ) ;
#24032 = AXIS2_PLACEMENT_3D ( 'NONE', #20565, #38662, #13964 ) ;
#24033 = CARTESIAN_POINT ( 'NONE',  ( 0.5748241391253147148, -1.612671306764259072, -0.5249618373864313181 ) ) ;
#24034 = CIRCLE ( 'NONE', #29929, 0.6115209409081865388 ) ;
#24035 = DIRECTION ( 'NONE',  ( 0.01254811300245564816, 0.8659344938869285579, 0.4999999971568664936 ) ) ;
#24036 = DIRECTION ( 'NONE',  ( -0.4999999999999968359, 0.4646411234949411884, -0.7308273574226419322 ) ) ;
#24037 = CARTESIAN_POINT ( 'NONE',  ( 0.6936858524652079749, -1.440596496979289265, 0.5164693539546609813 ) ) ;
#24038 = CARTESIAN_POINT ( 'NONE',  ( 0.08972986647850272890, -1.313679858983815230, 0.4566612845758172279 ) ) ;
#24039 = ADVANCED_FACE ( 'NONE', ( #3087 ), #34823, .T. ) ;
#24040 = APPROVAL_PERSON_ORGANIZATION ( #7111, #23717, #22798 ) ;
#24041 = CARTESIAN_POINT ( 'NONE',  ( 0.2750825180155820338, -1.558163865710181728, 0.9909808761736236260 ) ) ;
#24042 = CARTESIAN_POINT ( 'NONE',  ( 0.3807174028472657956, -1.746516858961833396, -0.5732035964501958070 ) ) ;
#24043 = ADVANCED_FACE ( 'NONE', ( #28177 ), #31272, .F. ) ;
#24044 = CARTESIAN_POINT ( 'NONE',  ( 0.4382015218937534429, -1.612541052972219724, -0.6615483979664105174 ) ) ;
#24045 = DIRECTION ( 'NONE',  ( 0.9998941247116546194, -0.01455087607601020239, 0.0001066420868422379362 ) ) ;
#24046 = EDGE_CURVE ( 'NONE', #23035, #15212, #13167, .T. ) ;
#24047 = VECTOR ( 'NONE', #12564, 39.37007874015748143 ) ;
#24048 = ORIENTED_EDGE ( 'NONE', *, *, #2991, .T. ) ;
#24049 = CARTESIAN_POINT ( 'NONE',  ( 0.4039231983721676134, -1.110675651203401948, 0.6196059181502108215 ) ) ;
#24050 =( BOUNDED_SURFACE ( )  B_SPLINE_SURFACE ( 3, 2, ( 
 ( #28408, #38671, #13772 ),
 ( #23662, #11301, #23869 ),
 ( #36186, #17483, #11104 ),
 ( #16880, #10695, #29421 ) ),
 .UNSPECIFIED., .F., .F., .T. ) 
 B_SPLINE_SURFACE_WITH_KNOTS ( ( 4, 4 ),
 ( 3, 3 ),
 ( 0.0007843053012490898077, 0.001168341556843950548 ),
 ( 0.000000000000000000, 1.000000000000000000 ),
 .UNSPECIFIED. ) 
 GEOMETRIC_REPRESENTATION_ITEM ( )  RATIONAL_B_SPLINE_SURFACE ( (
 ( 1.000000000000000000, 0.9117915798263362959, 1.000000000000000000),
 ( 1.000000000000000000, 0.9032018617293641194, 1.000000000000000000),
 ( 1.000000000000000000, 0.8990088477696668301, 1.000000000000000000),
 ( 1.000000000000000000, 0.8989970956543188452, 1.000000000000000000) ) ) 
 REPRESENTATION_ITEM ( '' )  SURFACE ( )  );
#24051 = CARTESIAN_POINT ( 'NONE',  ( 0.3643718150905314035, -1.122313172052715968, 0.6044674227507519371 ) ) ;
#24052 = DIRECTION ( 'NONE',  ( 1.707404996040162391E-15, 0.4393346272636243222, -0.8983234858819689750 ) ) ;
#24053 = CARTESIAN_POINT ( 'NONE',  ( -0.04293701532779600066, 0.3457382709204480653, -0.3536859687696375376 ) ) ;
#24054 = CARTESIAN_POINT ( 'NONE',  ( 0.4958217342451587406, -1.286626739914629614, 0.6909901939486514655 ) ) ;
#24056 = EDGE_LOOP ( 'NONE', ( #11190, #18935, #26962 ) ) ;
#24055 = CARTESIAN_POINT ( 'NONE',  ( -0.1665325656947614918, 0.5173663872579224998, 0.1272034666820887894 ) ) ;
#24057 = CARTESIAN_POINT ( 'NONE',  ( 0.5017447040277105419, -1.102516469585429260, 0.6180670868896422920 ) ) ;
#24058 = EDGE_LOOP ( 'NONE', ( #30291, #17618, #32471, #15924 ) ) ;
#24059 = DIRECTION ( 'NONE',  ( 0.000000000000000000, -0.9510565162951529761, 0.3090169943749491166 ) ) ;
#24060 = VERTEX_POINT ( 'NONE', #8620 ) ;
#24061 = CARTESIAN_POINT ( 'NONE',  ( 0.009884248493598344482, -0.5504904132058388022, 0.06650783079932308384 ) ) ;
#24062 = CARTESIAN_POINT ( 'NONE',  ( 0.3563132181259857645, -1.622456743041318594, 0.5765765839559005013 ) ) ;
#24063 = EDGE_CURVE ( 'NONE', #3794, #31075, #30165, .T. ) ;
#24065 = CARTESIAN_POINT ( 'NONE',  ( -0.04154009738085463754, -0.2902754972779529319, 0.3700679770908128496 ) ) ;
#24064 = CARTESIAN_POINT ( 'NONE',  ( 0.7086437989906794188, -1.516288493585639330, 0.5545215044661631065 ) ) ;
#24066 = DIRECTION ( 'NONE',  ( -7.771561172376107616E-16, 7.170354002788761615E-17, -1.000000000000000000 ) ) ;
#24067 = VERTEX_POINT ( 'NONE', #2876 ) ;
#24068 = TOROIDAL_SURFACE ( 'NONE', #20772, 0.9237847906030132172, 0.01499999999999999944 ) ;
#24069 = AXIS2_PLACEMENT_3D ( 'NONE', #17122, #7845, #35640 ) ;
#24070 = ORIENTED_EDGE ( 'NONE', *, *, #22274, .F. ) ;
#24071 = CARTESIAN_POINT ( 'NONE',  ( -2.112273405726188513E-14, -2.097675824466503691, -0.6968677163258658602 ) ) ;
#24072 = DIRECTION ( 'NONE',  ( 1.000000000000000000, 2.280301054154495132E-31, -1.664003471950577689E-31 ) ) ;
#24073 = CARTESIAN_POINT ( 'NONE',  ( 0.3229734859516730783, -1.276098296144065225, 0.6443918083873608760 ) ) ;
#24074 = SECURITY_CLASSIFICATION ( '', '', #21051 ) ;
#24075 = DIRECTION ( 'NONE',  ( 0.000000000000000000, 0.000000000000000000, 1.000000000000000000 ) ) ;
#24076 = DIRECTION ( 'NONE',  ( 1.702140497302373526E-12, -0.5877852522924708056, 0.8090169943749491166 ) ) ;
#24077 = AXIS2_PLACEMENT_3D ( 'NONE', #40289, #31257, #6342 ) ;
#24078 = ADVANCED_BREP_SHAPE_REPRESENTATION ( '', ( #32841, #27819 ), #30435 ) ;
#24079 = CARTESIAN_POINT ( 'NONE',  ( 0.1160572313976696857, -0.9313940905863343778, 0.2591244526804493131 ) ) ;
#24080 = FACE_OUTER_BOUND ( 'NONE', #4440, .T. ) ;
#24081 = DIRECTION ( 'NONE',  ( 0.9998941247116546194, -0.01455087607601020239, 0.0001066420868422379362 ) ) ;
#24082 = CARTESIAN_POINT ( 'NONE',  ( 0.6581239351981619246, -1.508981307375971026, 0.4182417262808776903 ) ) ;
#24083 = CARTESIAN_POINT ( 'NONE',  ( -0.2900000000000003131, 0.5182417262804744906, 0.3749999999999995004 ) ) ;
#24084 = PERSON_AND_ORGANIZATION ( #28500, #32463 ) ;
#24085 = CARTESIAN_POINT ( 'NONE',  ( 0.4752902067229345384, -1.128721034250735444, 0.4769721126355153107 ) ) ;
#24086 = CARTESIAN_POINT ( 'NONE',  ( 0.4091955671835494357, -1.131682303504549347, 0.5515612239602755151 ) ) ;
#24087 = EDGE_CURVE ( 'NONE', #641, #20865, #31056, .T. ) ;
#24088 = CARTESIAN_POINT ( 'NONE',  ( 0.01216095678309696802, -0.4295234428450211972, 0.1161211177829335195 ) ) ;
#24089 = DIRECTION ( 'NONE',  ( 0.4999999999999985567, 0.4646411234949399116, -0.7308273574226413771 ) ) ;
#24090 = ADVANCED_FACE ( 'NONE', ( #27979 ), #3302, .F. ) ;
#24091 = CARTESIAN_POINT ( 'NONE',  ( 0.007789957077748424150, -0.5295643729319113868, 0.4348223727464700650 ) ) ;
#24092 = VECTOR ( 'NONE', #14142, 39.37007874015748143 ) ;
#24093 = LINE ( 'NONE', #11724, #17085 ) ;
#24094 = EDGE_CURVE ( 'NONE', #22420, #20653, #13483, .T. ) ;
#24095 = ORIENTED_EDGE ( 'NONE', *, *, #9883, .T. ) ;
#24096 = ORIENTED_EDGE ( 'NONE', *, *, #32928, .F. ) ;
#24097 = CARTESIAN_POINT ( 'NONE',  ( 0.1726814644796534071, -0.5193392427952403523, 0.1436262120076541027 ) ) ;
#24098 = ORIENTED_EDGE ( 'NONE', *, *, #19209, .F. ) ;
#24099 = APPLIED_APPROVAL_ASSIGNMENT ( #1494, ( #20163 ) ) ;
#24100 = EDGE_CURVE ( 'NONE', #35807, #11394, #24484, .T. ) ;
#24101 = CARTESIAN_POINT ( 'NONE',  ( -0.05464101615137787610, -2.551729310907437043, -0.4286726180052709001 ) ) ;
#24103 = ORIENTED_EDGE ( 'NONE', *, *, #4125, .F. ) ;
#24102 = CARTESIAN_POINT ( 'NONE',  ( -0.1089540792635167732, -0.4972110540767095688, 0.1150843967103700460 ) ) ;
#24105 = ORIENTED_EDGE ( 'NONE', *, *, #22873, .T. ) ;
#24104 = CARTESIAN_POINT ( 'NONE',  ( 0.009274569113454507810, -0.5902431952254217906, 0.02081147810894002498 ) ) ;
#24106 = ORIENTED_EDGE ( 'NONE', *, *, #4932, .F. ) ;
#24107 = CARTESIAN_POINT ( 'NONE',  ( 0.2859601836109825213, -0.8602919011690969286, 0.7882872347711364913 ) ) ;
#24108 = ORIENTED_EDGE ( 'NONE', *, *, #16498, .T. ) ;
#24109 = EDGE_CURVE ( 'NONE', #10925, #38396, #18390, .T. ) ;
#24110 = CARTESIAN_POINT ( 'NONE',  ( 0.2658579063097570860, -1.675104683681777340, 0.5666873703055449463 ) ) ;
#24112 = CARTESIAN_POINT ( 'NONE',  ( 0.4634203168357881597, -1.610090559957644274, -0.3776084174194705989 ) ) ;
#24111 = CARTESIAN_POINT ( 'NONE',  ( -0.2399999999999999079, -4.289222312108804225, -0.5708809693675255259 ) ) ;
#24113 = CARTESIAN_POINT ( 'NONE',  ( -0.2399999999999999079, -3.791721498889941255, -0.2726869407194119077 ) ) ;
#24114 = EDGE_CURVE ( 'NONE', #32978, #29236, #9446, .T. ) ;
#24115 = PERSON_AND_ORGANIZATION_ROLE ( 'classification_officer' ) ;
#24116 = LINE ( 'NONE', #17516, #25079 ) ;
#24118 = ORIENTED_EDGE ( 'NONE', *, *, #32849, .F. ) ;
#24117 = VERTEX_POINT ( 'NONE', #242 ) ;
#24119 = EDGE_CURVE ( 'NONE', #30207, #3229, #20853, .T. ) ;
#24120 = CARTESIAN_POINT ( 'NONE',  ( 0.01133266107010722987, -0.9445109682311131349, 0.1117785243345983531 ) ) ;
#24121 = DIRECTION ( 'NONE',  ( -7.771561172376107616E-16, 7.170354002788761615E-17, -1.000000000000000000 ) ) ;
#24122 = CARTESIAN_POINT ( 'NONE',  ( 0.09236582558789477315, -0.5663732494358152403, 0.2468274383348227075 ) ) ;
#24123 = ADVANCED_FACE ( 'NONE', ( #38231 ), #17748, .T. ) ;
#24124 = CARTESIAN_POINT ( 'NONE',  ( 0.1874263242844142752, -0.6916738960414681170, 0.04030299999698908758 ) ) ;
#24125 = DIRECTION ( 'NONE',  ( 1.000000000000000000, 6.779273404243070203E-32, 4.314083075427408311E-32 ) ) ;
#24126 = DIRECTION ( 'NONE',  ( 0.000000000000000000, -0.5877852522924906786, 0.8090169943749346837 ) ) ;
#24127 = CARTESIAN_POINT ( 'NONE',  ( 0.01220502636281931008, -0.4284498256520046788, 0.1513327638351227855 ) ) ;
#24128 = CARTESIAN_POINT ( 'NONE',  ( 0.3869965781225513934, -1.721508965229717969, 0.4224448655611768855 ) ) ;
#24129 = VECTOR ( 'NONE', #9741, 39.37007874015748854 ) ;
#24130 = CARTESIAN_POINT ( 'NONE',  ( 0.3965913301904470112, -1.111811593118468666, 0.6217369508112339238 ) ) ;
#24131 = CARTESIAN_POINT ( 'NONE',  ( -0.05464101615137762630, -2.058305985490972212, -0.5970033804171128722 ) ) ;
#24132 = CARTESIAN_POINT ( 'NONE',  ( 0.3056347003372518745, -1.768333716703696323, 0.5707417262808793801 ) ) ;
#24133 = CARTESIAN_POINT ( 'NONE',  ( 0.4495844847086868379, -1.113559791644742836, 0.5920747722683810110 ) ) ;
#24134 = CARTESIAN_POINT ( 'NONE',  ( -2.070859481142756309, -2.678208067297373152, 0.4182417262808778013 ) ) ;
#24135 = CARTESIAN_POINT ( 'NONE',  ( 0.1992679972018663592, -1.286890268402110182, -0.7430135000225476238 ) ) ;
#24136 = CARTESIAN_POINT ( 'NONE',  ( 0.003124719664520466192, -0.5686731593868933343, 0.09441483597926585147 ) ) ;
#24137 = CARTESIAN_POINT ( 'NONE',  ( 0.4813782568983027699, -1.076368431653871971, 0.6093178202591913450 ) ) ;
#24138 = CARTESIAN_POINT ( 'NONE',  ( -0.002132486385545492077, -0.8570572293951210785, 0.2363897508679551895 ) ) ;
#24139 = APPROVAL_ROLE ( '' ) ;
#24140 = CARTESIAN_POINT ( 'NONE',  ( 0.4199384557880279645, -0.9749410087210258480, 0.8268343460595501959 ) ) ;
#24141 = EDGE_CURVE ( 'NONE', #356, #38533, #28906, .T. ) ;
#24142 = CARTESIAN_POINT ( 'NONE',  ( -0.05464101615137770263, -2.177105168660885326, -0.2518349584362399862 ) ) ;
#24143 = ADVANCED_FACE ( 'NONE', ( #10059 ), #23030, .T. ) ;
#24144 = CARTESIAN_POINT ( 'NONE',  ( 0.05076679145661983777, -0.04886774829954456528, -0.4712599967968629233 ) ) ;
#24145 = DIRECTION ( 'NONE',  ( -8.881784197001246407E-16, 2.361472542561082612E-16, -1.000000000000000000 ) ) ;
#24146 = EDGE_LOOP ( 'NONE', ( #36202, #8346, #38288, #39927 ) ) ;
#24147 = CARTESIAN_POINT ( 'NONE',  ( 0.4540174329365269656, -1.143689243732040728, -0.6344893339101922436 ) ) ;
#24148 = CARTESIAN_POINT ( 'NONE',  ( 0.03323571768382589664, -0.7628981867746865708, 0.6419652344973219016 ) ) ;
#24149 = CARTESIAN_POINT ( 'NONE',  ( 0.1286531880915040282, -0.5504795770112219655, 0.1533591383774981221 ) ) ;
#24150 = CARTESIAN_POINT ( 'NONE',  ( 0.3797463714376327348, -1.760601621700183639, -0.4487751144967741523 ) ) ;
#24152 = ORIENTED_EDGE ( 'NONE', *, *, #5851, .F. ) ;
#24151 = CARTESIAN_POINT ( 'NONE',  ( -0.08000000000000000167, -2.122347498858831116, -0.8313396097929490747 ) ) ;
#24153 = CARTESIAN_POINT ( 'NONE',  ( 0.1918124086860224231, -0.5891232155910660628, 0.2119633080407007653 ) ) ;
#24155 = ORIENTED_EDGE ( 'NONE', *, *, #39929, .F. ) ;
#24154 = ORIENTED_EDGE ( 'NONE', *, *, #18726, .T. ) ;
#24156 = CARTESIAN_POINT ( 'NONE',  ( 0.09591312667570967010, -1.362172318102457202, -0.6980176222590579460 ) ) ;
#24157 = ORIENTED_EDGE ( 'NONE', *, *, #3500, .F. ) ;
#24158 = CARTESIAN_POINT ( 'NONE',  ( 0.3591498995103418190, -1.737620376665806932, -0.5147966178037273188 ) ) ;
#24159 = DIRECTION ( 'NONE',  ( 1.000000000000000000, 0.000000000000000000, 0.000000000000000000 ) ) ;
#24160 = PERSON_AND_ORGANIZATION ( #38252, #34566 ) ;
#24161 = FACE_OUTER_BOUND ( 'NONE', #2030, .T. ) ;
#24162 = ORIENTED_EDGE ( 'NONE', *, *, #24842, .F. ) ;
#24163 = CARTESIAN_POINT ( 'NONE',  ( 0.1619021036549118109, -1.239954387664122804, 0.6006692075211629289 ) ) ;
#24164 = CARTESIAN_POINT ( 'NONE',  ( 0.1868433879157239408, -0.8567470366939088366, 0.6079207818232758020 ) ) ;
#24165 = CARTESIAN_POINT ( 'NONE',  ( 0.3076776373462946079, -1.692203703971726148, 0.8683076824790618709 ) ) ;
#24166 = CARTESIAN_POINT ( 'NONE',  ( 0.09958715870559087247, -0.5710702051975550253, 0.2566525979842094185 ) ) ;
#24168 = CARTESIAN_POINT ( 'NONE',  ( -0.001716626588588560445, -0.8384702095208486083, 0.07132058285942260989 ) ) ;
#24167 = CARTESIAN_POINT ( 'NONE',  ( 0.3224073211681580675, -1.764214325044133780, 0.5172595626481488740 ) ) ;
#24169 = CARTESIAN_POINT ( 'NONE',  ( 6.320982786526573478E-21, -0.9481888444201335142, 0.1628301291833881004 ) ) ;
#24170 = EDGE_LOOP ( 'NONE', ( #18150, #28217, #13207, #25323 ) ) ;
#24171 = VERTEX_POINT ( 'NONE', #38444 ) ;
#24172 = CARTESIAN_POINT ( 'NONE',  ( 0.3768783096114195486, -1.720370743462858343, 0.4222122349756301518 ) ) ;
#24173 = CARTESIAN_POINT ( 'NONE',  ( 0.3074793524532691835, -0.8298883473507410180, 0.6448015414277138424 ) ) ;
#24174 = DIRECTION ( 'NONE',  ( -0.1871397384865033653, -0.9823333030490227769, 9.555504051854013858E-17 ) ) ;
#24175 = CARTESIAN_POINT ( 'NONE',  ( 0.05082303569918527469, -0.4330427793496154365, 0.1918498709088723442 ) ) ;
#24176 = CARTESIAN_POINT ( 'NONE',  ( 0.06936654275873489761, -1.327133429011184917, 0.5458395137742713121 ) ) ;
#24177 = CARTESIAN_POINT ( 'NONE',  ( 0.4197981397002149007, -1.708404881074925274, -0.5025783929700992081 ) ) ;
#24178 = CARTESIAN_POINT ( 'NONE',  ( 0.3144318060873547704, -1.185957278504782941, 0.4815581988605170949 ) ) ;
#24179 = CARTESIAN_POINT ( 'NONE',  ( 0.1880247778135462344, -0.6881053353252821747, 0.1842137475136224611 ) ) ;
#24180 = PERSON_AND_ORGANIZATION ( #28500, #32463 ) ;
#24181 = DIRECTION ( 'NONE',  ( 0.9480245940703961871, 0.3181970600707375030, 0.000000000000000000 ) ) ;
#24182 = CARTESIAN_POINT ( 'NONE',  ( 0.06980746140711582837, 0.000000000000000000, 0.000000000000000000 ) ) ;
#24183 = FACE_OUTER_BOUND ( 'NONE', #8345, .T. ) ;
#24184 = DIRECTION ( 'NONE',  ( 0.000000000000000000, 0.000000000000000000, -1.000000000000000000 ) ) ;
#24185 = CIRCLE ( 'NONE', #23521, 0.01500000000000005496 ) ;
#24186 = CARTESIAN_POINT ( 'NONE',  ( 0.6064900336555086868, -1.480007000944690398, 0.5584290337526855996 ) ) ;
#24187 = EDGE_LOOP ( 'NONE', ( #25306, #13565 ) ) ;
#24188 = CARTESIAN_POINT ( 'NONE',  ( 0.1734973056165642902, -1.209394307038482719, -0.5155029497116575543 ) ) ;
#24189 = DIRECTION ( 'NONE',  ( -1.000000000000000000, 0.000000000000000000, 0.000000000000000000 ) ) ;
#24190 = B_SPLINE_CURVE_WITH_KNOTS ( 'NONE', 3,
 ( #25052, #34513, #6323, #32031, #6516, #25261, #25471, #9814, #38199, #13310 ),
 .UNSPECIFIED., .F., .F.,
 ( 4, 2, 2, 2, 4 ),
 ( 0.000000000000000000, 0.0002543125689965293913, 0.0005086251379930587825, 0.0007629377069895881738, 0.001017250275986117565 ),
 .UNSPECIFIED. ) ;
#24191 = CARTESIAN_POINT ( 'NONE',  ( -0.04575334816097852142, -0.06504672743687492376, -0.4827724779829238311 ) ) ;
#24192 = CARTESIAN_POINT ( 'NONE',  ( 0.2234517780780992391, -1.345597857905709294, 0.6134231468698841949 ) ) ;
#24193 = ORIENTED_EDGE ( 'NONE', *, *, #36156, .T. ) ;
#24194 = CARTESIAN_POINT ( 'NONE',  ( -0.04154009738085499837, 0.2622554993748598129, 0.3904256972020302419 ) ) ;
#24195 = CARTESIAN_POINT ( 'NONE',  ( 0.03674078017396018025, -0.04075419261117101122, 0.4790519037776401201 ) ) ;
#24196 = CARTESIAN_POINT ( 'NONE',  ( 0.02872242845529722130, -0.4768947642620330329, -0.2371557650702024733 ) ) ;
#24197 = CARTESIAN_POINT ( 'NONE',  ( -0.1969433606228599420, 0.5138636982738220560, 0.3032895567580801144 ) ) ;
#24198 = CARTESIAN_POINT ( 'NONE',  ( 0.4351441434883658310, -1.191296924415893965, 0.6803100719843556687 ) ) ;
#24200 = DIRECTION ( 'NONE',  ( -0.3468893892380666699, 0.2594111197898833487, 0.9013177145509789767 ) ) ;
#24199 = CARTESIAN_POINT ( 'NONE',  ( 0.03303708955568378236, 0.5155567402493611562, 0.07470075307486020999 ) ) ;
#24201 = DIRECTION ( 'NONE',  ( 2.465190328815661892E-32, 1.000000000000000000, 6.656013887802287108E-31 ) ) ;
#24202 = EDGE_LOOP ( 'NONE', ( #9710, #10514, #2429, #23083 ) ) ;
#24203 = ORIENTED_EDGE ( 'NONE', *, *, #20539, .F. ) ;
#24204 = CARTESIAN_POINT ( 'NONE',  ( 0.07443973040452947498, -1.324188178367487145, 0.5273133236568789961 ) ) ;
#24205 = ORIENTED_EDGE ( 'NONE', *, *, #21435, .F. ) ;
#24206 = CARTESIAN_POINT ( 'NONE',  ( 0.1853096727063575921, -0.4547550531002670371, -0.03797464539687132878 ) ) ;
#24207 = CARTESIAN_POINT ( 'NONE',  ( 0.3152971339881030510, -1.290423043535891656, 0.8808430741779670337 ) ) ;
#24209 = CARTESIAN_POINT ( 'NONE',  ( 0.2003689620726051279, -0.7510051162810029712, 0.3312793566268386614 ) ) ;
#24208 = CARTESIAN_POINT ( 'NONE',  ( -0.03309060444528710843, -0.5154120966056451314, 0.07470591001490139993 ) ) ;
#24210 = SPHERICAL_SURFACE ( 'NONE', #23780, 0.01499999999999999944 ) ;
#24211 = ORIENTED_EDGE ( 'NONE', *, *, #34137, .T. ) ;
#24212 = ORIENTED_EDGE ( 'NONE', *, *, #9486, .F. ) ;
#24213 = CARTESIAN_POINT ( 'NONE',  ( 0.3926986855850684854, -1.778818435110647522, -0.3125573702649511731 ) ) ;
#24214 = CARTESIAN_POINT ( 'NONE',  ( 0.5818144595221569348, -1.494326653636363522, 0.6059908575948350640 ) ) ;
#24215 = AXIS2_PLACEMENT_3D ( 'NONE', #6719, #19293, #611 ) ;
#24216 = CARTESIAN_POINT ( 'NONE',  ( 0.3939841861132012957, -1.751817660254116893, -0.4710238052775803652 ) ) ;
#24217 = FACE_OUTER_BOUND ( 'NONE', #33519, .T. ) ;
#24218 = DIRECTION ( 'NONE',  ( -2.465190328815661892E-32, -1.000000000000000000, -6.656013887802287108E-31 ) ) ;
#24219 = DIRECTION ( 'NONE',  ( -0.000000000000000000, -0.9450610163799286756, -0.3268939817722809615 ) ) ;
#24220 = CARTESIAN_POINT ( 'NONE',  ( -0.1532354427637372674, 0.4747053032734181444, 0.3600204025348321402 ) ) ;
#24221 = CARTESIAN_POINT ( 'NONE',  ( 0.1499999999999996336, -0.07651041855119578017, -0.5222379212568201146 ) ) ;
#24222 = CARTESIAN_POINT ( 'NONE',  ( 0.2366026829857577063, -0.6283501033379368383, 0.5457308484972661633 ) ) ;
#24223 = CARTESIAN_POINT ( 'NONE',  ( 0.08146015332400657893, -1.318321297778866308, 0.4704503523288177669 ) ) ;
#24224 = CARTESIAN_POINT ( 'NONE',  ( 0.6213544394143908356, -1.618324384172695529, -0.5525161381485133028 ) ) ;
#24225 = CARTESIAN_POINT ( 'NONE',  ( 0.1511697332786464953, -1.326440298964499886, -0.7191902533801515229 ) ) ;
#24226 = CARTESIAN_POINT ( 'NONE',  ( 0.6340757229130811190, -1.590406591614232479, 0.6099564950747226044 ) ) ;
#24227 = PLANE ( 'NONE',  #24533 ) ;
#24228 = EDGE_CURVE ( 'NONE', #22322, #28969, #21693, .T. ) ;
#24229 = VERTEX_POINT ( 'NONE', #16249 ) ;
#24230 = APPLIED_DATE_AND_TIME_ASSIGNMENT ( #9099, #36483, ( #25389 ) ) ;
#24231 = CARTESIAN_POINT ( 'NONE',  ( 0.006340579314978117206, -0.5092170189304694450, 0.4201425565785884553 ) ) ;
#24232 = CARTESIAN_POINT ( 'NONE',  ( 0.3630296588320852114, -1.750092887594260960, -0.5972373629894556224 ) ) ;
#24233 = CARTESIAN_POINT ( 'NONE',  ( 0.4212767629397370373, -1.592273061960515435, -0.6162690127139324181 ) ) ;
#24234 = CARTESIAN_POINT ( 'NONE',  ( 0.3532546603346390923, -1.752899160574764137, 0.5887449090255344464 ) ) ;
#24235 = ORIENTED_EDGE ( 'NONE', *, *, #18962, .T. ) ;
#24236 = CARTESIAN_POINT ( 'NONE',  ( 0.05999999999999990757, 0.4783370154475735103, 0.2940679337375869395 ) ) ;
#24237 = CARTESIAN_POINT ( 'NONE',  ( 0.3523703943677440331, -1.135285113435899884, 0.5996270292805977453 ) ) ;
#24238 = CARTESIAN_POINT ( 'NONE',  ( -0.01548846960707524721, 0.000000000000000000, 0.000000000000000000 ) ) ;
#24239 = CARTESIAN_POINT ( 'NONE',  ( 0.6400160853294423191, -1.459529829645036081, -0.3976988710621562895 ) ) ;
#24240 = CARTESIAN_POINT ( 'NONE',  ( 0.3321123081999855509, -1.047335542731505420, 0.7624713745059377157 ) ) ;
#24242 = ORIENTED_EDGE ( 'NONE', *, *, #34392, .T. ) ;
#24241 = LINE ( 'NONE', #2829, #40306 ) ;
#24243 = CARTESIAN_POINT ( 'NONE',  ( 0.5030539720840632167, -1.104010818905506675, 0.6157662270679344907 ) ) ;
#24244 = ORIENTED_EDGE ( 'NONE', *, *, #4254, .T. ) ;
#24245 = CARTESIAN_POINT ( 'NONE',  ( 0.1036077641498115154, -1.348975793691512992, -0.3541914004549143180 ) ) ;
#24246 = ORIENTED_EDGE ( 'NONE', *, *, #19073, .T. ) ;
#24247 = DIRECTION ( 'NONE',  ( 0.000000000000000000, 0.000000000000000000, -1.000000000000000000 ) ) ;
#24248 = ORIENTED_EDGE ( 'NONE', *, *, #40139, .F. ) ;
#24249 = EDGE_CURVE ( 'NONE', #9331, #22862, #12957, .T. ) ;
#24250 = CARTESIAN_POINT ( 'NONE',  ( 0.2272720996045521635, -1.257744579346037561, 0.9080304507863062868 ) ) ;
#24252 = CARTESIAN_POINT ( 'NONE',  ( 0.1762911760445602105, -0.5715213023984071494, -0.05307465194668001957 ) ) ;
#24251 = CARTESIAN_POINT ( 'NONE',  ( 0.6611561708455119257, -1.539609889559191869, 0.4316073648859315437 ) ) ;
#24253 = FACE_OUTER_BOUND ( 'NONE', #16863, .T. ) ;
#24254 = ORIENTED_EDGE ( 'NONE', *, *, #22868, .T. ) ;
#24255 = CARTESIAN_POINT ( 'NONE',  ( 0.4591084281630142261, -1.062138763103065875, 0.7175457429786104013 ) ) ;
#24256 = EDGE_CURVE ( 'NONE', #8281, #13526, #713, .T. ) ;
#24257 = VERTEX_POINT ( 'NONE', #34949 ) ;
#24258 = CARTESIAN_POINT ( 'NONE',  ( 0.06980746140711582837, -3.685538980774209949E-17, -0.1750000000000000167 ) ) ;
#24259 = ADVANCED_FACE ( 'NONE', ( #37843 ), #9657, .T. ) ;
#24260 = DIRECTION ( 'NONE',  ( 1.000000000000000000, 0.000000000000000000, 0.000000000000000000 ) ) ;
#24261 = CARTESIAN_POINT ( 'NONE',  ( 0.07907905168991602451, -0.8327024128097892941, 0.1796145744779967246 ) ) ;
#24262 = DIRECTION ( 'NONE',  ( 0.8660512985181135770, 0.4999551463232368431, 0.000000000000000000 ) ) ;
#24263 = EDGE_CURVE ( 'NONE', #1197, #29289, #31873, .T. ) ;
#24264 = CARTESIAN_POINT ( 'NONE',  ( 0.5010929404620397820, -1.674525211673266956, -0.6058220862217358338 ) ) ;
#24265 = ADVANCED_FACE ( 'NONE', ( #28588 ), #4063, .F. ) ;
#24266 = EDGE_CURVE ( 'NONE', #9810, #1239, #5908, .T. ) ;
#24267 = B_SPLINE_CURVE_WITH_KNOTS ( 'NONE', 1,
 ( #13026, #5814, #25163, #3152 ),
 .UNSPECIFIED., .F., .F.,
 ( 2, 1, 1, 2 ),
 ( -0.0007619999999999863211, 2.168404344971008868E-18, 0.0007619999999999993315, 0.001523999999999991074 ),
 .UNSPECIFIED. ) ;
#24268 = DIRECTION ( 'NONE',  ( -1.188678714063518227E-15, 1.000000000000000000, 3.263080277421930985E-16 ) ) ;
#24269 = CARTESIAN_POINT ( 'NONE',  ( -0.02000000000000000042, -2.297142231534299306, -0.5217974784625020179 ) ) ;
#24270 = CARTESIAN_POINT ( 'NONE',  ( 0.03309057659885145108, 0.4608882367397874602, 0.2425133248663937369 ) ) ;
#24271 = CARTESIAN_POINT ( 'NONE',  ( 0.4258872143332720350, -1.124793373273393682, 0.5082973339379032174 ) ) ;
#24272 = CARTESIAN_POINT ( 'NONE',  ( 0.05992090360963518020, -1.332693131100006312, 0.5739722883257112329 ) ) ;
#24273 = PERSON_AND_ORGANIZATION_ROLE ( 'design_owner' ) ;
#24274 = CARTESIAN_POINT ( 'NONE',  ( 0.4852819058807865682, -1.130531678747876967, 0.4902071956013302478 ) ) ;
#24275 = CARTESIAN_POINT ( 'NONE',  ( 0.4958658331358156701, -1.219703574955436576, 0.6057417262809811076 ) ) ;
#24276 = APPLICATION_CONTEXT ( 'configuration controlled 3d designs of mechanical parts and assemblies' ) ;
#24277 = CARTESIAN_POINT ( 'NONE',  ( 0.5838486772476066955, -1.549002738031555637, -0.6085822719328981556 ) ) ;
#24278 =( BOUNDED_SURFACE ( )  B_SPLINE_SURFACE ( 3, 2, ( 
 ( #24696, #37228, #34130 ),
 ( #28174, #38228, #31461 ),
 ( #29182, #3268, #19121 ),
 ( #31661, #16245, #3478 ) ),
 .UNSPECIFIED., .F., .F., .F. ) 
 B_SPLINE_SURFACE_WITH_KNOTS ( ( 4, 4 ),
 ( 3, 3 ),
 ( -7.975391180803370617E-16, 0.0006271655702608574731 ),
 ( 0.000000000000000000, 1.000000000000000000 ),
 .UNSPECIFIED. ) 
 GEOMETRIC_REPRESENTATION_ITEM ( )  RATIONAL_B_SPLINE_SURFACE ( (
 ( 1.000000000000000000, 0.7064740011966007538, 1.000000000000000000),
 ( 1.000000000000000000, 0.7219955957196710905, 1.000000000000000000),
 ( 1.000000000000000000, 0.7376221875044689513, 1.000000000000000000),
 ( 1.000000000000000000, 0.7525568848367699681, 1.000000000000000000) ) ) 
 REPRESENTATION_ITEM ( '' )  SURFACE ( )  );
#24279 = ADVANCED_FACE ( 'NONE', ( #30001 ), #23450, .F. ) ;
#24280 = CARTESIAN_POINT ( 'NONE',  ( 0.4428525721104821233, -1.108557561101682909, -0.3966740480326817475 ) ) ;
#24281 = DIRECTION ( 'NONE',  ( 0.000000000000000000, 0.000000000000000000, -1.000000000000000000 ) ) ;
#24282 = CARTESIAN_POINT ( 'NONE',  ( 0.2747286271120374934, -1.554764607944815635, -0.7171264253415187140 ) ) ;
#24283 = CARTESIAN_POINT ( 'NONE',  ( 0.3811173169455821519, -1.749731223830197191, -0.5852530064128164122 ) ) ;
#24284 = ORIENTED_EDGE ( 'NONE', *, *, #2167, .F. ) ;
#24285 = VERTEX_POINT ( 'NONE', #32862 ) ;
#24286 = DIRECTION ( 'NONE',  ( -0.01455087615875037474, -0.9998941303973200023, -4.739223851275271008E-17 ) ) ;
#24287 = ORIENTED_EDGE ( 'NONE', *, *, #7196, .F. ) ;
#24288 = CARTESIAN_POINT ( 'NONE',  ( 0.4498803379890206067, -1.659323614875797936, -0.3947173143921381411 ) ) ;
#24290 = EDGE_LOOP ( 'NONE', ( #9866, #10288, #6518, #24804 ) ) ;
#24289 = CARTESIAN_POINT ( 'NONE',  ( -0.3000000000000000999, -2.139295658456680904, -0.2024034539465678073 ) ) ;
#24292 = ORIENTED_EDGE ( 'NONE', *, *, #23983, .F. ) ;
#24291 = DIRECTION ( 'NONE',  ( -1.000000000000000000, -0.000000000000000000, -0.000000000000000000 ) ) ;
#24293 = ORIENTED_EDGE ( 'NONE', *, *, #34569, .T. ) ;
#24294 = CARTESIAN_POINT ( 'NONE',  ( -0.2300000000000000100, 0.5182417262804744906, 0.3749999999999995559 ) ) ;
#24295 = CARTESIAN_POINT ( 'NONE',  ( 0.2661946161772972275, -1.675245939826407016, 0.5712008051485940596 ) ) ;
#24297 = CARTESIAN_POINT ( 'NONE',  ( 0.1293833808128240226, -1.251700972679722357, 0.6057482417128505769 ) ) ;
#24296 = CARTESIAN_POINT ( 'NONE',  ( 1.900334097155061703E-16, 0.3059742766594581997, 0.06173076923076874917 ) ) ;
#24298 = CARTESIAN_POINT ( 'NONE',  ( 0.2469141422421070875, -1.581573626495411444, -0.3511777555542848206 ) ) ;
#24299 = DATE_AND_TIME ( #33745, #27384 ) ;
#24300 = CARTESIAN_POINT ( 'NONE',  ( 0.000000000000000000, 0.08000000000000023759, 0.000000000000000000 ) ) ;
#24302 = ORIENTED_EDGE ( 'NONE', *, *, #36897, .T. ) ;
#24301 = VERTEX_POINT ( 'NONE', #20541 ) ;
#24303 = CARTESIAN_POINT ( 'NONE',  ( 0.01159594543348162025, -0.8166607006614792219, -0.07868870078605369467 ) ) ;
#24304 = CARTESIAN_POINT ( 'NONE',  ( -0.05543910610524961646, -0.4446004295725691224, 0.1230574251923865076 ) ) ;
#24305 = EDGE_CURVE ( 'NONE', #2027, #18407, #28261, .T. ) ;
#24306 = CARTESIAN_POINT ( 'NONE',  ( 0.2950454914726564071, -0.9974602440063756736, 0.7344975353665614826 ) ) ;
#24307 = CARTESIAN_POINT ( 'NONE',  ( 0.1859701558446418823, -0.7915647177415402469, 0.06398500588167709002 ) ) ;
#24308 = FACE_BOUND ( 'NONE', #25098, .T. ) ;
#24309 = DIRECTION ( 'NONE',  ( 0.8660512985181133550, 0.4999551463232371207, 0.000000000000000000 ) ) ;
#24310 = ADVANCED_FACE ( 'NONE', ( #29584 ), #8711, .T. ) ;
#24311 = CARTESIAN_POINT ( 'NONE',  ( 0.3907225962692674193, -1.711934981260601063, -0.4322588514322361908 ) ) ;
#24312 = CARTESIAN_POINT ( 'NONE',  ( -0.2399999999999999079, -3.433273040916029029, -1.270777394095183199 ) ) ;
#24313 = ADVANCED_FACE ( 'NONE', ( #37183 ), #26434, .F. ) ;
#24314 = DIRECTION ( 'NONE',  ( 9.244463733058726621E-33, 0.4685245517976878160, 0.8834504764630419782 ) ) ;
#24315 = CARTESIAN_POINT ( 'NONE',  ( 0.4787764723021453728, -1.660223331282874915, 0.4687417262808790119 ) ) ;
#24316 = CARTESIAN_POINT ( 'NONE',  ( -1.501945623848432731E-05, -0.9404952636685606215, 0.08221629722440988719 ) ) ;
#24317 = CARTESIAN_POINT ( 'NONE',  ( 0.3907430023610570791, -1.657027545734215179, -0.4094362587932089403 ) ) ;
#24318 = DIRECTION ( 'NONE',  ( -1.232595164407830946E-32, 1.110223024625156540E-16, 0.9999999999999998890 ) ) ;
#24319 = CARTESIAN_POINT ( 'NONE',  ( 0.03174060074381968716, -0.2437182008228601648, 0.4645020220639594077 ) ) ;
#24320 = CARTESIAN_POINT ( 'NONE',  ( 0.01707166242847063184, -0.6102210326195973700, 0.5232503585198154950 ) ) ;
#24321 = CARTESIAN_POINT ( 'NONE',  ( 0.05627171146895854764, -1.105186018705181406, 0.7448477350381816908 ) ) ;
#24322 = PERSON_AND_ORGANIZATION_ROLE ( 'classification_officer' ) ;
#24323 = CARTESIAN_POINT ( 'NONE',  ( 0.7205914100055046401, -1.471989004879187490, 0.6461535000039996257 ) ) ;
#24324 = CIRCLE ( 'NONE', #3951, 0.01499999999999995434 ) ;
#24325 = EDGE_CURVE ( 'NONE', #9243, #8729, #16434, .T. ) ;
#24326 = EDGE_CURVE ( 'NONE', #34358, #34037, #3946, .T. ) ;
#24327 = CARTESIAN_POINT ( 'NONE',  ( 0.04855986989123495939, 0.05683501216513824755, -0.1249999999999999029 ) ) ;
#24328 = CARTESIAN_POINT ( 'NONE',  ( 0.04047170147976490023, -0.06272069502581187339, -0.4973236590858508555 ) ) ;
#24329 = CARTESIAN_POINT ( 'NONE',  ( -0.2399999999999999079, -4.292451985131092940, -0.8428112192407016812 ) ) ;
#24330 = VERTEX_POINT ( 'NONE', #27931 ) ;
#24331 = FACE_OUTER_BOUND ( 'NONE', #20597, .T. ) ;
#24332 = CARTESIAN_POINT ( 'NONE',  ( 0.08536974246100553776, -0.9712496366881051557, 0.8111207091837429051 ) ) ;
#24333 = CARTESIAN_POINT ( 'NONE',  ( 0.4692603364931002274, -1.311301443745613193, 0.8202886701068771158 ) ) ;
#24335 = ORIENTED_EDGE ( 'NONE', *, *, #5096, .F. ) ;
#24334 = CARTESIAN_POINT ( 'NONE',  ( 0.3984413745674345031, -1.753413336483850893, -0.5068292923117084792 ) ) ;
#24336 = CARTESIAN_POINT ( 'NONE',  ( 0.3050116026255210722, -0.8112037691066587008, 0.6500339927034136656 ) ) ;
#24338 = EDGE_LOOP ( 'NONE', ( #2945, #6848, #6556, #937 ) ) ;
#24337 = ORIENTED_EDGE ( 'NONE', *, *, #8501, .F. ) ;
#24339 = CARTESIAN_POINT ( 'NONE',  ( 0.1978587402095111636, -0.5849795632145003976, 0.3178455878192510409 ) ) ;
#24340 = FACE_OUTER_BOUND ( 'NONE', #35289, .T. ) ;
#24341 = DIRECTION ( 'NONE',  ( 0.000000000000000000, 0.000000000000000000, -1.000000000000000000 ) ) ;
#24342 = DATE_AND_TIME ( #24554, #6299 ) ;
#24343 = AXIS2_PLACEMENT_3D ( 'NONE', #38036, #13134, #22226 ) ;
#24344 = CARTESIAN_POINT ( 'NONE',  ( -0.04762200653274207413, 0.4434980416368405898, -0.1892582844414349152 ) ) ;
#24345 = ORIENTED_EDGE ( 'NONE', *, *, #6399, .T. ) ;
#24346 = CARTESIAN_POINT ( 'NONE',  ( 0.1570735404638902155, -0.8185203973244239428, 0.5474549588355609453 ) ) ;
#24347 = DIRECTION ( 'NONE',  ( 1.000000000000000000, 1.799754070459507683E-12, -1.860523581402830585E-12 ) ) ;
#24348 = CIRCLE ( 'NONE', #33512, 0.01500000000000001159 ) ;
#24349 = CARTESIAN_POINT ( 'NONE',  ( 0.4975257062221719595, -1.542520066884107477, 0.5745007069453309523 ) ) ;
#24351 = CARTESIAN_POINT ( 'NONE',  ( -0.001003582044002233756, -0.7901068500879731005, 0.01239078819350922581 ) ) ;
#24350 = CARTESIAN_POINT ( 'NONE',  ( 0.3228300096166880628, -1.762500210627791830, 0.5312294313579276617 ) ) ;
#24352 = CARTESIAN_POINT ( 'NONE',  ( 0.04506684102745490278, -1.071221704980362732, 0.6225836480969521025 ) ) ;
#24353 = ORIENTED_EDGE ( 'NONE', *, *, #27363, .T. ) ;
#24354 = ORIENTED_EDGE ( 'NONE', *, *, #26532, .F. ) ;
#24355 = ADVANCED_FACE ( 'NONE', ( #2432 ), #14970, .T. ) ;
#24356 = DIRECTION ( 'NONE',  ( 0.000000000000000000, 0.9510565162951502005, -0.3090169943749580539 ) ) ;
#24357 = CARTESIAN_POINT ( 'NONE',  ( 0.3490285838404457164, -0.8930994557897173891, 0.6976986907528974768 ) ) ;
#24358 = CARTESIAN_POINT ( 'NONE',  ( -0.01548846960707545191, -0.5198120922912051745, -0.07362328916749329155 ) ) ;
#24359 = DIRECTION ( 'NONE',  ( -1.000000000000000000, -0.000000000000000000, -0.000000000000000000 ) ) ;
#24360 = DIRECTION ( 'NONE',  ( -1.000000000000000000, -0.000000000000000000, -0.000000000000000000 ) ) ;
#24361 = CARTESIAN_POINT ( 'NONE',  ( 0.2649651584399684845, -1.675931921620917420, 0.5387030096079383767 ) ) ;
#24362 = CARTESIAN_POINT ( 'NONE',  ( 0.3599681117411700493, -1.738096220096565725, -0.5053368274672028759 ) ) ;
#24363 = CARTESIAN_POINT ( 'NONE',  ( 0.5392338747517343434, -1.163405467613477295, 0.6464276897500325081 ) ) ;
#24364 = PERSON_AND_ORGANIZATION ( #28500, #32463 ) ;
#24365 = CYLINDRICAL_SURFACE ( 'NONE', #7629, 0.1033070866141734129 ) ;
#24366 = ADVANCED_FACE ( 'NONE', ( #27523 ), #37454, .T. ) ;
#24367 = CIRCLE ( 'NONE', #38793, 0.1000000000000000194 ) ;
#24368 = CARTESIAN_POINT ( 'NONE',  ( 0.1991480113865250756, -2.054949600705706203, -0.6841806413415671972 ) ) ;
#24369 = EDGE_CURVE ( 'NONE', #35563, #17308, #19724, .T. ) ;
#24370 = CARTESIAN_POINT ( 'NONE',  ( 0.4154866155576192877, -1.204292224885589402, 0.6716659532497037954 ) ) ;
#24371 = CARTESIAN_POINT ( 'NONE',  ( 0.4428400309745523233, -1.146281092196613338, -0.3830631589809550541 ) ) ;
#24372 = EDGE_LOOP ( 'NONE', ( #37192, #39702, #20059, #23304 ) ) ;
#24373 = DIRECTION ( 'NONE',  ( 0.01455087615875041117, 0.9998941303973198913, 0.000000000000000000 ) ) ;
#24374 = AXIS2_PLACEMENT_3D ( 'NONE', #8477, #3131, #30496 ) ;
#24375 = VECTOR ( 'NONE', #205, 39.37007874015748143 ) ;
#24376 = CARTESIAN_POINT ( 'NONE',  ( 0.2554305435801562107, -0.9452134505148684918, 0.6994406939077150165 ) ) ;
#24377 = EDGE_LOOP ( 'NONE', ( #3876, #25887, #23387, #22025 ) ) ;
#24378 = CARTESIAN_POINT ( 'NONE',  ( -0.04285561529641568335, -0.07198636226547319716, -0.4895514295879473399 ) ) ;
#24379 = CARTESIAN_POINT ( 'NONE',  ( 0.008503815048827287337, -0.8451467311994965703, 0.1811066047224641762 ) ) ;
#24381 = ORIENTED_EDGE ( 'NONE', *, *, #2355, .T. ) ;
#24380 = ORIENTED_EDGE ( 'NONE', *, *, #5360, .T. ) ;
#24382 = CARTESIAN_POINT ( 'NONE',  ( 0.05999999999999990757, 0.5386841146467193919, -0.2575246450067292248 ) ) ;
#24383 = SHAPE_REPRESENTATION ( 'pulley bushing cover', ( #27819 ), #11399 ) ;
#24384 = DIRECTION ( 'NONE',  ( -1.000000000000000000, -2.280301054154495132E-31, 1.664003471950577689E-31 ) ) ;
#24385 = CARTESIAN_POINT ( 'NONE',  ( 0.7429241260303105499, -1.515741207197444762, 0.5682417262808782121 ) ) ;
#24386 = CARTESIAN_POINT ( 'NONE',  ( 0.1953882094510071277, -1.994676107002966381, -0.3200132981238684726 ) ) ;
#24387 = CARTESIAN_POINT ( 'NONE',  ( 0.3518875961510150585, -1.091088960822164555, 0.7123828146467774403 ) ) ;
#24389 = DIRECTION ( 'NONE',  ( -0.9378410757839554801, -0.1072489841977692648, -0.3300784330442382286 ) ) ;
#24388 = DIRECTION ( 'NONE',  ( 0.8660512985181133550, 0.4999551463232372872, 0.000000000000000000 ) ) ;
#24390 = CARTESIAN_POINT ( 'NONE',  ( -0.03309057659885163843, -0.3730661755626923370, -0.3633900220890627919 ) ) ;
#24391 = ORIENTED_EDGE ( 'NONE', *, *, #23024, .F. ) ;
#24392 = VERTEX_POINT ( 'NONE', #25243 ) ;
#24393 = CARTESIAN_POINT ( 'NONE',  ( 0.3999999999999787059, -2.183180860297921466, -0.5437760292030870968 ) ) ;
#24394 = ORIENTED_EDGE ( 'NONE', *, *, #28755, .F. ) ;
#24395 = CARTESIAN_POINT ( 'NONE',  ( 0.1832751269464030219, -0.7337134285967986669, 0.1015045423513593059 ) ) ;
#24396 = CARTESIAN_POINT ( 'NONE',  ( 0.4258307314927392007, -1.528964036469551369, 0.7696345003288364017 ) ) ;
#24398 = CARTESIAN_POINT ( 'NONE',  ( 0.05999999999999990757, -0.1944112117964420239, -0.1713095900442092034 ) ) ;
#24397 = CARTESIAN_POINT ( 'NONE',  ( -0.1163200376094536276, -0.5319009979872306726, 0.1426078552794942667 ) ) ;
#24399 = CARTESIAN_POINT ( 'NONE',  ( 0.3047823188150395324, -1.756856274844342147, 0.5653043665036784349 ) ) ;
#24400 = ORIENTED_EDGE ( 'NONE', *, *, #9835, .F. ) ;
#24401 = CONICAL_SURFACE ( 'NONE', #28965, 0.1624877031048690135, 0.1745329251994329756 ) ;
#24402 = EDGE_CURVE ( 'NONE', #23035, #9503, #9392, .T. ) ;
#24403 = EDGE_CURVE ( 'NONE', #4635, #4081, #12478, .T. ) ;
#24404 = UNCERTAINTY_MEASURE_WITH_UNIT (LENGTH_MEASURE( 1.000000000000000082E-05 ), #36843, 'distance_accuracy_value', 'NONE');
#24405 = CARTESIAN_POINT ( 'NONE',  ( 0.3831941804535738405, -1.607788291067505870, -0.3198167766998259998 ) ) ;
#24406 = VERTEX_POINT ( 'NONE', #15985 ) ;
#24407 = CARTESIAN_POINT ( 'NONE',  ( 0.2010877066827159720, -1.651987922488803440, -0.3292090611533607936 ) ) ;
#24408 = CIRCLE ( 'NONE', #5308, 0.01500000000000001159 ) ;
#24409 = CARTESIAN_POINT ( 'NONE',  ( 0.5009665901131933330, -1.376049689205368187, 0.8038812696496657750 ) ) ;
#24410 = CARTESIAN_POINT ( 'NONE',  ( 0.4664189868188083898, -1.671521195344378041, 0.4684108820178269350 ) ) ;
#24411 = CARTESIAN_POINT ( 'NONE',  ( 0.3999999999999787059, -2.166079853131637645, -0.4467913981637915422 ) ) ;
#24412 = AXIS2_PLACEMENT_3D ( 'NONE', #192, #37787, #3427 ) ;
#24413 = FACE_OUTER_BOUND ( 'NONE', #2185, .T. ) ;
#24414 = AXIS2_PLACEMENT_3D ( 'NONE', #3576, #28464, #339 ) ;
#24415 = PLANE ( 'NONE',  #37615 ) ;
#24416 = AXIS2_PLACEMENT_3D ( 'NONE', #17016, #5063, #35942 ) ;
#24417 = CARTESIAN_POINT ( 'NONE',  ( -0.1533385355407300699, 0.4750492940987078305, 0.3599999999999999867 ) ) ;
#24418 = DIRECTION ( 'NONE',  ( 1.000000000000000000, -1.023084414572551917E-11, -1.435532102222566415E-11 ) ) ;
#24419 = CARTESIAN_POINT ( 'NONE',  ( 0.1946137278002632309, -0.5377497569806550803, 0.3020257395598471839 ) ) ;
#24420 = CARTESIAN_POINT ( 'NONE',  ( -0.05186792262757213001, 0.2620061627190607423, 0.3911910583554848997 ) ) ;
#24421 = CARTESIAN_POINT ( 'NONE',  ( 0.01141983555232837372, -0.9471369104752583867, 0.2153783958211964722 ) ) ;
#24422 = CARTESIAN_POINT ( 'NONE',  ( 0.6169029553321203618, -1.567646591109399523, -0.4433873813970327094 ) ) ;
#24423 = CARTESIAN_POINT ( 'NONE',  ( 0.04765665840200696002, -1.630838948795847010, -0.6681089085276715744 ) ) ;
#24424 = CARTESIAN_POINT ( 'NONE',  ( 0.1186103394390872201, -1.414144848331978510, 0.5683298932114988489 ) ) ;
#24425 = CARTESIAN_POINT ( 'NONE',  ( 0.6983652742124539792, -1.438553779962960188, 0.5551970221657683835 ) ) ;
#24426 = CARTESIAN_POINT ( 'NONE',  ( -0.2746410161513776482, -4.385325017590463226, -0.5985264029706665045 ) ) ;
#24427 = ORIENTED_EDGE ( 'NONE', *, *, #20338, .T. ) ;
#24428 = DIRECTION ( 'NONE',  ( -1.000000000000000000, -2.341930812374887555E-31, 1.664003471950578127E-31 ) ) ;
#24429 = CARTESIAN_POINT ( 'NONE',  ( 0.5640895105453352931, -1.503407492374277510, 0.5358556994421860287 ) ) ;
#24430 = LINE ( 'NONE', #39440, #38308 ) ;
#24431 = VECTOR ( 'NONE', #34359, 39.37007874015748143 ) ;
#24432 = ADVANCED_FACE ( 'NONE', ( #37569, #28530 ), #14620, .F. ) ;
#24433 = CARTESIAN_POINT ( 'NONE',  ( 0.4621279655515690976, -1.664766036179415432, -0.6170834442379143914 ) ) ;
#24434 = EDGE_LOOP ( 'NONE', ( #203, #31933, #37383 ) ) ;
#24435 = CARTESIAN_POINT ( 'NONE',  ( 0.4685175142989152497, -1.068920175619711976, -0.6082962044498383403 ) ) ;
#24436 = CIRCLE ( 'NONE', #7996, 0.02499999999999993894 ) ;
#24437 = CIRCLE ( 'NONE', #6677, 0.04000000000000000777 ) ;
#24438 = FACE_OUTER_BOUND ( 'NONE', #10067, .T. ) ;
#24439 = CARTESIAN_POINT ( 'NONE',  ( 0.02881408050861173492, 0.2420347005671112106, -0.4354489374660193701 ) ) ;
#24440 = AXIS2_PLACEMENT_3D ( 'NONE', #27820, #9281, #40143 ) ;
#24441 = CARTESIAN_POINT ( 'NONE',  ( 0.4793721387301719816, -1.262504312832766651, 0.7257340988765215162 ) ) ;
#24443 = DIRECTION ( 'NONE',  ( -1.000000000000000000, 0.000000000000000000, 0.000000000000000000 ) ) ;
#24442 = CARTESIAN_POINT ( 'NONE',  ( -0.2399999999999999079, -2.139295658456680904, -0.3624034539465684213 ) ) ;
#24444 = CARTESIAN_POINT ( 'NONE',  ( 0.4930347527585871026, -1.093336683456308078, 0.6301225560750347565 ) ) ;
#24445 = VERTEX_POINT ( 'NONE', #19670 ) ;
#24446 = COORDINATED_UNIVERSAL_TIME_OFFSET ( 0, 0, .AHEAD. ) ;
#24447 = FACE_BOUND ( 'NONE', #3064, .T. ) ;
#24448 = ORIENTED_EDGE ( 'NONE', *, *, #19620, .T. ) ;
#24449 = CARTESIAN_POINT ( 'NONE',  ( -0.03868264068766708724, 0.3066108573455319508, -0.3648330973802349497 ) ) ;
#24450 = CARTESIAN_POINT ( 'NONE',  ( 0.3556005243248319680, -1.622197365539165936, 0.5664687466889557488 ) ) ;
#24452 = CARTESIAN_POINT ( 'NONE',  ( 0.1130246885457655975, -0.7035223855512272584, -0.09530233752769670663 ) ) ;
#24451 = LINE ( 'NONE', #28334, #24375 ) ;
#24453 = DIRECTION ( 'NONE',  ( 0.000000000000000000, -0.8660477418057305199, 0.4999613074160784154 ) ) ;
#24454 = ORIENTED_EDGE ( 'NONE', *, *, #15554, .T. ) ;
#24455 = ORIENTED_EDGE ( 'NONE', *, *, #38942, .T. ) ;
#24456 = CARTESIAN_POINT ( 'NONE',  ( 0.3793161018499474069, -0.9685596994469443111, 0.6812625861292541662 ) ) ;
#24457 = CARTESIAN_POINT ( 'NONE',  ( 0.3111660121705961957, -1.077154095635142417, 0.8049933954744191711 ) ) ;
#24458 = ORIENTED_EDGE ( 'NONE', *, *, #22995, .F. ) ;
#24459 = DIRECTION ( 'NONE',  ( -1.355854680848614260E-31, 3.330669073875470114E-16, 1.000000000000000000 ) ) ;
#24460 = DIRECTION ( 'NONE',  ( 0.000000000000000000, -0.3090169943749502823, -0.9510565162951527540 ) ) ;
#24461 = LINE ( 'NONE', #6125, #9313 ) ;
#24462 = AXIS2_PLACEMENT_3D ( 'NONE', #20171, #27360, #24075 ) ;
#24463 = CARTESIAN_POINT ( 'NONE',  ( -0.1062892842221577205, -0.4838739999896025101, 0.3472338291022580847 ) ) ;
#24464 = CARTESIAN_POINT ( 'NONE',  ( 0.3999999999999787059, -2.143627883852845528, -0.5325888117242426611 ) ) ;
#24465 = AXIS2_PLACEMENT_3D ( 'NONE', #30254, #14624, #39727 ) ;
#24466 = CARTESIAN_POINT ( 'NONE',  ( 0.5714515714113984624, -1.616742210554280135, 0.5707417262808793801 ) ) ;
#24467 = VECTOR ( 'NONE', #16282, 39.37007874015748143 ) ;
#24468 = CARTESIAN_POINT ( 'NONE',  ( 0.02953079040095717839, 0.4684706630666118365, 0.2484463060367366194 ) ) ;
#24469 = CARTESIAN_POINT ( 'NONE',  ( 0.2400364630114684983, -2.004548383824730884, -0.6718252909726382116 ) ) ;
#24470 = DIRECTION ( 'NONE',  ( 0.8660512985181133550, 0.4999551463232370652, 0.000000000000000000 ) ) ;
#24471 = PERSON_AND_ORGANIZATION ( #28500, #32463 ) ;
#24472 = CIRCLE ( 'NONE', #6030, 0.05000000000000000971 ) ;
#24473 = CARTESIAN_POINT ( 'NONE',  ( 0.4808682371952084367, -1.130070160517919753, 0.4859207442516079722 ) ) ;
#24474 = CARTESIAN_POINT ( 'NONE',  ( 0.4510981778992304569, -1.245710572978114161, 0.6057417262809815517 ) ) ;
#24475 = LINE ( 'NONE', #30442, #922 ) ;
#24476 = CARTESIAN_POINT ( 'NONE',  ( 0.0003542010310559907385, -0.4591614539952885155, 0.04612386700675097373 ) ) ;
#24477 = CARTESIAN_POINT ( 'NONE',  ( 0.0004750592482352814579, -0.4386115460793976739, 0.1457185332388683252 ) ) ;
#24478 = CARTESIAN_POINT ( 'NONE',  ( 0.0004755335033020558909, -0.4388027427473707998, 0.1568150681250891076 ) ) ;
#24479 = CARTESIAN_POINT ( 'NONE',  ( 0.5953303036072959964, -1.457508885835639978, 0.6057417262805095959 ) ) ;
#24480 = EDGE_CURVE ( 'NONE', #10169, #35222, #7223, .T. ) ;
#24481 = EDGE_LOOP ( 'NONE', ( #9307, #21511, #14828, #35331 ) ) ;
#24482 = EDGE_CURVE ( 'NONE', #5559, #35870, #10532, .T. ) ;
#24483 = ORIENTED_EDGE ( 'NONE', *, *, #30346, .F. ) ;
#24484 = LINE ( 'NONE', #30849, #6579 ) ;
#24485 = ORIENTED_EDGE ( 'NONE', *, *, #15935, .F. ) ;
#24486 = DIRECTION ( 'NONE',  ( 1.000000000000000000, 0.000000000000000000, 0.000000000000000000 ) ) ;
#24487 = EDGE_CURVE ( 'NONE', #9452, #37238, #5519, .T. ) ;
#24488 = AXIS2_PLACEMENT_3D ( 'NONE', #13626, #39136, #35430 ) ;
#24489 = CARTESIAN_POINT ( 'NONE',  ( 0.1499999999999993561, 0.07651041855119031232, -0.5222379212568211138 ) ) ;
#24491 = EDGE_LOOP ( 'NONE', ( #6812, #23200, #20611, #5813 ) ) ;
#24490 = CARTESIAN_POINT ( 'NONE',  ( 0.01056578810015139022, -0.5296855280550349931, 0.1486859626770064002 ) ) ;
#24492 = ADVANCED_FACE ( 'NONE', ( #22789 ), #22387, .T. ) ;
#24493 = VERTEX_POINT ( 'NONE', #35492 ) ;
#24494 = CARTESIAN_POINT ( 'NONE',  ( -0.1731185243557763487, 0.5373335498847187086, 0.09999999999999989453 ) ) ;
#24495 = CIRCLE ( 'NONE', #34991, 0.02499999999999998404 ) ;
#24496 = EDGE_LOOP ( 'NONE', ( #15684, #9623, #3336, #8628 ) ) ;
#24497 = AXIS2_PLACEMENT_3D ( 'NONE', #29428, #1274, #26552 ) ;
#24498 = CARTESIAN_POINT ( 'NONE',  ( 0.2654089594124767748, -1.674916358741208144, 0.5606694567451773192 ) ) ;
#24500 = CARTESIAN_POINT ( 'NONE',  ( 0.1691312463165446367, -1.239161314218422127, 0.5978938133338337346 ) ) ;
#24499 = CARTESIAN_POINT ( 'NONE',  ( 0.3538654265270187449, -1.126342156508903791, 0.7354529254703474628 ) ) ;
#24501 = CARTESIAN_POINT ( 'NONE',  ( -0.1157923916715204865, -0.5295015842444287246, 0.1380392329925466954 ) ) ;
#24502 = DATE_TIME_ROLE ( 'classification_date' ) ;
#24503 = AXIS2_PLACEMENT_3D ( 'NONE', #4490, #29597, #10890 ) ;
#24504 = CARTESIAN_POINT ( 'NONE',  ( 0.5382316988408143432, -1.161161114027098318, 0.5682417262808693303 ) ) ;
#24506 = VERTEX_POINT ( 'NONE', #38590 ) ;
#24505 = EDGE_LOOP ( 'NONE', ( #12154, #29397, #25264, #20391 ) ) ;
#24507 = CARTESIAN_POINT ( 'NONE',  ( 0.1772434461258276250, -1.460886006248064639, -0.3542314186169536749 ) ) ;
#24508 = CARTESIAN_POINT ( 'NONE',  ( 0.3424415908864473779, -1.747937484235617012, 0.4483338674949445268 ) ) ;
#24509 = CARTESIAN_POINT ( 'NONE',  ( -0.05268850283020078823, -0.4471020566665147578, 0.1404229504685532148 ) ) ;
#24510 = B_SPLINE_SURFACE_WITH_KNOTS ( 'NONE', 3, 3, ( 
 ( #22638, #3275, #25704, #22031, #40523, #19339, #34746, #22425, #34552, #2880, #248, #12538, #12961, #22231, #37425, #19543, #15830, #25093, #19131, #9238, #21813, #16253, #38235, #16046, #6157, #649, #6364, #12746, #37847, #18721, #18933, #31669, #34953, #463, #31277, #31878, #10064 ),
 ( #15634, #28181, #46, #3486, #28592, #37629, #31468, #6971, #15433, #29589, #38448, #23454, #7778, #1244, #20347, #10282, #13563, #22848, #1434, #29192, #16433, #29798, #32866, #35972, #19723, #16857, #25925, #13948, #32075, #26310, #4076, #20150, #4675, #1640, #35367, #29400, #26130 ),
 ( #17247, #26729, #23641, #10884, #36161, #1054, #35556, #38644, #32678, #13745, #26517, #14159, #7576, #39258, #32256, #17048, #11081, #4484, #16643, #38837, #4291, #39053, #10666, #10463, #3881, #7972, #28977, #842, #13350, #23029, #19930, #7157, #7353, #32466, #23238, #35765, #24240 ),
 ( #17456, #27723, #11275, #14554, #5278, #17844, #33079, #30807, #8383, #40258, #12091, #24657, #8185, #1838, #23842, #36364, #37187, #26918, #20951, #24441, #33681, #30403, #20546, #14354, #2234, #5492, #4889, #18060, #39652, #8574, #2436, #30005, #33473, #11489, #39448, #20759, #14774 ),
 ( #30611, #27336, #33281, #5088, #39865, #30194, #11686, #17648, #2024, #33908, #15163, #14973, #27122, #21370, #24054, #36580, #36763, #40049, #21152, #27527, #11871, #36973, #8793, #5705, #18263, #2628, #25248, #37992, #9189, #34697, #31823, #9609, #37376, #31423, #21972, #37789, #3225 ),
 ( #31007, #195, #28320, #34501, #16204, #12687, #2828, #410, #21757, #22184, #40475, #18453, #25653, #6312, #5893, #28739, #12297, #3044, #18884, #15774, #21567, #19283, #37573, #601, #13095, #9005, #34292, #15379, #24856, #6097, #34090, #27935, #9396, #12905, #6504, #19075, #18666 ),
 ( #31229, #31613, #15589, #3430, #3642, #28136, #1, #25460, #15989, #28534, #12481, #25036, #9801, #22374, #34896, #6708, #32020, #14107, #10415, #7106, #16806, #6915, #19489, #10831, #32815, #10610, #3828, #38999, #4024, #22976, #35495, #16383, #13512, #7301, #32629, #35712, #28924 ),
 ( #29352, #789, #13299, #25871, #38386, #35109, #29741, #10224, #4238, #4436, #38594, #1193, #17193, #22793, #19880, #32415, #13696, #35316, #19673, #16590, #32209, #29136, #10012, #13888, #1584, #38184, #22582, #26463, #998, #23187, #26075, #26263, #20099, #38781, #7520, #16996, #29538 ),
 ( #1379, #23406, #35923, #7730, #20295, #4619, #39599, #36309, #5237, #36110, #7916, #40004, #21315, #39815, #20489, #27479, #33237, #11434, #24000, #33026, #1979, #36529, #21099, #24198, #4829, #18001, #2384, #8340, #14924, #17400, #8130, #29960, #36721, #23787, #11035, #24387, #11826 ),
 ( #5655, #14309, #20909, #27066, #30350, #11221, #26871, #5044, #1796, #17606, #39214, #36922, #30758, #2577, #23594, #8737, #33853, #30561, #2181, #8530, #20705, #39402, #26681, #18210, #14501, #30151, #33431, #14719, #17792, #33625, #27284, #11640, #5439, #24987, #7027, #40618, #21524 ) ),
 .UNSPECIFIED., .F., .F., .F.,
 ( 4, 3, 3, 4 ),
 ( 4, 3, 3, 3, 3, 3, 3, 3, 3, 3, 3, 3, 4 ),
 ( 0.2346684314605614330, 0.4922368959575419423, 0.6210211282060321691, 0.7498053604545223960 ),
 ( 0.002735921434322369401, 0.006796569813770247936, 0.01085721819321812734, 0.01897851495211388614, 0.03522110846990540028, 0.05146370198769691096, 0.06770629550548842857, 0.08394888902327994618, 0.1001914825410714638, 0.1326766695766544990, 0.1651618566122375342, 0.1976470436478205417, 0.2626174177189866121 ),
 .UNSPECIFIED. ) ;
#24511 = CARTESIAN_POINT ( 'NONE',  ( 0.4662195773891402162, -1.247030207462705986, 0.8121041408566435083 ) ) ;
#24512 = AXIS2_PLACEMENT_3D ( 'NONE', #32143, #17321, #35630 ) ;
#24513 = EDGE_CURVE ( 'NONE', #617, #30709, #7992, .T. ) ;
#24514 = CARTESIAN_POINT ( 'NONE',  ( -2.128119112016648632E-14, -2.087870288139423103, -0.7252158372584678325 ) ) ;
#24515 = CARTESIAN_POINT ( 'NONE',  ( 0.1266021694322588542, -1.239399129679921829, 0.5182417262812423209 ) ) ;
#24516 = APPLIED_DATE_AND_TIME_ASSIGNMENT ( #28359, #22213, ( #37836 ) ) ;
#24517 = CARTESIAN_POINT ( 'NONE',  ( 0.3218125531527813998, -1.760402285594251159, 0.6125947341875596086 ) ) ;
#24518 = CARTESIAN_POINT ( 'NONE',  ( 0.3830298086532948343, -1.726706798021515610, 0.4282875075352186034 ) ) ;
#24519 = DIRECTION ( 'NONE',  ( -7.000205099780314469E-17, -1.000000000000000000, 6.590151126658399604E-16 ) ) ;
#24520 = DIRECTION ( 'NONE',  ( 1.000000000000000000, 0.000000000000000000, 0.000000000000000000 ) ) ;
#24521 = CARTESIAN_POINT ( 'NONE',  ( 0.5714515714113984624, -1.616742210554280135, 0.5707417262808793801 ) ) ;
#24522 =( BOUNDED_SURFACE ( )  B_SPLINE_SURFACE ( 3, 2, ( 
 ( #12393, #24950, #21877 ),
 ( #6415, #25564, #22483 ),
 ( #34405, #308, #6221 ),
 ( #31339, #12203, #37904 ) ),
 .UNSPECIFIED., .F., .F., .F. ) 
 B_SPLINE_SURFACE_WITH_KNOTS ( ( 4, 4 ),
 ( 3, 3 ),
 ( -3.035766082959412415E-18, 0.0002157631431912795808 ),
 ( 0.000000000000000000, 1.000000000000000000 ),
 .UNSPECIFIED. ) 
 GEOMETRIC_REPRESENTATION_ITEM ( )  RATIONAL_B_SPLINE_SURFACE ( (
 ( 1.000000000000000000, 0.6984366549430296445, 1.000000000000000000),
 ( 1.000000000000000000, 0.6988655720237708646, 1.000000000000000000),
 ( 1.000000000000000000, 0.6993079394701908758, 1.000000000000000000),
 ( 1.000000000000000000, 0.6997606559984659302, 1.000000000000000000) ) ) 
 REPRESENTATION_ITEM ( '' )  SURFACE ( )  );
#24523 = CARTESIAN_POINT ( 'NONE',  ( 0.4051897154098655363, -1.104944129929064101, 0.6010342342611436628 ) ) ;
#24524 = CARTESIAN_POINT ( 'NONE',  ( 0.3428182734493427919, -1.642767540764730416, -0.3789368674292417083 ) ) ;
#24525 =( LENGTH_UNIT ( ) NAMED_UNIT ( * ) SI_UNIT ( $, .METRE. ) );
#24526 = AXIS2_PLACEMENT_3D ( 'NONE', #13725, #29381, #4270 ) ;
#24527 = CARTESIAN_POINT ( 'NONE',  ( 0.2161879510971927987, -1.277123080371499242, -0.7187326247832955817 ) ) ;
#24528 = CARTESIAN_POINT ( 'NONE',  ( 0.01197363197122058853, -0.5805133742323803636, 0.4689902101802463363 ) ) ;
#24529 = CARTESIAN_POINT ( 'NONE',  ( 0.04888454729359380940, -1.019292185716472732, 0.7074266517341860627 ) ) ;
#24530 = CALENDAR_DATE ( 2026, 13, 10 ) ;
#24531 = TOROIDAL_SURFACE ( 'NONE', #33702, 0.5250000000000000222, 0.01499999999999999944 ) ;
#24532 = CARTESIAN_POINT ( 'NONE',  ( 0.7168528728721502707, -1.464418552067108470, 0.6746166867755808427 ) ) ;
#24533 = AXIS2_PLACEMENT_3D ( 'NONE', #23827, #39244, #36349 ) ;
#24534 = CARTESIAN_POINT ( 'NONE',  ( -2.070754768975504589, -0.09959325338431362917, 0.3599999999999976552 ) ) ;
#24535 = CARTESIAN_POINT ( 'NONE',  ( 0.05561375719525327166, -0.02040745343123889777, -0.4604703763991774834 ) ) ;
#24536 = AXIS2_PLACEMENT_3D ( 'NONE', #39942, #40134, #21027 ) ;
#24537 = ADVANCED_FACE ( 'NONE', ( #14103 ), #36107, .T. ) ;
#24538 = AXIS2_PLACEMENT_3D ( 'NONE', #8508, #34015, #31145 ) ;
#24539 = CARTESIAN_POINT ( 'NONE',  ( 0.3395458163374477922, -1.664374608384261878, -0.3921577936940786602 ) ) ;
#24540 = VERTEX_POINT ( 'NONE', #11032 ) ;
#24541 = CARTESIAN_POINT ( 'NONE',  ( 0.000000000000000000, 0.000000000000000000, 0.000000000000000000 ) ) ;
#24542 = CARTESIAN_POINT ( 'NONE',  ( 0.2585116059216619466, -1.600704214304080608, 0.8541279405034801764 ) ) ;
#24543 = EDGE_CURVE ( 'NONE', #4931, #21660, #2618, .T. ) ;
#24544 = CARTESIAN_POINT ( 'NONE',  ( 0.5884674137009996420, -1.491157991441193209, 0.5851315895956400448 ) ) ;
#24546 = ORIENTED_EDGE ( 'NONE', *, *, #38802, .T. ) ;
#24545 = CARTESIAN_POINT ( 'NONE',  ( 0.3441766385685567364, -1.748888513973746228, 0.4490806875465770398 ) ) ;
#24547 = EDGE_CURVE ( 'NONE', #27939, #32882, #27630, .T. ) ;
#24548 = CARTESIAN_POINT ( 'NONE',  ( 0.2254586261693722060, -0.6723955984770768612, 0.4589204916406527945 ) ) ;
#24550 = ORIENTED_EDGE ( 'NONE', *, *, #6683, .F. ) ;
#24549 = ORIENTED_EDGE ( 'NONE', *, *, #22230, .F. ) ;
#24551 = CARTESIAN_POINT ( 'NONE',  ( 0.1734973056165642902, -1.209394307038482497, -0.5155029497116575543 ) ) ;
#24552 = CARTESIAN_POINT ( 'NONE',  ( 0.05999999999999990757, -0.4893429041855150707, -0.1489153186320146816 ) ) ;
#24553 = LINE ( 'NONE', #28047, #8825 ) ;
#24554 = CALENDAR_DATE ( 2026, 13, 10 ) ;
#24555 = CARTESIAN_POINT ( 'NONE',  ( -0.1499999999999996336, 0.000000000000000000, 0.000000000000000000 ) ) ;
#24556 = EDGE_LOOP ( 'NONE', ( #33426, #29803, #37190, #15707 ) ) ;
#24557 = CARTESIAN_POINT ( 'NONE',  ( 0.08982948562931099279, -0.7300237816344226083, 0.2455375391678501773 ) ) ;
#24558 = AXIS2_PLACEMENT_3D ( 'NONE', #32156, #35651, #32564 ) ;
#24559 = CARTESIAN_POINT ( 'NONE',  ( -0.02000000000000000042, -1.761115123485013534, -0.1975702831323159492 ) ) ;
#24560 = AXIS2_PLACEMENT_3D ( 'NONE', #29785, #1627, #1045 ) ;
#24561 = CARTESIAN_POINT ( 'NONE',  ( 0.1038461025547566530, -0.5461054185183505938, 0.1537531581841332651 ) ) ;
#24563 = CARTESIAN_POINT ( 'NONE',  ( 0.07044958284825096617, -1.315011783116714073, 0.5339628106424040288 ) ) ;
#24562 = DIRECTION ( 'NONE',  ( -2.682900528199994008E-31, 0.9510565162951504226, -0.3090169943749569437 ) ) ;
#24564 = ADVANCED_FACE ( 'NONE', ( #20485 ), #10827, .T. ) ;
#24565 = CARTESIAN_POINT ( 'NONE',  ( 0.02056819537566472247, -1.080172155999248318, 0.6281642683093259238 ) ) ;
#24566 = VERTEX_POINT ( 'NONE', #13508 ) ;
#24567 = ORIENTED_EDGE ( 'NONE', *, *, #18557, .F. ) ;
#24568 = DIRECTION ( 'NONE',  ( 1.000000000000000000, 2.280301054154495132E-31, -1.664003471950577689E-31 ) ) ;
#24569 = CARTESIAN_POINT ( 'NONE',  ( 0.2465799821153819571, -0.7910269351804194438, 0.7388407842391677693 ) ) ;
#24570 = VECTOR ( 'NONE', #14813, 39.37007874015748143 ) ;
#24571 = DIRECTION ( 'NONE',  ( 0.4999551463232372317, -0.8660512985181134660, 0.000000000000000000 ) ) ;
#24572 = CIRCLE ( 'NONE', #40319, 0.01499999999999996302 ) ;
#24573 = DIRECTION ( 'NONE',  ( -7.000205099780314469E-17, -1.000000000000000000, 6.590151126658399604E-16 ) ) ;
#24574 = DIRECTION ( 'NONE',  ( -6.162975822039154046E-33, 0.000000000000000000, -1.000000000000000000 ) ) ;
#24575 = CARTESIAN_POINT ( 'NONE',  ( 0.3184462859233389564, -1.172215077377981585, 0.5535637004880700207 ) ) ;
#24576 = CARTESIAN_POINT ( 'NONE',  ( 0.1886295724182434630, -0.6892155111403490686, 0.2012867199884409153 ) ) ;
#24577 = APPROVAL_DATE_TIME ( #23006, #26276 ) ;
#24578 = DIRECTION ( 'NONE',  ( 0.000000000000000000, 0.000000000000000000, 1.000000000000000000 ) ) ;
#24579 = AXIS2_PLACEMENT_3D ( 'NONE', #27334, #33077, #20758 ) ;
#24580 = CARTESIAN_POINT ( 'NONE',  ( 0.3594221198575611176, -1.931599736257602284, -0.6668497031992260959 ) ) ;
#24581 = DIRECTION ( 'NONE',  ( -1.000000000000000000, -7.857794173099924470E-32, -8.628166150854818811E-32 ) ) ;
#24582 = CARTESIAN_POINT ( 'NONE',  ( -0.02872242845530496164, -0.3729171224323663547, -0.3802687114177501493 ) ) ;
#24583 = AXIS2_PLACEMENT_3D ( 'NONE', #35488, #10407, #12898 ) ;
#24584 = EDGE_CURVE ( 'NONE', #17702, #12964, #1793, .T. ) ;
#24585 = AXIS2_PLACEMENT_3D ( 'NONE', #12607, #28064, #34628 ) ;
#24586 = VERTEX_POINT ( 'NONE', #32412 ) ;
#24587 = DIRECTION ( 'NONE',  ( 0.4999551463232373427, -0.8660512985181134660, 0.000000000000000000 ) ) ;
#24588 = FACE_OUTER_BOUND ( 'NONE', #22087, .T. ) ;
#24589 = EDGE_CURVE ( 'NONE', #26219, #37479, #17773, .T. ) ;
#24590 = DIRECTION ( 'NONE',  ( 1.000000000000000000, 0.000000000000000000, 0.000000000000000000 ) ) ;
#24591 = VERTEX_POINT ( 'NONE', #4234 ) ;
#24592 = CARTESIAN_POINT ( 'NONE',  ( -0.05187277790672318450, -0.01792103310036803968, -0.4704724753798314452 ) ) ;
#24593 = AXIS2_PLACEMENT_3D ( 'NONE', #40018, #11095, #20360 ) ;
#24594 = CARTESIAN_POINT ( 'NONE',  ( 0.05336070580022266724, -1.000409524100160485, 0.6919889636817496692 ) ) ;
#24596 = ORIENTED_EDGE ( 'NONE', *, *, #38360, .T. ) ;
#24595 = ORIENTED_EDGE ( 'NONE', *, *, #33881, .F. ) ;
#24597 = CARTESIAN_POINT ( 'NONE',  ( 0.3163627804571104707, -1.761805152290217613, 0.5682287416806770519 ) ) ;
#24598 = CARTESIAN_POINT ( 'NONE',  ( 0.04157078424165364799, -0.01703670724029039338, 0.4699541233906588955 ) ) ;
#24599 = CARTESIAN_POINT ( 'NONE',  ( 0.03478489236951080865, -0.4639981600178390564, -0.2267640475915320142 ) ) ;
#24600 = CARTESIAN_POINT ( 'NONE',  ( 0.3699999999999789013, -2.087706782572656738, -0.4706861924077629378 ) ) ;
#24601 = CARTESIAN_POINT ( 'NONE',  ( 0.3644626074408009453, -1.765287842794585726, -0.5889622461435645162 ) ) ;
#24603 = CARTESIAN_POINT ( 'NONE',  ( 0.005475248526801685008, -0.9459170876539717554, 0.1457173627829773666 ) ) ;
#24602 = CARTESIAN_POINT ( 'NONE',  ( 0.04229883635638006373, 0.4470233673486206927, 0.1406638142521503265 ) ) ;
#24604 = CARTESIAN_POINT ( 'NONE',  ( -0.05634307799789443211, -0.2614070397638467713, -0.3772863199289407388 ) ) ;
#24605 = ORIENTED_EDGE ( 'NONE', *, *, #4471, .T. ) ;
#24606 = CARTESIAN_POINT ( 'NONE',  ( 0.2003523658259203089, -0.8065114950566329988, 0.6680553503048993758 ) ) ;
#24607 = VERTEX_POINT ( 'NONE', #29956 ) ;
#24608 = DIRECTION ( 'NONE',  ( 1.000000000000000000, 2.276539994720214024E-15, -1.138269997360107012E-15 ) ) ;
#24609 = CARTESIAN_POINT ( 'NONE',  ( 0.06157545530246535254, -0.5616945561363291262, 0.2499708142322518700 ) ) ;
#24610 = ADVANCED_FACE ( 'NONE', ( #29348 ), #21146, .T. ) ;
#24612 = FACE_OUTER_BOUND ( 'NONE', #17545, .T. ) ;
#24611 = CARTESIAN_POINT ( 'NONE',  ( -0.08000000000000000167, -2.542046649843399564, -0.2305290188067205259 ) ) ;
#24613 = CARTESIAN_POINT ( 'NONE',  ( -0.1206014988277951117, -0.5041571071311164998, 0.1364167062886335602 ) ) ;
#24614 = LINE ( 'NONE', #32881, #31000 ) ;
#24615 = EDGE_CURVE ( 'NONE', #556, #7985, #16469, .T. ) ;
#24616 = VERTEX_POINT ( 'NONE', #11823 ) ;
#24617 = CIRCLE ( 'NONE', #12770, 0.07999999999999996003 ) ;
#24618 = CARTESIAN_POINT ( 'NONE',  ( -0.2399999999999999079, -2.391283043799508956, -0.6083071156998423046 ) ) ;
#24619 = EDGE_CURVE ( 'NONE', #10835, #15637, #33540, .T. ) ;
#24620 = CARTESIAN_POINT ( 'NONE',  ( 0.3871477414013556606, -1.840016465421978165, -0.5197212197501380748 ) ) ;
#24621 = AXIS2_PLACEMENT_3D ( 'NONE', #33872, #2406, #18637 ) ;
#24622 = CARTESIAN_POINT ( 'NONE',  ( 0.1787419356640313761, -0.7505968874023245530, 0.5623186377554705295 ) ) ;
#24623 = CARTESIAN_POINT ( 'NONE',  ( 0.4764753233885406503, -1.665949717495130766, 0.4947212307176814261 ) ) ;
#24624 = DIRECTION ( 'NONE',  ( -1.355854680848614260E-31, 3.330669073875470114E-16, 1.000000000000000000 ) ) ;
#24625 = AXIS2_PLACEMENT_3D ( 'NONE', #15577, #5880, #12288 ) ;
#24626 = AXIS2_PLACEMENT_3D ( 'NONE', #13697, #26264, #29539 ) ;
#24627 = ORIENTED_EDGE ( 'NONE', *, *, #5622, .F. ) ;
#24628 = DIRECTION ( 'NONE',  ( -1.000000000000000000, -0.000000000000000000, -0.000000000000000000 ) ) ;
#24629 = AXIS2_PLACEMENT_3D ( 'NONE', #28819, #9694, #10094 ) ;
#24630 = CARTESIAN_POINT ( 'NONE',  ( 0.2144086742444059612, -1.243025793896146869, 0.5645655484585248018 ) ) ;
#24631 = CARTESIAN_POINT ( 'NONE',  ( 0.6260846371513943964, -1.362782225785380996, -0.6250000000000000000 ) ) ;
#24632 = CARTESIAN_POINT ( 'NONE',  ( 0.4184753273149497965, -1.633759443312357007, -0.5155029497116575543 ) ) ;
#24633 = TOROIDAL_SURFACE ( 'NONE', #18713, 0.2200000000000000566, 0.02999999999999999889 ) ;
#24634 = CARTESIAN_POINT ( 'NONE',  ( 0.6791962457086077043, -1.401251971513146621, 0.6322342638419099492 ) ) ;
#24635 = CARTESIAN_POINT ( 'NONE',  ( -0.03877220711930155078, 0.3061923002804438076, 0.3649281646214391772 ) ) ;
#24636 = CARTESIAN_POINT ( 'NONE',  ( 0.01276022671919619343, -1.030438920969866334, 0.5664345702674732363 ) ) ;
#24637 = CARTESIAN_POINT ( 'NONE',  ( 0.6626821769541543228, -1.455497439629167777, -0.4141230538711661580 ) ) ;
#24638 = CARTESIAN_POINT ( 'NONE',  ( -0.3000000000000000999, -4.162452804151155483, -0.5855328176471856771 ) ) ;
#24639 = CARTESIAN_POINT ( 'NONE',  ( 0.1044625578173912356, -0.8429083989444113856, 0.3673943131971453835 ) ) ;
#24640 = CARTESIAN_POINT ( 'NONE',  ( 0.2681719626984005456, -1.674357821296572846, 0.5749781514038686536 ) ) ;
#24641 = CARTESIAN_POINT ( 'NONE',  ( 0.02953079040095704308, -0.09152108205201929525, 0.5223162075576431862 ) ) ;
#24642 = EDGE_LOOP ( 'NONE', ( #7150, #2286, #2533, #30170, #19271, #3596, #13461, #5701 ) ) ;
#24643 = CARTESIAN_POINT ( 'NONE',  ( 0.3596447502321097334, -1.738446402475701591, -0.5125164628055072225 ) ) ;
#24644 = CARTESIAN_POINT ( 'NONE',  ( 0.4034397895666202993, -1.737305379259379334, -0.5960298613879961849 ) ) ;
#24645 = CIRCLE ( 'NONE', #22042, 0.03000000000000002318 ) ;
#24646 = DIRECTION ( 'NONE',  ( 0.000000000000000000, 0.000000000000000000, 1.000000000000000000 ) ) ;
#24647 = EDGE_CURVE ( 'NONE', #20771, #30911, #39595, .T. ) ;
#24648 = CARTESIAN_POINT ( 'NONE',  ( 0.1499999999999989120, -0.3688619771572964612, -0.3775276577326955874 ) ) ;
#24649 = EDGE_CURVE ( 'NONE', #15212, #15646, #97, .T. ) ;
#24650 = AXIS2_PLACEMENT_3D ( 'NONE', #20084, #592, #3818 ) ;
#24651 = VERTEX_POINT ( 'NONE', #40202 ) ;
#24652 = CARTESIAN_POINT ( 'NONE',  ( 0.5137479461421968763, -1.668697091725908521, -0.5969086590007808280 ) ) ;
#24653 = DIRECTION ( 'NONE',  ( 0.000000000000000000, 3.414809992080324783E-15, -1.000000000000000000 ) ) ;
#24654 = LOCAL_TIME ( 0, 53, 7.000000000000000000, #37005 ) ;
#24655 = CYLINDRICAL_SURFACE ( 'NONE', #21766, 0.1762268159172277748 ) ;
#24656 = CYLINDRICAL_SURFACE ( 'NONE', #14734, 0.06000000000000045575 ) ;
#24657 = CARTESIAN_POINT ( 'NONE',  ( 0.5188837243650441522, -1.324382180592332148, 0.6742563569798550871 ) ) ;
#24659 = CARTESIAN_POINT ( 'NONE',  ( 0.5269601233575494925, -1.601707680730814598, -0.5991548076442045900 ) ) ;
#24658 = DIRECTION ( 'NONE',  ( -0.3468893892380665589, 0.7396492646828625173, -0.5767033179097742490 ) ) ;
#24660 = CARTESIAN_POINT ( 'NONE',  ( 0.2317493251130877951, -0.9016848682509819302, 0.4453502113744062241 ) ) ;
#24661 = ORIENTED_EDGE ( 'NONE', *, *, #2147, .T. ) ;
#24662 = APPROVAL_DATE_TIME ( #3231, #24017 ) ;
#24663 = AXIS2_PLACEMENT_3D ( 'NONE', #37970, #7444, #37764 ) ;
#24664 = DIRECTION ( 'NONE',  ( 0.4999999999999984457, 0.000000000000000000, -0.8660254037844394848 ) ) ;
#24665 = ORIENTED_EDGE ( 'NONE', *, *, #2018, .T. ) ;
#24666 = CARTESIAN_POINT ( 'NONE',  ( 2.048885995248197414E-16, 0.2900000000000004796, -5.122214988120493288E-16 ) ) ;
#24667 = B_SPLINE_CURVE_WITH_KNOTS ( 'NONE', 3,
 ( #29718, #8105, #4805, #17590 ),
 .UNSPECIFIED., .F., .F.,
 ( 4, 4 ),
 ( 0.4469892262121280546, 0.5550469413684232522 ),
 .UNSPECIFIED. ) ;
#24668 = VERTEX_POINT ( 'NONE', #37326 ) ;
#24669 = CARTESIAN_POINT ( 'NONE',  ( 0.03696608829255258744, -0.5625377656374845881, 0.2658259557143141660 ) ) ;
#24671 = CARTESIAN_POINT ( 'NONE',  ( 0.1855568200014149904, -0.7725989946471569780, 0.002349788420466783143 ) ) ;
#24670 = DIRECTION ( 'NONE',  ( -8.881784197001246407E-16, 2.361472542561082612E-16, -1.000000000000000000 ) ) ;
#24672 = DIRECTION ( 'NONE',  ( 0.4999999999999993894, -0.6415696268731904128, -0.5817116243241110540 ) ) ;
#24673 = ORIENTED_EDGE ( 'NONE', *, *, #34287, .T. ) ;
#24674 = ORIENTED_EDGE ( 'NONE', *, *, #18841, .F. ) ;
#24675 = CARTESIAN_POINT ( 'NONE',  ( 0.3744491522119342553, -1.096499884473891129, 0.6351544032997803457 ) ) ;
#24676 = CARTESIAN_POINT ( 'NONE',  ( 0.3711814119498326736, -1.195443994201320415, 0.8360198855415841290 ) ) ;
#24677 = ORIENTED_EDGE ( 'NONE', *, *, #39715, .T. ) ;
#24678 = FACE_OUTER_BOUND ( 'NONE', #15386, .T. ) ;
#24679 = PLANE ( 'NONE',  #17810 ) ;
#24680 = CARTESIAN_POINT ( 'NONE',  ( 0.5875120920308054551, -1.532572385145595684, -0.4099296195555359179 ) ) ;
#24681 = CARTESIAN_POINT ( 'NONE',  ( 0.4409062655693438137, -1.690090444797295977, -0.2869361388274795921 ) ) ;
#24682 = AXIS2_PLACEMENT_3D ( 'NONE', #10638, #39426, #17023 ) ;
#24683 = CARTESIAN_POINT ( 'NONE',  ( -0.07216878364870250862, 0.05141091571461216952, 0.1249999999999993477 ) ) ;
#24684 = CARTESIAN_POINT ( 'NONE',  ( 0.3931005117246323399, -1.715828765679402679, 0.3667417262808779777 ) ) ;
#24685 = LINE ( 'NONE', #37215, #22480 ) ;
#24686 = CARTESIAN_POINT ( 'NONE',  ( 0.2219773688075763474, -1.468623658325240333, -0.6797324060620716368 ) ) ;
#24687 = DIRECTION ( 'NONE',  ( -7.771561172376107616E-16, 7.170354002788761615E-17, -1.000000000000000000 ) ) ;
#24688 = COORDINATED_UNIVERSAL_TIME_OFFSET ( 0, 0, .AHEAD. ) ;
#24689 = LOCAL_TIME ( 0, 53, 7.000000000000000000, #27652 ) ;
#24690 = CARTESIAN_POINT ( 'NONE',  ( 0.4878316403371781851, -1.125113395602889810, 0.5164237391570506430 ) ) ;
#24691 = CARTESIAN_POINT ( 'NONE',  ( 0.4609248481599033109, -1.239710877643270814, 0.6057417262809816627 ) ) ;
#24692 = CARTESIAN_POINT ( 'NONE',  ( -0.2300000000000002875, 0.5182417262804733804, 0.1000000000000000194 ) ) ;
#24693 = CARTESIAN_POINT ( 'NONE',  ( 0.1233923337978296703, -1.433947342477501108, 0.6209663710929820279 ) ) ;
#24694 = CARTESIAN_POINT ( 'NONE',  ( 0.01548846960721252282, 0.2450655194478999765, 0.4674710490746267211 ) ) ;
#24695 = DIRECTION ( 'NONE',  ( -0.4999551463232372317, 0.8660512985181134660, -0.000000000000000000 ) ) ;
#24696 = CARTESIAN_POINT ( 'NONE',  ( 0.3434800707738534520, -1.169184835483325857, 0.4282596159935431746 ) ) ;
#24697 = EDGE_LOOP ( 'NONE', ( #28337, #14558, #3646, #26860 ) ) ;
#24698 = ORIENTED_EDGE ( 'NONE', *, *, #11943, .T. ) ;
#24699 = CARTESIAN_POINT ( 'NONE',  ( -0.1111952754772590757, -0.5081759048641385501, 0.1244868412816175218 ) ) ;
#24700 = ORIENTED_EDGE ( 'NONE', *, *, #37639, .T. ) ;
#24701 = CARTESIAN_POINT ( 'NONE',  ( 0.2637112460222606480, -1.676801009589977465, 0.5217148786151403206 ) ) ;
#24702 = LINE ( 'NONE', #9052, #40297 ) ;
#24703 = CARTESIAN_POINT ( 'NONE',  ( -0.3000000000000000999, -3.527715956914472706, -0.3920205355121876289 ) ) ;
#24705 = ORIENTED_EDGE ( 'NONE', *, *, #18335, .T. ) ;
#24704 = CARTESIAN_POINT ( 'NONE',  ( 0.002012706044603155327, -0.5245499851267817482, 0.1047619216058349734 ) ) ;
#24706 = VECTOR ( 'NONE', #12907, 39.37007874015748143 ) ;
#24707 = B_SPLINE_CURVE_WITH_KNOTS ( 'NONE', 3,
 ( #39536, #33566, #8285, #11369, #33378, #5181, #30285, #27221, #5381, #39284, #4321, #32893, #38866, #10699 ),
 .UNSPECIFIED., .F., .F.,
 ( 4, 2, 2, 2, 2, 2, 4 ),
 ( 1.262897753262582698E-17, 0.0007771926555927994576, 0.001554385311185586338, 0.001942981638981979833, 0.002331577966778373111, 0.002720174294574766605, 0.003108770622371160100 ),
 .UNSPECIFIED. ) ;
#24708 = CIRCLE ( 'NONE', #6944, 0.009999999999999894390 ) ;
#24709 = VERTEX_POINT ( 'NONE', #11429 ) ;
#24710 = CARTESIAN_POINT ( 'NONE',  ( 0.03868649100028155596, 0.4624880946332495801, -0.1149381524902354373 ) ) ;
#24711 = ORIENTED_EDGE ( 'NONE', *, *, #38374, .F. ) ;
#24712 = CARTESIAN_POINT ( 'NONE',  ( 0.008877318523083597632, -0.6275083649376383965, 0.4284230457359336497 ) ) ;
#24714 = CARTESIAN_POINT ( 'NONE',  ( 0.08830248264660876811, -1.300195518436201514, 0.5784869194914967760 ) ) ;
#24713 = CARTESIAN_POINT ( 'NONE',  ( 0.3720203041987413806, -1.150922219009145042, 0.7251981425757600963 ) ) ;
#24715 = APPLIED_APPROVAL_ASSIGNMENT ( #24017, ( #17475 ) ) ;
#24716 = DIRECTION ( 'NONE',  ( 1.000000000000000000, -1.693379103678898785E-12, 2.967165974375456995E-13 ) ) ;
#24717 = CARTESIAN_POINT ( 'NONE',  ( 0.4167269056019572426, -1.703721376542429722, -0.4188292666922682761 ) ) ;
#24719 = EDGE_LOOP ( 'NONE', ( #11383, #39045, #23022, #30359 ) ) ;
#24718 = VERTEX_POINT ( 'NONE', #39811 ) ;
#24720 = CARTESIAN_POINT ( 'NONE',  ( 0.4795819664771983071, -1.106247336020415917, -0.4111404562665418871 ) ) ;
#24721 = AXIS2_PLACEMENT_3D ( 'NONE', #1220, #13722, #26288 ) ;
#24722 = FACE_OUTER_BOUND ( 'NONE', #5670, .T. ) ;
#24723 = CARTESIAN_POINT ( 'NONE',  ( 0.01548846960707497486, -0.5198120922912106145, -0.07362328916748536733 ) ) ;
#24724 = CARTESIAN_POINT ( 'NONE',  ( 0.4998018223844837848, -1.298799938538372167, 0.7895654180778867159 ) ) ;
#24725 = DIRECTION ( 'NONE',  ( 0.8660512985181133550, 0.4999551463232373982, 0.000000000000000000 ) ) ;
#24726 = DIRECTION ( 'NONE',  ( -1.000000000000000000, 0.000000000000000000, 0.000000000000000000 ) ) ;
#24727 = B_SPLINE_CURVE_WITH_KNOTS ( 'NONE', 3,
 ( #19275, #31815, #3632, #28917 ),
 .UNSPECIFIED., .F., .F.,
 ( 4, 4 ),
 ( 6.254634441385501517E-18, 0.0006271655702610368002 ),
 .UNSPECIFIED. ) ;
#24728 = CARTESIAN_POINT ( 'NONE',  ( -0.1082158540381399775, -0.4935046016075750885, 0.3575786101922723281 ) ) ;
#24729 = CARTESIAN_POINT ( 'NONE',  ( 0.4611095784274710785, -1.074565241972302410, -0.4179763115151196029 ) ) ;
#24730 = CARTESIAN_POINT ( 'NONE',  ( 0.6586301574024518990, -1.563739711041315816, 0.4687417262808791230 ) ) ;
#24731 = DIRECTION ( 'NONE',  ( 0.000000000000000000, 1.821231995776161674E-15, -1.000000000000000000 ) ) ;
#24732 = CARTESIAN_POINT ( 'NONE',  ( 0.1399999999999994582, 4.857225732735059864E-17, 0.1249999999999999584 ) ) ;
#24733 = EDGE_CURVE ( 'NONE', #8537, #7737, #5279, .T. ) ;
#24734 = AXIS2_PLACEMENT_3D ( 'NONE', #15177, #24066, #36986 ) ;
#24735 = FACE_OUTER_BOUND ( 'NONE', #349, .T. ) ;
#24736 = ADVANCED_FACE ( 'NONE', ( #12244 ), #23997, .F. ) ;
#24737 = CARTESIAN_POINT ( 'NONE',  ( 0.2936473109780965429, -1.729059834919730809, 0.6366410771178455663 ) ) ;
#24738 = CARTESIAN_POINT ( 'NONE',  ( 0.04400829994862880817, -1.043756151267425603, 0.7156344331538354586 ) ) ;
#24739 = COORDINATED_UNIVERSAL_TIME_OFFSET ( 0, 0, .AHEAD. ) ;
#24740 = CARTESIAN_POINT ( 'NONE',  ( 0.6786648513340227673, -1.399193080605451334, 0.7803980693475389696 ) ) ;
#24741 = APPROVAL_PERSON_ORGANIZATION ( #24160, #3604, #8296 ) ;
#24742 = DIRECTION ( 'NONE',  ( 0.8660512985181133550, 0.4999551463232373982, 0.000000000000000000 ) ) ;
#24743 = CIRCLE ( 'NONE', #5014, 0.06250000000000001388 ) ;
#24744 = CARTESIAN_POINT ( 'NONE',  ( 0.05279905671744771628, 0.03987410640504355369, -0.4667149812770573503 ) ) ;
#24745 = EDGE_CURVE ( 'NONE', #15727, #34759, #29570, .T. ) ;
#24746 = CARTESIAN_POINT ( 'NONE',  ( 0.3439082139226234403, -1.634872185475882533, -0.4352343451533515206 ) ) ;
#24747 = ORIENTED_EDGE ( 'NONE', *, *, #1882, .T. ) ;
#24748 = CARTESIAN_POINT ( 'NONE',  ( 0.1901695884102587719, -0.5023773489605858344, 0.1477569985384105666 ) ) ;
#24749 = APPROVAL ( #40348, 'UNSPECIFIED' ) ;
#24750 = CARTESIAN_POINT ( 'NONE',  ( 0.2292083863995310611, -1.502172107109858379, 0.9124160356758439505 ) ) ;
#24751 = CARTESIAN_POINT ( 'NONE',  ( 0.5699498466869539204, -1.462345630761733739, 0.7181541738695536026 ) ) ;
#24753 = ORIENTED_EDGE ( 'NONE', *, *, #16465, .T. ) ;
#24752 = CARTESIAN_POINT ( 'NONE',  ( 0.2134937173224229212, -1.278678410919930730, -0.5155029497116575543 ) ) ;
#24754 = CARTESIAN_POINT ( 'NONE',  ( 0.5463261744266250108, -1.174184195093048277, 0.6317594707774240037 ) ) ;
#24756 = EDGE_LOOP ( 'NONE', ( #28232, #28194, #5551, #40527 ) ) ;
#24755 = ORIENTED_EDGE ( 'NONE', *, *, #23622, .F. ) ;
#24757 = LINE ( 'NONE', #37279, #13273 ) ;
#24758 = CARTESIAN_POINT ( 'NONE',  ( 0.3543612153453276070, -1.726706594326277822, -0.5324466127738753940 ) ) ;
#24759 = DIRECTION ( 'NONE',  ( 0.000000000000000000, 0.000000000000000000, 1.000000000000000000 ) ) ;
#24760 = ITEM_DEFINED_TRANSFORMATION ( 'NONE', 'NONE', #34435,  #27819 ) ;
#24761 = CARTESIAN_POINT ( 'NONE',  ( -0.05464101615137762630, -1.910390638264138685, -0.7420407338378623985 ) ) ;
#24762 = ORIENTED_EDGE ( 'NONE', *, *, #27831, .T. ) ;
#24763 = AXIS2_PLACEMENT_3D ( 'NONE', #8716, #14483, #36514 ) ;
#24764 = CARTESIAN_POINT ( 'NONE',  ( 0.09262515131973823868, -0.7343695447130378362, 0.2782437690132907315 ) ) ;
#24765 = CARTESIAN_POINT ( 'NONE',  ( 0.2211959769661342168, -1.309495541150525799, -0.4400554600884077350 ) ) ;
#24766 =( BOUNDED_SURFACE ( )  B_SPLINE_SURFACE ( 3, 2, ( 
 ( #27398, #4947, #11131 ),
 ( #21006, #18118, #14404 ),
 ( #29858, #2491, #14831 ),
 ( #17513, #11935, #1698 ),
 ( #4734, #20607, #23901 ),
 ( #27581, #39310, #24500 ),
 ( #26967, #36429, #39922 ),
 ( #36818, #30062, #1892 ),
 ( #40107, #11740, #2073 ),
 ( #37032, #14217, #20817 ),
 ( #5144, #17697, #36636 ),
 ( #39712, #26785, #24297 ),
 ( #14610, #30243, #8852 ),
 ( #27182, #11549, #5554 ),
 ( #8440, #36215, #8633 ),
 ( #21206, #33743, #30672 ),
 ( #24910, #18941, #34353 ),
 ( #37641, #28389, #33962 ),
 ( #5762, #12149, #12756 ),
 ( #15226, #37434, #18730 ),
 ( #19139, #9246, #27993 ),
 ( #27784, #40322, #24714 ),
 ( #34147, #31678, #30862 ),
 ( #12352, #18320, #6167 ),
 ( #9672, #34564, #54 ),
 ( #25317, #37245, #21823 ) ),
 .UNSPECIFIED., .F., .F., .F. ) 
 B_SPLINE_SURFACE_WITH_KNOTS ( ( 4, 2, 2, 2, 2, 2, 2, 2, 2, 2, 2, 2, 4 ),
 ( 3, 3 ),
 ( 0.000000000000000000, 0.0006596057055745040533, 0.001319211411149008107, 0.001978817116723512268, 0.002308619969510764241, 0.002638422822298016213, 0.002968225675085268619, 0.003298028527872520592, 0.003627831380659772564, 0.003957634233447024537, 0.004617239939021528482, 0.004947042791808780454, 0.005276845644596032427 ),
 ( 0.000000000000000000, 1.000000000000000000 ),
 .UNSPECIFIED. ) 
 GEOMETRIC_REPRESENTATION_ITEM ( )  RATIONAL_B_SPLINE_SURFACE ( (
 ( 1.000000000000000000, 0.7087361850990782086, 1.000000000000000000),
 ( 1.000000000000000000, 0.6765739502726043630, 1.000000000000000000),
 ( 1.000000000000000000, 0.6402241378258116677, 1.000000000000000000),
 ( 1.000000000000000000, 0.5685252139047779485, 1.000000000000000000),
 ( 1.000000000000000000, 0.5311641938883238101, 1.000000000000000000),
 ( 1.000000000000000000, 0.4614670254680833250, 1.000000000000000000),
 ( 1.000000000000000000, 0.4296915687615939228, 1.000000000000000000),
 ( 1.000000000000000000, 0.3941419833073060430, 1.000000000000000000),
 ( 1.000000000000000000, 0.3843396926333228492, 1.000000000000000000),
 ( 1.000000000000000000, 0.3710601004298905159, 1.000000000000000000),
 ( 1.000000000000000000, 0.3677117356413553417, 1.000000000000000000),
 ( 1.000000000000000000, 0.3678937320958496904, 1.000000000000000000),
 ( 1.000000000000000000, 0.3715092472210990704, 1.000000000000000000),
 ( 1.000000000000000000, 0.3844660984943514825, 1.000000000000000000),
 ( 1.000000000000000000, 0.3936923856040987491, 1.000000000000000000),
 ( 1.000000000000000000, 0.4158998654390018701, 1.000000000000000000),
 ( 1.000000000000000000, 0.4289333015709035357, 1.000000000000000000),
 ( 1.000000000000000000, 0.4565842304191866652, 1.000000000000000000),
 ( 1.000000000000000000, 0.4712877118585055980, 1.000000000000000000),
 ( 1.000000000000000000, 0.5188537258417635911, 1.000000000000000000),
 ( 1.000000000000000000, 0.5552410424637538311, 1.000000000000000000),
 ( 1.000000000000000000, 0.6097807446480927318, 1.000000000000000000),
 ( 1.000000000000000000, 0.6288539315404778618, 1.000000000000000000),
 ( 1.000000000000000000, 0.6690853270610633841, 1.000000000000000000),
 ( 1.000000000000000000, 0.6898774606012713084, 1.000000000000000000),
 ( 1.000000000000000000, 0.7100124105822595011, 1.000000000000000000) ) ) 
 REPRESENTATION_ITEM ( '' )  SURFACE ( )  );
#24767 = CARTESIAN_POINT ( 'NONE',  ( 0.1579296938348824231, -0.7527599258947673677, 0.5723136178885942504 ) ) ;
#24769 = CARTESIAN_POINT ( 'NONE',  ( 0.002222032174280575301, -0.5198793158962575767, 0.1346323604582328748 ) ) ;
#24768 = CARTESIAN_POINT ( 'NONE',  ( 0.3263566400396368250, -1.758504154136070863, 0.4800462819687809080 ) ) ;
#24770 = CARTESIAN_POINT ( 'NONE',  ( -0.05634307799789442517, -0.2780413953411582928, 0.3652007531760607661 ) ) ;
#24771 = SECURITY_CLASSIFICATION ( '', '', #35827 ) ;
#24772 = ORIENTED_EDGE ( 'NONE', *, *, #34264, .T. ) ;
#24773 = DIRECTION ( 'NONE',  ( -0.1871397384865033098, -0.9823333030490228879, 2.482107064044991629E-16 ) ) ;
#24774 = CARTESIAN_POINT ( 'NONE',  ( 0.3251954281970569904, -0.9255269374606153177, 0.8255160753196725265 ) ) ;
#24775 = ADVANCED_FACE ( 'NONE', ( #38134 ), #25604, .T. ) ;
#24776 = CIRCLE ( 'NONE', #28062, 0.1033070866141734129 ) ;
#24777 = CARTESIAN_POINT ( 'NONE',  ( 0.02953079040095673430, -0.2329676531120485339, -0.4763574306556319637 ) ) ;
#24778 = EDGE_CURVE ( 'NONE', #6931, #33948, #36191, .T. ) ;
#24779 = CARTESIAN_POINT ( 'NONE',  ( 0.4685502202651029569, -1.116536938686066183, 0.5688043585934901003 ) ) ;
#24780 =( LENGTH_UNIT ( ) NAMED_UNIT ( * ) SI_UNIT ( $, .METRE. ) );
#24781 = ADVANCED_FACE ( 'NONE', ( #19024 ), #15819, .T. ) ;
#24782 = CARTESIAN_POINT ( 'NONE',  ( 0.07014435923142441076, -1.325199841737237261, 0.5075297796642793680 ) ) ;
#24783 = EDGE_CURVE ( 'NONE', #33509, #19821, #2695, .T. ) ;
#24784 = CARTESIAN_POINT ( 'NONE',  ( 0.02319709399062810581, -1.613360830953564973, -0.6353126625343105127 ) ) ;
#24785 = EDGE_CURVE ( 'NONE', #3931, #10985, #13248, .T. ) ;
#24786 = DIRECTION ( 'NONE',  ( 0.000000000000000000, 0.000000000000000000, 1.000000000000000000 ) ) ;
#24787 = CARTESIAN_POINT ( 'NONE',  ( 0.4556718857535577705, -1.059138143784118302, 0.6919068033735837897 ) ) ;
#24788 = CALENDAR_DATE ( 2026, 13, 10 ) ;
#24789 = FACE_OUTER_BOUND ( 'NONE', #6930, .T. ) ;
#24790 = AXIS2_PLACEMENT_3D ( 'NONE', #5588, #12378, #24933 ) ;
#24791 = CARTESIAN_POINT ( 'NONE',  ( 0.1959911413068460284, -1.662491970225822735, -0.6568654529857578250 ) ) ;
#24792 = CARTESIAN_POINT ( 'NONE',  ( -0.3000000000000000999, -2.376910030844113564, -0.7058185084100425666 ) ) ;
#24793 = CARTESIAN_POINT ( 'NONE',  ( -0.2746410161513779258, -2.183180860297908144, -0.2991170932241127844 ) ) ;
#24794 = EDGE_CURVE ( 'NONE', #38515, #7881, #25695, .T. ) ;
#24795 = VERTEX_POINT ( 'NONE', #16152 ) ;
#24796 = CARTESIAN_POINT ( 'NONE',  ( -2.070754768975505034, -0.09959325338431362917, 0.08499999999999909017 ) ) ;
#24797 = APPLIED_PERSON_AND_ORGANIZATION_ASSIGNMENT ( #2265, #2469, ( #22018 ) ) ;
#24798 = PLANE ( 'NONE',  #79 ) ;
#24799 = CARTESIAN_POINT ( 'NONE',  ( 0.1999999999999789724, -2.183180860297921466, -0.4937760292030871079 ) ) ;
#24800 = VERTEX_POINT ( 'NONE', #35053 ) ;
#24801 = CARTESIAN_POINT ( 'NONE',  ( -0.04574984450155245713, 0.06505050184193394980, -0.4827809015761244105 ) ) ;
#24802 = CARTESIAN_POINT ( 'NONE',  ( 0.01407560669633875494, -0.9971709087417149897, 0.6860632370118421308 ) ) ;
#24804 = ORIENTED_EDGE ( 'NONE', *, *, #26651, .F. ) ;
#24803 = EDGE_LOOP ( 'NONE', ( #4491, #4140, #10721 ) ) ;
#24805 = CARTESIAN_POINT ( 'NONE',  ( -0.1167294259372919918, -0.5331983348239598408, 0.1528658435936951776 ) ) ;
#24806 = CARTESIAN_POINT ( 'NONE',  ( 0.05201782277453272096, -0.01807851807932046515, 0.4701313241416045230 ) ) ;
#24807 = CARTESIAN_POINT ( 'NONE',  ( 0.7371735653322752935, -1.498976209023650696, 0.6847608182276055944 ) ) ;
#24808 = CARTESIAN_POINT ( 'NONE',  ( 0.2764337282391428618, -1.207704344519209938, -0.5166151207188711680 ) ) ;
#24810 = CARTESIAN_POINT ( 'NONE',  ( 0.01128677947712186484, -0.9461986806730106059, 0.1457185332388702959 ) ) ;
#24809 = CARTESIAN_POINT ( 'NONE',  ( 0.04285534776242382049, 0.4878382857517603588, 0.08280911155782964828 ) ) ;
#24811 = CARTESIAN_POINT ( 'NONE',  ( 0.02953079040095420854, -0.3810518745593896028, -0.3687679460475819515 ) ) ;
#24812 = ORIENTED_EDGE ( 'NONE', *, *, #13480, .F. ) ;
#24813 = CARTESIAN_POINT ( 'NONE',  ( -0.1574377185082707353, 0.4885537809602767401, 0.1000000000000000194 ) ) ;
#24814 = VERTEX_POINT ( 'NONE', #6261 ) ;
#24815 = DIRECTION ( 'NONE',  ( -1.000000000000000000, -0.000000000000000000, -0.000000000000000000 ) ) ;
#24816 = CARTESIAN_POINT ( 'NONE',  ( 0.1328749367006503146, -0.7849577211208300653, 0.6191913765737894204 ) ) ;
#24818 = CARTESIAN_POINT ( 'NONE',  ( 0.5771924405437491856, -1.609115206908811047, 0.4469232899498119527 ) ) ;
#24817 = CARTESIAN_POINT ( 'NONE',  ( -0.05283710938260965245, -0.4315340639268090972, 0.1819215676045965735 ) ) ;
#24819 = DIRECTION ( 'NONE',  ( 1.000000000000000000, 0.000000000000000000, 0.000000000000000000 ) ) ;
#24820 = CARTESIAN_POINT ( 'NONE',  ( 0.3234194364778873454, -1.642295127928019793, -0.6168578883319564277 ) ) ;
#24821 = CARTESIAN_POINT ( 'NONE',  ( 0.05999999999999990757, -0.02383748379410547888, -0.1985743547550029575 ) ) ;
#24822 = CARTESIAN_POINT ( 'NONE',  ( 0.1963639982240613369, -1.999069888237751780, -0.2881341410394136493 ) ) ;
#24823 = CARTESIAN_POINT ( 'NONE',  ( 0.1822190496678027793, -0.7502263017545820478, 0.5606200488576618124 ) ) ;
#24824 = CARTESIAN_POINT ( 'NONE',  ( 0.4446621238095426754, -1.684612092570755726, 0.4299412632484984620 ) ) ;
#24825 = DIRECTION ( 'NONE',  ( 7.771561172376107616E-16, -7.170354002788761615E-17, 1.000000000000000000 ) ) ;
#24826 = EDGE_CURVE ( 'NONE', #24994, #37890, #11431, .T. ) ;
#24827 = ORIENTED_EDGE ( 'NONE', *, *, #29544, .T. ) ;
#24828 = CARTESIAN_POINT ( 'NONE',  ( 0.08058916068514494768, -1.309220013881624123, 0.4727703015479320370 ) ) ;
#24829 = CARTESIAN_POINT ( 'NONE',  ( 0.5908959048872451936, -1.601544548465861695, 0.4282886817583847483 ) ) ;
#24830 = ADVANCED_FACE ( 'NONE', ( #21919 ), #36162, .F. ) ;
#24831 = CARTESIAN_POINT ( 'NONE',  ( -0.2746410161513779258, -2.416006048095809877, -1.059240699271965402 ) ) ;
#24832 = DIRECTION ( 'NONE',  ( -1.000000000000000000, -2.341930812374887555E-31, 1.664003471950578127E-31 ) ) ;
#24833 = ADVANCED_FACE ( 'NONE', ( #15722 ), #28294, .T. ) ;
#24834 = CARTESIAN_POINT ( 'NONE',  ( 0.4224057990199354684, -0.9849677903659747047, 0.8092447908785728172 ) ) ;
#24835 = CARTESIAN_POINT ( 'NONE',  ( -0.03672309138970067388, 0.2485858928251931943, 0.4115746274616670641 ) ) ;
#24836 = CARTESIAN_POINT ( 'NONE',  ( 0.01259362679367681710, -0.9548954960245769064, 0.3190520231937701845 ) ) ;
#24837 = CARTESIAN_POINT ( 'NONE',  ( 0.6355919355275447824, -1.485218526194229005, -0.3957663088022824738 ) ) ;
#24838 = CARTESIAN_POINT ( 'NONE',  ( 0.01548846960706657880, 0.2450655194479920418, 0.4674710490749448555 ) ) ;
#24839 = DIRECTION ( 'NONE',  ( 0.000000000000000000, 0.6595282642760672553, 0.7516797646744243222 ) ) ;
#24840 = DIRECTION ( 'NONE',  ( -1.000000000000000000, -7.857794173099924470E-32, -8.628166150854818811E-32 ) ) ;
#24841 = CARTESIAN_POINT ( 'NONE',  ( 0.1909286924077255032, -1.257064795538239022, -0.3194753470178354759 ) ) ;
#24842 = EDGE_CURVE ( 'NONE', #7197, #10109, #23059, .T. ) ;
#24843 = EDGE_LOOP ( 'NONE', ( #1183, #8786, #5949, #32819, #25620 ) ) ;
#24844 = DIRECTION ( 'NONE',  ( 0.000000000000000000, 0.5877852522924756906, 0.8090169943749454529 ) ) ;
#24845 = CARTESIAN_POINT ( 'NONE',  ( 0.4089074357954356476, -1.710833460744737078, -0.6076181741210081588 ) ) ;
#24846 = ADVANCED_FACE ( 'NONE', ( #28689 ), #10553, .T. ) ;
#24847 = CARTESIAN_POINT ( 'NONE',  ( 0.6623769754396896525, -1.516903808842391177, 0.4182417262808777458 ) ) ;
#24848 = CARTESIAN_POINT ( 'NONE',  ( 0.5542431180310618544, -1.624464136724068419, -0.4644229827488332574 ) ) ;
#24849 = CARTESIAN_POINT ( 'NONE',  ( 0.3992403239432265050, -1.683235622436123125, -0.6263438071736147084 ) ) ;
#24850 = EDGE_CURVE ( 'NONE', #3583, #394, #2025, .T. ) ;
#24851 = ORIENTED_EDGE ( 'NONE', *, *, #34825, .T. ) ;
#24852 = CARTESIAN_POINT ( 'NONE',  ( 0.4867251962510779073, -1.680960026995275802, -0.6125153944540090434 ) ) ;
#24853 = CARTESIAN_POINT ( 'NONE',  ( 0.3968636464328635372, -1.134397982594676613, 0.6056963140804544343 ) ) ;
#24854 = CARTESIAN_POINT ( 'NONE',  ( -0.05464101615137761936, -1.906060000575976021, -0.2916525572568466340 ) ) ;
#24855 = CARTESIAN_POINT ( 'NONE',  ( 0.04047043078435860058, 0.3430608037303070068, -0.3654822131371353033 ) ) ;
#24856 = CARTESIAN_POINT ( 'NONE',  ( 0.4151592125368772646, -1.168422792391130116, 0.7279282713727704968 ) ) ;
#24858 = CARTESIAN_POINT ( 'NONE',  ( 0.4517786694993131680, -1.612323574982035712, -0.6578841968208716251 ) ) ;
#24857 = DIRECTION ( 'NONE',  ( 1.000000000000000000, 2.280301054154495132E-31, -1.664003471950577689E-31 ) ) ;
#24859 = CARTESIAN_POINT ( 'NONE',  ( 0.2246580631734754474, -0.8968525156641222740, 0.4249663362035034364 ) ) ;
#24860 = VERTEX_POINT ( 'NONE', #6046 ) ;
#24861 = CALENDAR_DATE ( 2026, 13, 10 ) ;
#24862 = AXIS2_PLACEMENT_3D ( 'NONE', #36172, #39268, #23465 ) ;
#24863 = CARTESIAN_POINT ( 'NONE',  ( -2.567390744445674500E-16, 1.219177958431796432E-16, -0.1849999999999994982 ) ) ;
#24864 = ORIENTED_EDGE ( 'NONE', *, *, #19319, .F. ) ;
#24865 = ORIENTED_EDGE ( 'NONE', *, *, #27552, .F. ) ;
#24866 = CARTESIAN_POINT ( 'NONE',  ( 0.3857633994507903008, -1.605746613796385391, 0.5814654401004829554 ) ) ;
#24868 = CARTESIAN_POINT ( 'NONE',  ( 0.1750730331674688889, -0.8628421928542436836, -0.003741419850515158470 ) ) ;
#24867 = CYLINDRICAL_SURFACE ( 'NONE', #25295, 0.01500000000000005669 ) ;
#24869 = DIRECTION ( 'NONE',  ( 0.4999551463232371762, -0.8660512985181134660, 0.000000000000000000 ) ) ;
#24870 = VERTEX_POINT ( 'NONE', #741 ) ;
#24871 = ORIENTED_EDGE ( 'NONE', *, *, #3444, .F. ) ;
#24872 = CARTESIAN_POINT ( 'NONE',  ( 0.3960837959415427489, -1.111483722700696397, 0.6223813603130625705 ) ) ;
#24873 = CARTESIAN_POINT ( 'NONE',  ( 0.1303976270792735204, -0.6539453279429289223, 0.4317581259434655760 ) ) ;
#24874 = ORIENTED_EDGE ( 'NONE', *, *, #35628, .F. ) ;
#24875 = CARTESIAN_POINT ( 'NONE',  ( 0.2049227550019952493, -1.874964159105817485, -0.3434029161829166843 ) ) ;
#24876 = CARTESIAN_POINT ( 'NONE',  ( 0.4409062655693438137, -1.690090444797295977, -0.7462941026102624109 ) ) ;
#24877 = CARTESIAN_POINT ( 'NONE',  ( 0.05999999999999990757, -0.2940959072101921867, -0.05922497245433272495 ) ) ;
#24878 = EDGE_CURVE ( 'NONE', #8354, #3740, #732, .T. ) ;
#24879 = CARTESIAN_POINT ( 'NONE',  ( -0.1044436713285783330, -0.4741860147766016054, 0.3606502365330791493 ) ) ;
#24880 = ADVANCED_FACE ( 'NONE', ( #19634 ), #37967, .F. ) ;
#24881 = CARTESIAN_POINT ( 'NONE',  ( 0.1637585665034339832, -0.5994899851647166322, 0.1022936816274461203 ) ) ;
#24882 = DIRECTION ( 'NONE',  ( -0.2681551574199820265, -0.1548009352265700411, -0.9508572353419014744 ) ) ;
#24883 = CARTESIAN_POINT ( 'NONE',  ( -0.1142670043590668788, -0.4723146173917492918, 0.3382895567580816443 ) ) ;
#24884 = CARTESIAN_POINT ( 'NONE',  ( 0.4206426192640880246, -1.125420795136339747, 0.5391101744456719969 ) ) ;
#24885 = CARTESIAN_POINT ( 'NONE',  ( 0.0003547581337898165674, -0.9504652791025145486, 0.2394745140284491591 ) ) ;
#24886 = COORDINATED_UNIVERSAL_TIME_OFFSET ( 0, 0, .AHEAD. ) ;
#24887 = CARTESIAN_POINT ( 'NONE',  ( 0.1991581284650917050, -0.9215239498232444815, 0.3071336240427082753 ) ) ;
#24888 = CARTESIAN_POINT ( 'NONE',  ( 0.4312022151739950404, -1.138629288109622273, 0.4375280249474818306 ) ) ;
#24889 = CARTESIAN_POINT ( 'NONE',  ( 0.5465277059400872606, -1.167200690009414510, 0.5856983068965131434 ) ) ;
#24890 = DIRECTION ( 'NONE',  ( 0.000000000000000000, 0.9510565162951414298, -0.3090169943749848658 ) ) ;
#24891 = CARTESIAN_POINT ( 'NONE',  ( -0.002783323111321702164, -0.8122190247268278318, 0.2436509486217987297 ) ) ;
#24892 = CARTESIAN_POINT ( 'NONE',  ( -0.02953079040095693900, -0.3810518745593846068, 0.3687679460475796756 ) ) ;
#24893 = CARTESIAN_POINT ( 'NONE',  ( 0.2198247498919005116, -1.608236751325475167, -0.6963561265924880228 ) ) ;
#24894 = CARTESIAN_POINT ( 'NONE',  ( 0.1909286924077256420, -1.257064795538239244, -0.2869361388274796476 ) ) ;
#24895 = ADVANCED_FACE ( 'NONE', ( #32771 ), #8575, .T. ) ;
#24896 = ORIENTED_EDGE ( 'NONE', *, *, #1491, .T. ) ;
#24897 = ORIENTED_EDGE ( 'NONE', *, *, #30569, .F. ) ;
#24898 = CARTESIAN_POINT ( 'NONE',  ( -0.1129900121204040209, -0.5167580615069109484, 0.1415474730881046972 ) ) ;
#24899 = ORIENTED_EDGE ( 'NONE', *, *, #35019, .F. ) ;
#24900 = LINE ( 'NONE', #21420, #20413 ) ;
#24901 = CARTESIAN_POINT ( 'NONE',  ( 0.1999999999999794720, -2.107936428766273629, -0.2870436526301871627 ) ) ;
#24902 = CARTESIAN_POINT ( 'NONE',  ( -0.02000000000000000042, -2.183180860297908144, -0.3917586832283071474 ) ) ;
#24904 = VERTEX_POINT ( 'NONE', #949 ) ;
#24903 = CARTESIAN_POINT ( 'NONE',  ( 0.03113248654051816583, 0.6304109427692223822, -0.1442409525262416947 ) ) ;
#24905 = EDGE_LOOP ( 'NONE', ( #8094, #39874, #6222, #12404 ) ) ;
#24906 = CARTESIAN_POINT ( 'NONE',  ( 0.04154009738085467918, 0.4416556227939101298, -0.1617111092119887517 ) ) ;
#24907 = ORIENTED_EDGE ( 'NONE', *, *, #39307, .T. ) ;
#24908 = CARTESIAN_POINT ( 'NONE',  ( 0.2407897211441908936, -1.453152299343511755, 0.9165384340539985963 ) ) ;
#24910 = CARTESIAN_POINT ( 'NONE',  ( 0.1100434532894998957, -1.277816772219506625, 0.6166110354182127162 ) ) ;
#24909 = CARTESIAN_POINT ( 'NONE',  ( 0.1221059964993554542, -0.8717596041297476228, 0.5005114288050678262 ) ) ;
#24911 = DIRECTION ( 'NONE',  ( 2.465190328815661892E-32, 1.000000000000000000, -5.978086547377980964E-31 ) ) ;
#24912 = CARTESIAN_POINT ( 'NONE',  ( 0.4026370839150480996, -1.708716391613833041, 0.4182417262808775793 ) ) ;
#24914 = EDGE_LOOP ( 'NONE', ( #135, #38445, #23125, #14465 ) ) ;
#24913 = VERTEX_POINT ( 'NONE', #17145 ) ;
#24915 = LINE ( 'NONE', #28399, #2076 ) ;
#24916 = CARTESIAN_POINT ( 'NONE',  ( 0.3555645034559717366, -1.742873732338575898, 0.4378062404383618045 ) ) ;
#24917 = CARTESIAN_POINT ( 'NONE',  ( -0.03170752374382796585, -0.4816921673044493590, 0.09938322573836505525 ) ) ;
#24918 = CARTESIAN_POINT ( 'NONE',  ( 0.3202064935259268941, -1.032063384080334822, 0.7518809291558405938 ) ) ;
#24919 = CARTESIAN_POINT ( 'NONE',  ( 0.1874578000378240850, -0.6893444085712847613, 0.06304793604024336307 ) ) ;
#24920 = EDGE_CURVE ( 'NONE', #11635, #1766, #24367, .T. ) ;
#24921 = CARTESIAN_POINT ( 'NONE',  ( 0.01226325382937903420, -0.4335986999190264979, 0.2007874243352632537 ) ) ;
#24922 = CARTESIAN_POINT ( 'NONE',  ( 0.4650292090997563133, -1.068238633521630732, -0.4213092890091242881 ) ) ;
#24923 = CARTESIAN_POINT ( 'NONE',  ( 0.7472694261237929902, -1.513267490863592135, 0.4687417262808789009 ) ) ;
#24924 = CARTESIAN_POINT ( 'NONE',  ( 0.1850349610749611740, -0.7952146172061540508, 0.1457185332388699905 ) ) ;
#24925 = CARTESIAN_POINT ( 'NONE',  ( 0.1850841550199354701, -0.8515884040318244530, 0.1812164098636643572 ) ) ;
#24926 = DIRECTION ( 'NONE',  ( 0.9999999999999998890, -5.551115123125783935E-17, -5.551115123125785167E-17 ) ) ;
#24927 = DIRECTION ( 'NONE',  ( 0.000000000000000000, -0.3420201433256721546, 0.9396926207859070956 ) ) ;
#24928 = CARTESIAN_POINT ( 'NONE',  ( 0.0003038568743942667081, -0.4444331504931744448, 0.2553847410507332771 ) ) ;
#24929 = CARTESIAN_POINT ( 'NONE',  ( 0.08174454493327279470, -1.241495247832560489, 0.7557354517501940760 ) ) ;
#24930 = DATE_TIME_ROLE ( 'classification_date' ) ;
#24931 = CARTESIAN_POINT ( 'NONE',  ( 0.6491914112794352487, -1.351404041023776204, 0.8153926641961858346 ) ) ;
#24932 = CARTESIAN_POINT ( 'NONE',  ( -0.02953079040095689042, 0.5250338024619264354, 0.07436286310882508910 ) ) ;
#24933 = DIRECTION ( 'NONE',  ( 0.8660512985181134660, 0.4999551463232372317, 0.000000000000000000 ) ) ;
#24934 = CARTESIAN_POINT ( 'NONE',  ( 0.04293317454820651941, -0.3457449726441599314, 0.3536934093827153180 ) ) ;
#24935 = CARTESIAN_POINT ( 'NONE',  ( 2.567413883183506493E-16, -0.03000000000000006481, 0.1699999999999995404 ) ) ;
#24936 = EDGE_LOOP ( 'NONE', ( #30101, #18903, #23847, #1448 ) ) ;
#24937 = DIRECTION ( 'NONE',  ( 0.000000000000000000, 0.000000000000000000, 1.000000000000000000 ) ) ;
#24938 = CARTESIAN_POINT ( 'NONE',  ( 0.2454656089401869856, -1.560133056456860290, 0.8800177669848034956 ) ) ;
#24939 = CARTESIAN_POINT ( 'NONE',  ( 0.5878865232721811607, -1.491222718801129776, 0.5725363768365727690 ) ) ;
#24940 = EDGE_CURVE ( 'NONE', #26277, #19589, #32221, .T. ) ;
#24942 = ORIENTED_EDGE ( 'NONE', *, *, #20367, .F. ) ;
#24941 = DIRECTION ( 'NONE',  ( 0.000000000000000000, -0.3882559824134196313, 0.9215515678030125057 ) ) ;
#24943 = CARTESIAN_POINT ( 'NONE',  ( 0.1876168051218740918, -0.6873969840233377093, 0.1659352930446481023 ) ) ;
#24945 = ORIENTED_EDGE ( 'NONE', *, *, #35574, .F. ) ;
#24944 = ORIENTED_EDGE ( 'NONE', *, *, #904, .F. ) ;
#24946 = CARTESIAN_POINT ( 'NONE',  ( 0.3539056426437465763, -0.9003241868202508380, 0.7035817311501109117 ) ) ;
#24947 = CARTESIAN_POINT ( 'NONE',  ( 0.1856533569311497323, -0.7573055082216308964, 0.1457185332388697685 ) ) ;
#24948 = DIRECTION ( 'NONE',  ( -7.000205099780314469E-17, -1.000000000000000000, 6.590151126658399604E-16 ) ) ;
#24949 = CONTEXT_DEPENDENT_SHAPE_REPRESENTATION ( #10874, #23278 ) ;
#24950 = CARTESIAN_POINT ( 'NONE',  ( 0.3100229871264634229, -1.765619355789175282, 0.5593676469398397577 ) ) ;
#24951 = ORIENTED_EDGE ( 'NONE', *, *, #16543, .T. ) ;
#24952 = CARTESIAN_POINT ( 'NONE',  ( 0.2533938263156997883, -0.9611212520725127550, 0.6837618949440756877 ) ) ;
#24953 = CARTESIAN_POINT ( 'NONE',  ( 0.3245437662617405850, -1.759079744317569860, 0.6570495871072389305 ) ) ;
#24954 = CARTESIAN_POINT ( 'NONE',  ( 0.4817671749021297245, -1.450000170275026479, 0.7905690555072178993 ) ) ;
#24955 = CARTESIAN_POINT ( 'NONE',  ( 0.3165945761936767022, -1.762959260158723840, 0.5320016251091660431 ) ) ;
#24956 = CARTESIAN_POINT ( 'NONE',  ( -0.1684323896976702706, 0.5231977508182777958, 0.1451849067762199241 ) ) ;
#24957 = VERTEX_POINT ( 'NONE', #13842 ) ;
#24958 = CARTESIAN_POINT ( 'NONE',  ( 0.4189016656849444686, -1.713998620513816018, 0.6094645527338905522 ) ) ;
#24959 = CARTESIAN_POINT ( 'NONE',  ( 0.7359799699820096519, -1.496616301705748997, 0.6950498515647415276 ) ) ;
#24960 = CARTESIAN_POINT ( 'NONE',  ( 0.1163334220414616871, -1.415481480104449741, 0.5683323772858765999 ) ) ;
#24961 = CARTESIAN_POINT ( 'NONE',  ( 0.4093192649698301211, -1.477391824278449395, -0.4706793243405929528 ) ) ;
#24962 = LINE ( 'NONE', #22302, #14855 ) ;
#24963 = FACE_OUTER_BOUND ( 'NONE', #36485, .T. ) ;
#24964 = CARTESIAN_POINT ( 'NONE',  ( 0.002346242718065488699, -0.9632443647534850717, 0.3631189922238501344 ) ) ;
#24965 = CARTESIAN_POINT ( 'NONE',  ( 0.5463261744266250108, -1.174184195093048277, 0.6317594707774240037 ) ) ;
#24966 = SECURITY_CLASSIFICATION_LEVEL ( 'unclassified' ) ;
#24967 = FACE_OUTER_BOUND ( 'NONE', #40144, .T. ) ;
#24968 = CARTESIAN_POINT ( 'NONE',  ( 0.3947704391985938921, -1.713677448712424445, 0.4185425205145197336 ) ) ;
#24969 = CARTESIAN_POINT ( 'NONE',  ( -0.05489899477340599854, -0.02536133381296585068, 0.4620560448753001093 ) ) ;
#24970 = EDGE_LOOP ( 'NONE', ( #11820, #12033 ) ) ;
#24971 = CARTESIAN_POINT ( 'NONE',  ( 0.4673214953140302219, -1.236749788148563400, 0.6057417262809804415 ) ) ;
#24972 = LINE ( 'NONE', #15315, #13234 ) ;
#24973 = VECTOR ( 'NONE', #22371, 39.37007874015748143 ) ;
#24974 = CARTESIAN_POINT ( 'NONE',  ( -2.070754768975509474, -0.09959325338431662678, 0.3602693341844405150 ) ) ;
#24975 = ORIENTED_EDGE ( 'NONE', *, *, #30010, .T. ) ;
#24976 = CARTESIAN_POINT ( 'NONE',  ( -0.03174036153405046523, 0.07585545617081057568, -0.5190446117378511026 ) ) ;
#24977 = EDGE_CURVE ( 'NONE', #12681, #38249, #25645, .T. ) ;
#24978 = CARTESIAN_POINT ( 'NONE',  ( -0.01318839431724684423, -0.8581597300867446210, 0.3276449317425384478 ) ) ;
#24980 = VERTEX_POINT ( 'NONE', #7254 ) ;
#24979 = ORIENTED_EDGE ( 'NONE', *, *, #37059, .T. ) ;
#24981 = EDGE_CURVE ( 'NONE', #13737, #1061, #10930, .T. ) ;
#24982 = DIRECTION ( 'NONE',  ( -1.000000000000000000, 0.000000000000000000, 0.000000000000000000 ) ) ;
#24983 = CONICAL_SURFACE ( 'NONE', #4604, 0.1599999999999999201, 1.047197551196601850 ) ;
#24984 = DIRECTION ( 'NONE',  ( 0.000000000000000000, 0.000000000000000000, -1.000000000000000000 ) ) ;
#24985 = CARTESIAN_POINT ( 'NONE',  ( 0.3625773210575073957, -1.777458267349059540, -0.3444665025425360239 ) ) ;
#24986 = ADVANCED_FACE ( 'NONE', ( #29301, #1753 ), #38338, .T. ) ;
#24987 = CARTESIAN_POINT ( 'NONE',  ( 0.3782534879241810644, -1.123019940516551740, 0.6966012497027646022 ) ) ;
#24989 = CARTESIAN_POINT ( 'NONE',  ( 0.2325938614944302874, -1.347997356825076487, 0.5182417262812506475 ) ) ;
#24988 = CARTESIAN_POINT ( 'NONE',  ( 0.03674260963082216086, 0.4430101671189279333, 0.1867880763203807470 ) ) ;
#24990 = CARTESIAN_POINT ( 'NONE',  ( 0.05279905671744909018, -0.2420693533014104115, -0.4010177630757500444 ) ) ;
#24991 = ORIENTED_EDGE ( 'NONE', *, *, #30152, .T. ) ;
#24992 = EDGE_CURVE ( 'NONE', #35807, #17948, #19754, .T. ) ;
#24993 = CARTESIAN_POINT ( 'NONE',  ( 0.09191803790759442427, -0.5734812623173219936, 0.2369789867951458406 ) ) ;
#24994 = VERTEX_POINT ( 'NONE', #1335 ) ;
#24995 = CARTESIAN_POINT ( 'NONE',  ( 0.7053080889764471451, -1.513942001867420339, 0.5667347313869608438 ) ) ;
#24996 = CARTESIAN_POINT ( 'NONE',  ( 0.4143629965670120319, -1.443116486983128111, 0.8306079842001903302 ) ) ;
#24998 = CARTESIAN_POINT ( 'NONE',  ( 0.5856637561180031426, -1.604417808857893535, 0.4379681301762496926 ) ) ;
#24997 = DIRECTION ( 'NONE',  ( -0.8662449985352328463, -0.4996194577002526782, 4.774657901377541008E-15 ) ) ;
#24999 = DIRECTION ( 'NONE',  ( 1.000000000000000000, 7.250402404269733157E-14, -8.188689774234050758E-16 ) ) ;
#25000 = CARTESIAN_POINT ( 'NONE',  ( 0.3634081991604131701, -1.011642316747166870, 0.6166164155041838901 ) ) ;
#25001 = ORIENTED_EDGE ( 'NONE', *, *, #28244, .F. ) ;
#25002 = CARTESIAN_POINT ( 'NONE',  ( 0.1175254897578254243, -1.414866947670519570, 0.5260415310556526558 ) ) ;
#25003 = CARTESIAN_POINT ( 'NONE',  ( 0.1887433770899517860, -0.4595573870411951978, 0.1492066213800052610 ) ) ;
#25004 = CARTESIAN_POINT ( 'NONE',  ( 0.1319611972603651762, -0.6045625464573930463, 0.3271665123075399584 ) ) ;
#25005 = CARTESIAN_POINT ( 'NONE',  ( 0.4452565618721048835, -1.695813388727355653, 0.4387187260761371554 ) ) ;
#25006 = CARTESIAN_POINT ( 'NONE',  ( -0.02953079040095603694, 0.3810518745593876599, -0.3687679460475788429 ) ) ;
#25007 = EDGE_CURVE ( 'NONE', #16107, #8744, #21049, .T. ) ;
#25008 = CARTESIAN_POINT ( 'NONE',  ( 0.1499999999999993561, -0.3772621329472632401, 0.3651003739303507190 ) ) ;
#25009 = PRODUCT_RELATED_PRODUCT_CATEGORY ( 'detail', '', ( #3852 ) ) ;
#25010 = DIRECTION ( 'NONE',  ( 0.000000000000000000, 0.7516797646744247663, -0.6595282642760668113 ) ) ;
#25011 = AXIS2_PLACEMENT_3D ( 'NONE', #4434, #993, #26868 ) ;
#25012 = PLANE ( 'NONE',  #5574 ) ;
#25013 = CARTESIAN_POINT ( 'NONE',  ( 0.2335251464432007984, -1.232233318504470043, 0.5010574213731815441 ) ) ;
#25014 = CARTESIAN_POINT ( 'NONE',  ( 0.2791332027808016703, -0.7342173681784933681, 0.6310308052199803397 ) ) ;
#25015 = VECTOR ( 'NONE', #35970, 39.37007874015748143 ) ;
#25016 = CARTESIAN_POINT ( 'NONE',  ( -0.05615703521554987060, 0.2616264896058755340, 0.3776298641847850579 ) ) ;
#25017 = CARTESIAN_POINT ( 'NONE',  ( 0.05037753678752365100, -1.191647567912915040, 0.6657367322637173235 ) ) ;
#25018 = AXIS2_PLACEMENT_3D ( 'NONE', #36732, #21715, #6273 ) ;
#25019 = CARTESIAN_POINT ( 'NONE',  ( 0.6213533671482026621, -1.618071575169615306, -0.4781682850753038450 ) ) ;
#25020 = FACE_OUTER_BOUND ( 'NONE', #15933, .T. ) ;
#25021 = CARTESIAN_POINT ( 'NONE',  ( 0.1263930849240390564, -0.8569068895757016024, 0.4518561175853242906 ) ) ;
#25022 = CARTESIAN_POINT ( 'NONE',  ( 0.2631236827724738325, -1.677172619524047947, 0.5509572661685944173 ) ) ;
#25023 = DIRECTION ( 'NONE',  ( 0.8660512985181130219, 0.4999551463232378978, 0.000000000000000000 ) ) ;
#25024 = ORIENTED_EDGE ( 'NONE', *, *, #19843, .F. ) ;
#25025 = DIRECTION ( 'NONE',  ( 0.4999551463232372317, -0.8660512985181134660, 0.000000000000000000 ) ) ;
#25026 = CARTESIAN_POINT ( 'NONE',  ( 0.4415664673242307714, -1.208588400238274740, 0.7960777065921241791 ) ) ;
#25027 = CARTESIAN_POINT ( 'NONE',  ( 0.3623340787431935106, -1.967984212679734446, -0.5065714937396946782 ) ) ;
#25028 = DIRECTION ( 'NONE',  ( -1.000000000000000000, 0.000000000000000000, 0.000000000000000000 ) ) ;
#25029 = ORIENTED_EDGE ( 'NONE', *, *, #19055, .F. ) ;
#25030 = ADVANCED_FACE ( 'NONE', ( #27439 ), #35508, .T. ) ;
#25031 = CARTESIAN_POINT ( 'NONE',  ( -0.1450923023275428325, -0.5230583524816332375, 0.3181161673586312411 ) ) ;
#25032 = CARTESIAN_POINT ( 'NONE',  ( 0.1514213231021494244, -1.394936281994370697, 0.5181495499691263218 ) ) ;
#25033 = CARTESIAN_POINT ( 'NONE',  ( 0.3249649890265327024, -1.766762640835898290, 0.5057684568561345850 ) ) ;
#25034 = FACE_OUTER_BOUND ( 'NONE', #35550, .T. ) ;
#25035 = EDGE_CURVE ( 'NONE', #2123, #13011, #15164, .T. ) ;
#25036 = CARTESIAN_POINT ( 'NONE',  ( 0.4901888945983902679, -1.275704295442520397, 0.6511736332760663659 ) ) ;
#25037 = VECTOR ( 'NONE', #17460, 39.37007874015748854 ) ;
#25039 = FACE_OUTER_BOUND ( 'NONE', #1282, .T. ) ;
#25038 = FACE_OUTER_BOUND ( 'NONE', #18309, .T. ) ;
#25040 = B_SPLINE_CURVE_WITH_KNOTS ( 'NONE', 3,
 ( #14102, #11821, #21095, #23783, #20291, #4614, #11427, #17602, #30343, #29955, #36302, #29733, #14714, #39210, #17395, #23996, #11031, #26867 ),
 .UNSPECIFIED., .F., .F.,
 ( 4, 2, 2, 2, 2, 2, 2, 2, 4 ),
 ( -0.003133633995111204627, -0.002350221109836722611, -0.001566808224562240811, -0.0007833953392877642148, 1.754598671259779974E-08, 0.0007834304312611898441, 0.001566843316535666657, 0.002350256201810143469, 0.003133669087084620282 ),
 .UNSPECIFIED. ) ;
#25041 = CARTESIAN_POINT ( 'NONE',  ( 0.1874346505856443745, -0.8710952576279675785, 0.2160754816401605771 ) ) ;
#25042 = VERTEX_POINT ( 'NONE', #8079 ) ;
#25043 = COORDINATED_UNIVERSAL_TIME_OFFSET ( 0, 0, .AHEAD. ) ;
#25044 = ADVANCED_FACE ( 'NONE', ( #24340 ), #39545, .T. ) ;
#25045 = CARTESIAN_POINT ( 'NONE',  ( 0.09473499835993481888, -1.365368924775509196, -0.3575598482871295558 ) ) ;
#25046 = VERTEX_POINT ( 'NONE', #2339 ) ;
#25047 = EDGE_LOOP ( 'NONE', ( #19232, #17450, #31600, #3384, #5591, #40517, #11725, #5402, #37594 ) ) ;
#25048 = AXIS2_PLACEMENT_3D ( 'NONE', #19830, #38740, #16757 ) ;
#25049 = CARTESIAN_POINT ( 'NONE',  ( 0.3135982152475476070, -1.415948938436505822, 0.8853364428893668592 ) ) ;
#25051 = CARTESIAN_POINT ( 'NONE',  ( 0.1137653586930576638, -0.5867251212695386853, -0.07337486296685742648 ) ) ;
#25050 = DIRECTION ( 'NONE',  ( 1.000000000000000000, 2.280301054154495132E-31, -1.664003471950577689E-31 ) ) ;
#25052 = CARTESIAN_POINT ( 'NONE',  ( 0.3595715536228106801, -1.625401886829162423, -0.3696110269036073093 ) ) ;
#25053 = CONICAL_SURFACE ( 'NONE', #40132, 0.4615209409081865166, 1.047197551196600740 ) ;
#25054 = ORIENTED_EDGE ( 'NONE', *, *, #20595, .T. ) ;
#25055 = CIRCLE ( 'NONE', #14528, 0.2500000000000000000 ) ;
#25056 = ORIENTED_EDGE ( 'NONE', *, *, #24266, .T. ) ;
#25057 = ORIENTED_EDGE ( 'NONE', *, *, #20060, .F. ) ;
#25058 = CARTESIAN_POINT ( 'NONE',  ( 0.4084715984908769415, -1.024951146690285642, 0.6323129096802421190 ) ) ;
#25059 = CARTESIAN_POINT ( 'NONE',  ( 0.4998774473189910861, -1.399813891400437216, 0.7994217634795599547 ) ) ;
#25060 = ORIENTED_EDGE ( 'NONE', *, *, #26320, .T. ) ;
#25061 = CARTESIAN_POINT ( 'NONE',  ( 0.1870184603604498619, -0.7197645011776521162, 0.03166985066965816165 ) ) ;
#25062 = CARTESIAN_POINT ( 'NONE',  ( 0.7059656540691128246, -1.571716619208481935, -0.5155029497116575543 ) ) ;
#25063 = CARTESIAN_POINT ( 'NONE',  ( 0.6089330441038812713, -1.477473485466218150, -0.6250000000000000000 ) ) ;
#25064 = ADVANCED_FACE ( 'NONE', ( #20655, #39963 ), #21259, .T. ) ;
#25065 = DIRECTION ( 'NONE',  ( -1.000000000000000000, -7.857794173099924470E-32, -8.628166150854818811E-32 ) ) ;
#25066 = CARTESIAN_POINT ( 'NONE',  ( -0.1142670043590667539, -0.4723146173917426860, 0.3382895567580836982 ) ) ;
#25067 = CIRCLE ( 'NONE', #7293, 0.08000000000000000167 ) ;
#25068 = LINE ( 'NONE', #34527, #7395 ) ;
#25069 = CARTESIAN_POINT ( 'NONE',  ( -0.2399999999999999079, -3.811657270145150989, -0.1642545796697100491 ) ) ;
#25070 = CARTESIAN_POINT ( 'NONE',  ( 0.07779920321647403048, -1.322114474344633583, 0.5682417262808776570 ) ) ;
#25071 = CARTESIAN_POINT ( 'NONE',  ( 0.1708500036367240627, -1.718699357903690439, -0.6511465918194946356 ) ) ;
#25072 = CARTESIAN_POINT ( 'NONE',  ( 0.3533584531583440214, -1.730880459003149907, -0.4486410610578602243 ) ) ;
#25073 = CALENDAR_DATE ( 2026, 13, 10 ) ;
#25074 = CIRCLE ( 'NONE', #21792, 0.07999999999999996003 ) ;
#25075 = CARTESIAN_POINT ( 'NONE',  ( 0.4903202831852248589, -1.081274614053407523, 0.5895842322316532380 ) ) ;
#25076 = CARTESIAN_POINT ( 'NONE',  ( -0.01548846960688968731, -0.2306506793135497668, -0.4716198300885139361 ) ) ;
#25077 = CARTESIAN_POINT ( 'NONE',  ( 0.4669205535706663635, -1.236249669535754103, 0.6057417262809816627 ) ) ;
#25078 = CARTESIAN_POINT ( 'NONE',  ( 0.5114126470110640366, -1.614748454822723556, -0.5166151207188711680 ) ) ;
#25079 = VECTOR ( 'NONE', #30468, 39.37007874015748854 ) ;
#25080 = AXIS2_PLACEMENT_3D ( 'NONE', #17851, #30411, #2242 ) ;
#25081 = CARTESIAN_POINT ( 'NONE',  ( -0.0004320282599767403219, -0.9107381779821550616, 0.3274798035714688860 ) ) ;
#25082 = CARTESIAN_POINT ( 'NONE',  ( 0.2615233978049238406, -1.678084768816710648, 0.5373352594323992371 ) ) ;
#25083 = AXIS2_PLACEMENT_3D ( 'NONE', #35913, #24145, #4016 ) ;
#25084 = FACE_OUTER_BOUND ( 'NONE', #16390, .T. ) ;
#25085 = CARTESIAN_POINT ( 'NONE',  ( 0.3771763907541850758, -1.752869764700489830, -0.5848310859449704635 ) ) ;
#25086 = EDGE_LOOP ( 'NONE', ( #4339, #4834, #16810, #26428 ) ) ;
#25087 = VERTEX_POINT ( 'NONE', #11784 ) ;
#25088 = CARTESIAN_POINT ( 'NONE',  ( 0.03113248654051816583, 0.5878163732725504298, -0.1704268771689479434 ) ) ;
#25089 = VERTEX_POINT ( 'NONE', #24552 ) ;
#25090 = CARTESIAN_POINT ( 'NONE',  ( -0.01548846960688914087, 0.2306506793135502942, 0.4716198300885117156 ) ) ;
#25091 = CARTESIAN_POINT ( 'NONE',  ( 0.01895494625228208441, 0.2428766181966295346, 0.4598657641708832067 ) ) ;
#25092 = EDGE_CURVE ( 'NONE', #16637, #33948, #6603, .T. ) ;
#25093 = CARTESIAN_POINT ( 'NONE',  ( 0.5328035064341107852, -1.351445797141976213, 0.7805622800820304352 ) ) ;
#25095 = ORIENTED_EDGE ( 'NONE', *, *, #35438, .F. ) ;
#25094 = CARTESIAN_POINT ( 'NONE',  ( 2.845524969047803358E-18, 1.562563540555661551E-17, 0.04249999999999995448 ) ) ;
#25096 = ORIENTED_EDGE ( 'NONE', *, *, #31101, .F. ) ;
#25097 = CARTESIAN_POINT ( 'NONE',  ( 0.5532309630114417009, -1.623494765793418670, 0.5182130042910411127 ) ) ;
#25098 = EDGE_LOOP ( 'NONE', ( #10363, #16871 ) ) ;
#25099 = CARTESIAN_POINT ( 'NONE',  ( 0.01228388642712701859, -0.5615114497096570512, 0.2760925587857833707 ) ) ;
#25101 = DIRECTION ( 'NONE',  ( -0.9877995450870419303, -0.03415031169247099291, 0.1519401689387651910 ) ) ;
#25100 = CARTESIAN_POINT ( 'NONE',  ( 0.3780826364363035208, -1.158814516788133409, 0.7205068528634307468 ) ) ;
#25102 = EDGE_CURVE ( 'NONE', #35001, #4931, #34965, .T. ) ;
#25103 = CARTESIAN_POINT ( 'NONE',  ( 0.3956641542645719656, -1.754140676906325469, -0.4988858376329875499 ) ) ;
#25104 = CALENDAR_DATE ( 2026, 13, 10 ) ;
#25105 = AXIS2_PLACEMENT_3D ( 'NONE', #10435, #19899, #1214 ) ;
#25106 = CARTESIAN_POINT ( 'NONE',  ( 0.4092767628406372982, -1.698388671139740680, 0.4182417262808776903 ) ) ;
#25108 = EDGE_LOOP ( 'NONE', ( #40316, #39616, #12107, #38891 ) ) ;
#25107 = ORIENTED_EDGE ( 'NONE', *, *, #21504, .T. ) ;
#25109 = CARTESIAN_POINT ( 'NONE',  ( 0.4661081799873099119, -1.093130792299548570, -0.4039132814442666364 ) ) ;
#25110 = FACE_OUTER_BOUND ( 'NONE', #37534, .T. ) ;
#25111 = CARTESIAN_POINT ( 'NONE',  ( -0.3000000000000000999, -4.233163482269810096, -0.5148221395285308422 ) ) ;
#25112 = CARTESIAN_POINT ( 'NONE',  ( 0.2042467818395008738, -0.8389012776653698156, 0.6553572424280913467 ) ) ;
#25113 = VECTOR ( 'NONE', #1895, 39.37007874015748143 ) ;
#25114 =( BOUNDED_SURFACE ( )  B_SPLINE_SURFACE ( 3, 2, ( 
 ( #30579, #5253, #21117 ),
 ( #12265, #5673, #2197 ),
 ( #21721, #30371, #21332 ),
 ( #36737, #12059, #15345 ),
 ( #27901, #40224, #34059 ),
 ( #27303, #28105, #24822 ),
 ( #15557, #8356, #27690 ),
 ( #18416, #18017, #11843 ),
 ( #33647, #40442, #40633 ),
 ( #20925, #2403, #17809 ),
 ( #2592, #33869, #3009 ),
 ( #24620, #37345, #39832 ),
 ( #24020, #37155, #36544 ),
 ( #11653, #24213, #8966 ),
 ( #9156, #30775, #18228 ),
 ( #21540, #34253, #8546 ),
 ( #5859, #2797, #6067 ),
 ( #40020, #5457, #18634 ),
 ( #14942, #27494, #24407 ),
 ( #36942, #34863, #154 ),
 ( #3805, #13268, #32183 ),
 ( #3607, #34465, #16361 ),
 ( #16174, #3197, #21939 ),
 ( #9773, #9359, #19650 ),
 ( #6476, #37963, #22346 ),
 ( #22759, #370, #3995 ),
 ( #16557, #6281, #25211 ),
 ( #9978, #37756, #19250 ) ),
 .UNSPECIFIED., .F., .F., .F. ) 
 B_SPLINE_SURFACE_WITH_KNOTS ( ( 4, 2, 2, 2, 2, 2, 2, 2, 2, 2, 2, 2, 2, 4 ),
 ( 3, 3 ),
 ( 0.03544507920328695411, 0.03595486840377590254, 0.03646465760426484404, 0.03748423600524272703, 0.03952339280719850689, 0.04156254960915428676, 0.04360170641111006662, 0.04462128481208795655, 0.04564086321306584648, 0.04768002001502162635, 0.04869959841599951628, 0.04971917681697740621, 0.05073875521795528920, 0.05175833361893317913 ),
 ( 0.000000000000000000, 1.000000000000000000 ),
 .UNSPECIFIED. ) 
 GEOMETRIC_REPRESENTATION_ITEM ( )  RATIONAL_B_SPLINE_SURFACE ( (
 ( 1.000000000000000000, 0.7061763356917282186, 1.000000000000000000),
 ( 1.000000000000000000, 0.7080421523057206512, 1.000000000000000000),
 ( 1.000000000000000000, 0.7088516299600281512, 1.000000000000000000),
 ( 1.000000000000000000, 0.7099244856010550331, 1.000000000000000000),
 ( 1.000000000000000000, 0.7101378557341009312, 1.000000000000000000),
 ( 1.000000000000000000, 0.7103445576143324613, 1.000000000000000000),
 ( 1.000000000000000000, 0.7098994762787452784, 1.000000000000000000),
 ( 1.000000000000000000, 0.7079279405282515869, 1.000000000000000000),
 ( 1.000000000000000000, 0.7057284653323193657, 1.000000000000000000),
 ( 1.000000000000000000, 0.7007157790496724159, 1.000000000000000000),
 ( 1.000000000000000000, 0.6978342510162854895, 1.000000000000000000),
 ( 1.000000000000000000, 0.6916754492645512675, 1.000000000000000000),
 ( 1.000000000000000000, 0.6883795134656507386, 1.000000000000000000),
 ( 1.000000000000000000, 0.6835032746938722870, 1.000000000000000000),
 ( 1.000000000000000000, 0.6818926907722926423, 1.000000000000000000),
 ( 1.000000000000000000, 0.6788412388327813574, 1.000000000000000000),
 ( 1.000000000000000000, 0.6773936298796078281, 1.000000000000000000),
 ( 1.000000000000000000, 0.6736810316134569376, 1.000000000000000000),
 ( 1.000000000000000000, 0.6720343155085293230, 1.000000000000000000),
 ( 1.000000000000000000, 0.6725111439841665595, 1.000000000000000000),
 ( 1.000000000000000000, 0.6731816333784569339, 1.000000000000000000),
 ( 1.000000000000000000, 0.6757599976965816824, 1.000000000000000000),
 ( 1.000000000000000000, 0.6776668555842312314, 1.000000000000000000),
 ( 1.000000000000000000, 0.6829223581645637031, 1.000000000000000000),
 ( 1.000000000000000000, 0.6862934035413942313, 1.000000000000000000),
 ( 1.000000000000000000, 0.6945721712650552160, 1.000000000000000000),
 ( 1.000000000000000000, 0.6994068901145212847, 1.000000000000000000),
 ( 1.000000000000000000, 0.7048795877316381686, 1.000000000000000000) ) ) 
 REPRESENTATION_ITEM ( '' )  SURFACE ( )  );
#25115 = AXIS2_PLACEMENT_3D ( 'NONE', #12170, #28013, #34584 ) ;
#25116 = CARTESIAN_POINT ( 'NONE',  ( 0.6984807982178791175, -1.438753897344778432, 0.5682417262808779901 ) ) ;
#25117 = CARTESIAN_POINT ( 'NONE',  ( 0.2731127878045417900, -1.644505663937311013, 0.7612257175765594353 ) ) ;
#25118 = EDGE_CURVE ( 'NONE', #18164, #26070, #34867, .T. ) ;
#25119 = AXIS2_PLACEMENT_3D ( 'NONE', #18831, #31375, #36918 ) ;
#25120 = CARTESIAN_POINT ( 'NONE',  ( 0.01524602687849146640, -0.4843663032112671130, 0.3577232613832507790 ) ) ;
#25121 = ADVANCED_FACE ( 'NONE', ( #30714 ), #38159, .F. ) ;
#25122 = DIRECTION ( 'NONE',  ( 1.000000000000000000, 6.779273404243070203E-32, 4.314083075427408311E-32 ) ) ;
#25123 = CARTESIAN_POINT ( 'NONE',  ( 0.4159916692016358830, -1.069406866067976081, -0.5155029497116575543 ) ) ;
#25124 = CARTESIAN_POINT ( 'NONE',  ( 0.1856533569311497323, -0.7573055082216308964, 0.1457185332388697685 ) ) ;
#25125 = LINE ( 'NONE', #2703, #416 ) ;
#25126 = CARTESIAN_POINT ( 'NONE',  ( 0.6007854161875070265, -1.040715339458748057, 0.000000000000000000 ) ) ;
#25127 = DIRECTION ( 'NONE',  ( 0.000000000000000000, 0.000000000000000000, 1.000000000000000000 ) ) ;
#25128 = CARTESIAN_POINT ( 'NONE',  ( 0.001298983775798597754, -0.4632363948272406606, 0.3098607539948510792 ) ) ;
#25129 = CARTESIAN_POINT ( 'NONE',  ( 0.09875757964952747159, -1.346375778014429425, 0.7038248674981169017 ) ) ;
#25130 = PERSON_AND_ORGANIZATION ( #28500, #32463 ) ;
#25131 = B_SPLINE_CURVE_WITH_KNOTS ( 'NONE', 3,
 ( #5571, #1505, #14231, #14019, #26594, #5158, #39132, #26796 ),
 .UNSPECIFIED., .F., .F.,
 ( 4, 2, 2, 4 ),
 ( 1.734723475976807094E-18, 0.0009467803671446852441, 0.001420170550717034155, 0.001893560734289383065 ),
 .UNSPECIFIED. ) ;
#25132 = CIRCLE ( 'NONE', #38271, 0.009999999999999986330 ) ;
#25133 = CARTESIAN_POINT ( 'NONE',  ( -0.05561375719525295941, 0.4316271021131496410, 0.1617018132803555996 ) ) ;
#25134 = DIRECTION ( 'NONE',  ( -0.4999551463232372317, 0.8660512985181135770, -0.000000000000000000 ) ) ;
#25135 = AXIS2_PLACEMENT_3D ( 'NONE', #2693, #12162, #24725 ) ;
#25136 = VECTOR ( 'NONE', #18380, 39.37007874015748143 ) ;
#25137 = DIRECTION ( 'NONE',  ( -0.8660254037844397068, 0.4607757839015044210, 0.1941279912067096214 ) ) ;
#25138 = EDGE_LOOP ( 'NONE', ( #28162, #898, #26637, #36686 ) ) ;
#25139 = CARTESIAN_POINT ( 'NONE',  ( 0.1053303053968787928, -1.411347232757804271, 0.5669086859767527020 ) ) ;
#25140 = CARTESIAN_POINT ( 'NONE',  ( 0.2248388864219118266, -1.477604057314256369, 0.9308881366616725828 ) ) ;
#25141 = CIRCLE ( 'NONE', #6064, 0.5302738246768090580 ) ;
#25142 = EDGE_CURVE ( 'NONE', #9243, #25380, #20866, .T. ) ;
#25143 = CARTESIAN_POINT ( 'NONE',  ( 0.5956979317618377179, -1.486985939769752241, 0.5919158884504209794 ) ) ;
#25145 = EDGE_LOOP ( 'NONE', ( #847, #3316, #28972, #10238 ) ) ;
#25144 = CARTESIAN_POINT ( 'NONE',  ( 0.4362155086522900849, -1.060665164869476929, 0.5182417262812423209 ) ) ;
#25146 = CARTESIAN_POINT ( 'NONE',  ( 0.5537997781288683807, -1.186498928682228504, 0.6031466697272260813 ) ) ;
#25148 = VERTEX_POINT ( 'NONE', #11378 ) ;
#25147 = EDGE_LOOP ( 'NONE', ( #38692, #19396, #26885, #31774 ) ) ;
#25149 = CARTESIAN_POINT ( 'NONE',  ( 0.6993646500685410938, -1.437698798162368341, 0.6034325323896145843 ) ) ;
#25150 = CARTESIAN_POINT ( 'NONE',  ( 0.3330378571917648745, -1.679292210583121170, -0.6251523164888654893 ) ) ;
#25151 = TOROIDAL_SURFACE ( 'NONE', #39610, 0.08830708661417323302, 0.01499999999999999944 ) ;
#25152 = LINE ( 'NONE', #3322, #25948 ) ;
#25153 = CALENDAR_DATE ( 2026, 13, 10 ) ;
#25154 = DIRECTION ( 'NONE',  ( 1.060606950627616897E-16, 6.122684696619992497E-17, 1.000000000000000000 ) ) ;
#25155 = ORIENTED_EDGE ( 'NONE', *, *, #33932, .T. ) ;
#25156 = CARTESIAN_POINT ( 'NONE',  ( 0.08659262626681933639, -0.7684511726617067051, 0.2033331541635994277 ) ) ;
#25157 = DIRECTION ( 'NONE',  ( 0.4999551463232372317, -0.8660512985181135770, 0.000000000000000000 ) ) ;
#25158 = CARTESIAN_POINT ( 'NONE',  ( 0.5250024315009472753, -1.526804064326204413, 0.5696525905436546910 ) ) ;
#25159 = CARTESIAN_POINT ( 'NONE',  ( 0.01548846960707528191, 0.3880410510314791783, 0.3755318131854940567 ) ) ;
#25160 = LINE ( 'NONE', #9523, #31687 ) ;
#25161 = ORIENTED_EDGE ( 'NONE', *, *, #21075, .F. ) ;
#25162 = VECTOR ( 'NONE', #18955, 39.37007874015748143 ) ;
#25163 = CARTESIAN_POINT ( 'NONE',  ( 0.1909286924077255032, -1.257064795538239022, -0.6184399470714002645 ) ) ;
#25164 = CARTESIAN_POINT ( 'NONE',  ( 0.7431085294082976356, -1.516429236334945196, 0.5637232355900747560 ) ) ;
#25165 = CARTESIAN_POINT ( 'NONE',  ( 0.000000000000000000, -0.2940959072101921867, -0.05922497245433272495 ) ) ;
#25166 = CARTESIAN_POINT ( 'NONE',  ( 0.6088915796500192767, -1.479003135906368227, 0.5701753227515949929 ) ) ;
#25167 = AXIS2_PLACEMENT_3D ( 'NONE', #25852, #38170, #10596 ) ;
#25168 = CARTESIAN_POINT ( 'NONE',  ( 0.05634307799789257248, -0.4332460723641358147, 0.1515798417490696048 ) ) ;
#25169 = VECTOR ( 'NONE', #22882, 39.37007874015748143 ) ;
#25170 = ADVANCED_FACE ( 'NONE', ( #5603 ), #2536, .F. ) ;
#25171 = CARTESIAN_POINT ( 'NONE',  ( 0.05579155178881651383, -1.335540925555324332, 0.3667417262808778111 ) ) ;
#25172 = DIRECTION ( 'NONE',  ( 0.000000000000000000, 0.000000000000000000, 1.000000000000000000 ) ) ;
#25173 = CARTESIAN_POINT ( 'NONE',  ( 0.04695358122948785351, -1.249483587492180581, 0.6552810377283075915 ) ) ;
#25174 = AXIS2_PLACEMENT_3D ( 'NONE', #36455, #17123, #17329 ) ;
#25175 = CARTESIAN_POINT ( 'NONE',  ( 0.3550363906115478474, -0.9559691138050746551, 0.6482402363088731745 ) ) ;
#25176 = PERSON_AND_ORGANIZATION_ROLE ( 'design_owner' ) ;
#25177 = CARTESIAN_POINT ( 'NONE',  ( 0.6409058204046232943, -1.459016202299332710, -0.5155029497116575543 ) ) ;
#25178 = ORIENTED_EDGE ( 'NONE', *, *, #28513, .F. ) ;
#25179 = CARTESIAN_POINT ( 'NONE',  ( -2.638061800623833890E-32, -3.491513147198974441E-33, 0.6114999999999938263 ) ) ;
#25180 = CARTESIAN_POINT ( 'NONE',  ( -0.05078493045284415697, 0.04880252970040156041, 0.4712186791567239408 ) ) ;
#25181 = EDGE_LOOP ( 'NONE', ( #8800, #6449, #17653, #4144 ) ) ;
#25182 = CARTESIAN_POINT ( 'NONE',  ( 0.4139939964727673005, -1.143890656390630367, 0.4261699876408763799 ) ) ;
#25183 = DIRECTION ( 'NONE',  ( 0.000000000000000000, 0.000000000000000000, -1.000000000000000000 ) ) ;
#25184 = CIRCLE ( 'NONE', #9439, 1.991674066779354213 ) ;
#25185 = CARTESIAN_POINT ( 'NONE',  ( 0.1911258005295297935, -0.8295430315077879646, 0.2652737953583465536 ) ) ;
#25186 = ORIENTED_EDGE ( 'NONE', *, *, #23528, .F. ) ;
#25187 = CARTESIAN_POINT ( 'NONE',  ( 0.2321526281619643584, -1.233007205928619232, 0.3667417262808778111 ) ) ;
#25188 = CARTESIAN_POINT ( 'NONE',  ( 0.007912233754840233141, -0.9669037819151463653, 0.6493826208389911203 ) ) ;
#25190 = ORIENTED_EDGE ( 'NONE', *, *, #31331, .F. ) ;
#25189 = VERTEX_POINT ( 'NONE', #30296 ) ;
#25191 = DIRECTION ( 'NONE',  ( 1.000000000000000000, 0.000000000000000000, 0.000000000000000000 ) ) ;
#25192 = AXIS2_PLACEMENT_3D ( 'NONE', #34685, #19061, #37773 ) ;
#25193 = AXIS2_PLACEMENT_3D ( 'NONE', #16034, #22022, #455 ) ;
#25194 = ORIENTED_EDGE ( 'NONE', *, *, #26247, .F. ) ;
#25195 = DIRECTION ( 'NONE',  ( 0.000000000000000000, 0.7516797646744242112, -0.6595282642760673664 ) ) ;
#25196 = CARTESIAN_POINT ( 'NONE',  ( -0.1533385355407297923, 0.4750492940987078860, 0.3599999999999995981 ) ) ;
#25198 = DIRECTION ( 'NONE',  ( 0.000000000000000000, 0.000000000000000000, -1.000000000000000000 ) ) ;
#25197 = CARTESIAN_POINT ( 'NONE',  ( 0.04308745346419525640, 0.4494111352305708018, 0.2058334250444144586 ) ) ;
#25199 = CARTESIAN_POINT ( 'NONE',  ( 0.04157143636675652426, -0.2900120080285103485, -0.3701876636500650575 ) ) ;
#25200 = VERTEX_POINT ( 'NONE', #2127 ) ;
#25201 = CARTESIAN_POINT ( 'NONE',  ( 0.09836942906952807208, -0.6323750885681652667, 0.3152165718758609958 ) ) ;
#25202 = ORIENTED_EDGE ( 'NONE', *, *, #23531, .F. ) ;
#25203 = VECTOR ( 'NONE', #24089, 39.37007874015748854 ) ;
#25204 = CARTESIAN_POINT ( 'NONE',  ( 0.05082294681498979866, 0.04864283519431678721, 0.4711332289091949566 ) ) ;
#25205 = CARTESIAN_POINT ( 'NONE',  ( 0.4416675145290221427, -1.573766806705525489, 0.5734788493934752651 ) ) ;
#25207 = DIRECTION ( 'NONE',  ( -1.000000000000000000, -2.280301054154495132E-31, 1.664003471950577689E-31 ) ) ;
#25206 = CARTESIAN_POINT ( 'NONE',  ( 0.5058599984363494340, -1.583313914148366752, -0.4933326546058601214 ) ) ;
#25208 = CARTESIAN_POINT ( 'NONE',  ( 0.06936654275873489761, -1.327133429011184917, 0.5458395137742713121 ) ) ;
#25209 = CARTESIAN_POINT ( 'NONE',  ( 0.4912014431318024732, -1.081758076222086862, 0.5909367962944523933 ) ) ;
#25210 = CARTESIAN_POINT ( 'NONE',  ( -0.1142670043590670731, -0.4723146173917492918, 0.1178658435937000315 ) ) ;
#25211 = CARTESIAN_POINT ( 'NONE',  ( 0.2831656786010217641, -1.548301601687314788, -0.3099957012843251869 ) ) ;
#25212 = CARTESIAN_POINT ( 'NONE',  ( 0.5805227504890819734, -1.495156126203962987, 0.5657488023295393909 ) ) ;
#25213 = CARTESIAN_POINT ( 'NONE',  ( -0.05543910610524985239, 0.2873579635174380864, -0.3608851239303206282 ) ) ;
#25214 = CARTESIAN_POINT ( 'NONE',  ( -0.1999999999999997891, 0.5182417262804734914, 0.3749999999999999445 ) ) ;
#25215 = CARTESIAN_POINT ( 'NONE',  ( -0.3000000000000000999, -2.761122741982423801, -0.2878817176880067996 ) ) ;
#25216 = AXIS2_PLACEMENT_3D ( 'NONE', #24197, #20703, #26680 ) ;
#25217 = DIRECTION ( 'NONE',  ( -0.3515883117872521946, 3.118021572908016454E-16, 0.9361547195921140485 ) ) ;
#25218 = ADVANCED_FACE ( 'NONE', ( #27232 ), #40354, .F. ) ;
#25219 = EDGE_CURVE ( 'NONE', #22886, #10025, #2721, .T. ) ;
#25220 = CARTESIAN_POINT ( 'NONE',  ( 0.4378619693737221819, -1.010538247186560268, 0.8194577876302902020 ) ) ;
#25221 = VECTOR ( 'NONE', #23229, 39.37007874015748854 ) ;
#25222 = AXIS2_PLACEMENT_3D ( 'NONE', #35557, #37848, #464 ) ;
#25223 = CARTESIAN_POINT ( 'NONE',  ( -0.04087116408467122985, 0.2940498268759185185, 0.3688792544161150211 ) ) ;
#25224 = CARTESIAN_POINT ( 'NONE',  ( 0.01419313219423278850, -1.039704043814793755, 0.5807212468082825207 ) ) ;
#25225 = EDGE_CURVE ( 'NONE', #34108, #37380, #790, .T. ) ;
#25226 = CARTESIAN_POINT ( 'NONE',  ( 0.6448693075501473748, -1.567563692131277220, -0.4251249543968058653 ) ) ;
#25227 = CARTESIAN_POINT ( 'NONE',  ( 0.3993946999846398893, -2.070215760155117213, -0.4742227968861380538 ) ) ;
#25228 = CARTESIAN_POINT ( 'NONE',  ( 0.05999999999999990757, -0.3829990175980249600, -0.3390339253215535198 ) ) ;
#25229 = EDGE_CURVE ( 'NONE', #11216, #20247, #10582, .T. ) ;
#25230 = CARTESIAN_POINT ( 'NONE',  ( 0.2676415634711663549, -1.674658064059759033, 0.5739467722781522729 ) ) ;
#25231 = AXIS2_PLACEMENT_3D ( 'NONE', #27325, #20942, #30393 ) ;
#25232 = DIRECTION ( 'NONE',  ( 1.000000000000000000, 1.446659165673942287E-15, -8.266623803851098360E-16 ) ) ;
#25233 = CIRCLE ( 'NONE', #14750, 0.1600000000000000588 ) ;
#25234 = ORIENTED_EDGE ( 'NONE', *, *, #18289, .T. ) ;
#25235 = DIRECTION ( 'NONE',  ( 1.000000000000000000, -1.799754070459521415E-12, 1.860523581402820487E-12 ) ) ;
#25236 = CARTESIAN_POINT ( 'NONE',  ( 0.5010411840214703538, -1.300757910890522062, 0.7890095542399213624 ) ) ;
#25237 = FACE_OUTER_BOUND ( 'NONE', #13806, .T. ) ;
#25238 = DIRECTION ( 'NONE',  ( 0.4999551463232373427, -0.8660512985181134660, 0.000000000000000000 ) ) ;
#25239 = CARTESIAN_POINT ( 'NONE',  ( 0.3398313727135623963, -1.151616092976642136, 0.5895549894284093373 ) ) ;
#25240 = ORIENTED_EDGE ( 'NONE', *, *, #37185, .F. ) ;
#25241 = CARTESIAN_POINT ( 'NONE',  ( 0.3639089045978470272, -1.623236563750744876, -0.6630443531552572267 ) ) ;
#25242 = ADVANCED_FACE ( 'NONE', ( #15493 ), #1058, .T. ) ;
#25243 = CARTESIAN_POINT ( 'NONE',  ( -0.3000000000000000999, -2.154189217240303655, -0.3012881438978375903 ) ) ;
#25244 = CARTESIAN_POINT ( 'NONE',  ( 0.1859093133543100740, -0.7573093211699954974, 0.1754562816741712661 ) ) ;
#25245 = APPROVAL ( #18963, 'UNSPECIFIED' ) ;
#25246 = CARTESIAN_POINT ( 'NONE',  ( 0.02242828275838930699, 0.3548975010106716343, -0.3695194593235469060 ) ) ;
#25247 = AXIS2_PLACEMENT_3D ( 'NONE', #29740, #32814, #20908 ) ;
#25248 = CARTESIAN_POINT ( 'NONE',  ( 0.4340226251431142934, -1.195050833747549834, 0.7346307913083539587 ) ) ;
#25250 = ORIENTED_EDGE ( 'NONE', *, *, #39388, .F. ) ;
#25249 = DIRECTION ( 'NONE',  ( 7.771561172376107616E-16, -7.170354002788761615E-17, 1.000000000000000000 ) ) ;
#25251 = CARTESIAN_POINT ( 'NONE',  ( 0.1920143701880955289, -0.8743002769911518701, 0.2704752137325454608 ) ) ;
#25252 = VERTEX_POINT ( 'NONE', #6412 ) ;
#25253 = COORDINATED_UNIVERSAL_TIME_OFFSET ( 0, 0, .AHEAD. ) ;
#25254 = DIRECTION ( 'NONE',  ( 0.000000000000000000, 0.000000000000000000, -1.000000000000000000 ) ) ;
#25255 = VERTEX_POINT ( 'NONE', #31512 ) ;
#25256 = CIRCLE ( 'NONE', #7493, 0.2200000000000001121 ) ;
#25257 = VECTOR ( 'NONE', #7917, 39.37007874015748854 ) ;
#25258 = CARTESIAN_POINT ( 'NONE',  ( 0.05827439840305041058, -0.6775244079679950682, 0.4991996434535173055 ) ) ;
#25260 = CARTESIAN_POINT ( 'NONE',  ( 0.1132202721956721558, -0.6714642036273535952, -0.09530415291956083335 ) ) ;
#25259 = CARTESIAN_POINT ( 'NONE',  ( 0.08569141848276186357, -0.7951378289679750244, 0.08553711018156767709 ) ) ;
#25261 = CARTESIAN_POINT ( 'NONE',  ( 0.3439881215215967458, -1.640653147150704871, -0.3778432901105419073 ) ) ;
#25262 =( GEOMETRIC_REPRESENTATION_CONTEXT ( 3 ) GLOBAL_UNCERTAINTY_ASSIGNED_CONTEXT ( ( #35074 ) ) GLOBAL_UNIT_ASSIGNED_CONTEXT ( ( #39522, #33359, #14633 ) ) REPRESENTATION_CONTEXT ( 'NONE', 'WORKASPACE' ) );
#25263 = ORIENTED_EDGE ( 'NONE', *, *, #16957, .T. ) ;
#25264 = ORIENTED_EDGE ( 'NONE', *, *, #14263, .F. ) ;
#25265 = VERTEX_POINT ( 'NONE', #24947 ) ;
#25266 = CARTESIAN_POINT ( 'NONE',  ( 0.4152142928025790991, -1.128277177651309193, 0.5697251069065648599 ) ) ;
#25267 = CARTESIAN_POINT ( 'NONE',  ( 0.1176201142355292467, -0.5735051211531788651, 0.2538439209176449607 ) ) ;
#25268 = ORIENTED_EDGE ( 'NONE', *, *, #3396, .F. ) ;
#25269 = AXIS2_PLACEMENT_3D ( 'NONE', #33492, #20974, #32888 ) ;
#25270 = CARTESIAN_POINT ( 'NONE',  ( 0.1874127487346899379, -0.6926261066621903772, 0.03768796299198888533 ) ) ;
#25271 = CARTESIAN_POINT ( 'NONE',  ( 0.1094055670226265625, -1.326767981663566243, -0.3565224830446982462 ) ) ;
#25272 = CARTESIAN_POINT ( 'NONE',  ( 0.1499999999999990508, -0.4770632572900511681, -0.2530032579707427454 ) ) ;
#25273 = CIRCLE ( 'NONE', #19276, 0.1999999999999994837 ) ;
#25274 = CARTESIAN_POINT ( 'NONE',  ( 0.4334739817046469601, -1.659740982267900566, -0.5155029497116575543 ) ) ;
#25275 = CARTESIAN_POINT ( 'NONE',  ( 0.07779920321647403048, -1.322114474344633583, 0.5682417262808776570 ) ) ;
#25276 = CARTESIAN_POINT ( 'NONE',  ( 0.5949938736933503280, -1.485520306704343207, -0.4218885508374648485 ) ) ;
#25277 = CARTESIAN_POINT ( 'NONE',  ( 0.08693421129271258763, -0.7278123032406825788, 0.02060656405704834257 ) ) ;
#25278 = CARTESIAN_POINT ( 'NONE',  ( -0.04828289906928839859, 0.05688126243839979057, 0.1249999999999993894 ) ) ;
#25279 = EDGE_CURVE ( 'NONE', #27922, #10402, #9512, .T. ) ;
#25280 = FACE_OUTER_BOUND ( 'NONE', #13453, .T. ) ;
#25281 = CARTESIAN_POINT ( 'NONE',  ( 0.05083665881509029372, 0.3162195626322004127, -0.3525671453250072140 ) ) ;
#25282 = CARTESIAN_POINT ( 'NONE',  ( 0.1630182088513137673, -1.785047172228910517, -0.6488655176575248706 ) ) ;
#25283 = CARTESIAN_POINT ( 'NONE',  ( -0.02000000000000000042, -2.196538720661423749, -0.6552417777791260667 ) ) ;
#25284 = CALENDAR_DATE ( 2026, 13, 10 ) ;
#25285 = AXIS2_PLACEMENT_3D ( 'NONE', #14833, #24716, #2074 ) ;
#25286 = EDGE_CURVE ( 'NONE', #14004, #18990, #23090, .T. ) ;
#25287 = EDGE_CURVE ( 'NONE', #33332, #33486, #22756, .T. ) ;
#25288 = CARTESIAN_POINT ( 'NONE',  ( 0.4862843069642890925, -1.079060212656593798, 0.6007065101366493298 ) ) ;
#25289 = AXIS2_PLACEMENT_3D ( 'NONE', #31195, #20928, #33449 ) ;
#25290 = CARTESIAN_POINT ( 'NONE',  ( 0.2086414000262838409, -1.361922069228335364, 0.4817113886979867421 ) ) ;
#25291 = ADVANCED_FACE ( 'NONE', ( #26521 ), #26734, .F. ) ;
#25292 = CARTESIAN_POINT ( 'NONE',  ( 0.4474210138429077221, -1.247506387532115735, 0.6057417262809816627 ) ) ;
#25293 = CARTESIAN_POINT ( 'NONE',  ( -0.2746410161513779258, -3.527715956914472706, -0.3920205355121876289 ) ) ;
#25294 = VECTOR ( 'NONE', #34322, 39.37007874015748143 ) ;
#25295 = AXIS2_PLACEMENT_3D ( 'NONE', #28146, #12311, #18070 ) ;
#25296 = SECURITY_CLASSIFICATION ( '', '', #27370 ) ;
#25297 = CARTESIAN_POINT ( 'NONE',  ( -0.003075981321608621880, -0.8070878537792822716, 0.1960017582677906212 ) ) ;
#25298 = CARTESIAN_POINT ( 'NONE',  ( 8.402003333010158955E-05, -0.6075279228541787813, -0.09071442693374498489 ) ) ;
#25299 = CARTESIAN_POINT ( 'NONE',  ( 0.1937395639937359026, -1.657857108843001193, -0.6872458559241637621 ) ) ;
#25300 = DIRECTION ( 'NONE',  ( -1.000000000000000000, -2.276539994720197063E-15, 0.000000000000000000 ) ) ;
#25301 = TOROIDAL_SURFACE ( 'NONE', #29906, 0.04749999999977554815, 0.01000000000000000021 ) ;
#25302 = ORIENTED_EDGE ( 'NONE', *, *, #7131, .F. ) ;
#25303 = ORIENTED_EDGE ( 'NONE', *, *, #34382, .F. ) ;
#25304 = ADVANCED_FACE ( 'NONE', ( #11085 ), #11496, .T. ) ;
#25305 = CARTESIAN_POINT ( 'NONE',  ( 0.3704391661570882177, -1.756796239285488337, 0.5182417262812423209 ) ) ;
#25306 = ORIENTED_EDGE ( 'NONE', *, *, #1735, .F. ) ;
#25307 = CARTESIAN_POINT ( 'NONE',  ( -0.2666757540196709186, 0.4921670437878968851, 0.3599999999999988765 ) ) ;
#25308 = CARTESIAN_POINT ( 'NONE',  ( 0.03662792686184443425, 0.3149733899719660002, 0.3635662525351497365 ) ) ;
#25309 = DIRECTION ( 'NONE',  ( -0.8660512985181135770, -0.4999551463232368431, 0.000000000000000000 ) ) ;
#25311 = ORIENTED_EDGE ( 'NONE', *, *, #20784, .T. ) ;
#25310 = CARTESIAN_POINT ( 'NONE',  ( -1.019575837292305831, -0.04310840302198155199, 0.3750000000000002220 ) ) ;
#25312 = ORIENTED_EDGE ( 'NONE', *, *, #9781, .F. ) ;
#25313 = DIRECTION ( 'NONE',  ( -1.387778780781449620E-15, 6.528313220153589231E-16, -1.000000000000000000 ) ) ;
#25314 = ORIENTED_EDGE ( 'NONE', *, *, #16965, .F. ) ;
#25315 = CARTESIAN_POINT ( 'NONE',  ( 0.1177973440672865080, -0.9935853818565597573, 0.8155281618166205782 ) ) ;
#25317 = CARTESIAN_POINT ( 'NONE',  ( 0.07780827639779400173, -1.322105357709411733, 0.5682417262808776570 ) ) ;
#25316 = CARTESIAN_POINT ( 'NONE',  ( 0.07530787293288457307, -0.8414947218206061397, 0.3166737376759417022 ) ) ;
#25318 = CARTESIAN_POINT ( 'NONE',  ( 0.3100229871264633674, -1.765619355789175948, 0.5593676469398386475 ) ) ;
#25319 = CARTESIAN_POINT ( 'NONE',  ( 0.1881312614525582350, -0.9196856789278203825, 0.05501147976861575639 ) ) ;
#25320 = VECTOR ( 'NONE', #27399, 39.37007874015748143 ) ;
#25321 = CARTESIAN_POINT ( 'NONE',  ( -2.112273405726188513E-14, -1.837418632672298768, -0.6339733133327630776 ) ) ;
#25323 = ORIENTED_EDGE ( 'NONE', *, *, #12309, .F. ) ;
#25322 = ORIENTED_EDGE ( 'NONE', *, *, #3045, .F. ) ;
#25324 = TOROIDAL_SURFACE ( 'NONE', #8207, 0.1333070866141734256, 0.02999999999999999889 ) ;
#25325 = CARTESIAN_POINT ( 'NONE',  ( 0.1960722456818423942, -1.288731303253011218, -0.2917126172454974631 ) ) ;
#25326 = CARTESIAN_POINT ( 'NONE',  ( 0.1862143093560568174, -0.9153542374865832887, 0.1410250186500938141 ) ) ;
#25327 = CARTESIAN_POINT ( 'NONE',  ( -0.02872242845530427816, -0.4768947642620218197, 0.2371557650701859032 ) ) ;
#25328 = CIRCLE ( 'NONE', #6612, 0.01500000000000000118 ) ;
#25329 = CARTESIAN_POINT ( 'NONE',  ( 0.5480184601717554838, -1.413123777809382364, 0.7684874893864968026 ) ) ;
#25330 = CARTESIAN_POINT ( 'NONE',  ( 0.3071154694917676009, -1.047539419770983304, 0.7367026581941298335 ) ) ;
#25331 = APPROVAL_PERSON_ORGANIZATION ( #2970, #14697, #40400 ) ;
#25332 = CARTESIAN_POINT ( 'NONE',  ( 0.2130547489620155110, -1.418506719972717489, 0.9320990850557395735 ) ) ;
#25333 = CARTESIAN_POINT ( 'NONE',  ( 0.1596578019756997591, -1.106139421783004062, 0.9882459099239285782 ) ) ;
#25334 = VECTOR ( 'NONE', #4916, 39.37007874015748143 ) ;
#25335 = CARTESIAN_POINT ( 'NONE',  ( 0.01548846960703768524, 0.09061086148575155097, -0.5171215251571049665 ) ) ;
#25336 = EDGE_CURVE ( 'NONE', #40606, #23678, #13226, .T. ) ;
#25337 = CARTESIAN_POINT ( 'NONE',  ( 0.1566196390284286255, -1.366403859981695224, 0.5182417262812423209 ) ) ;
#25338 = DIRECTION ( 'NONE',  ( 0.000000000000000000, 0.000000000000000000, -1.000000000000000000 ) ) ;
#25339 = DIRECTION ( 'NONE',  ( -1.000000000000000000, -0.000000000000000000, -0.000000000000000000 ) ) ;
#25340 =( LENGTH_UNIT ( ) NAMED_UNIT ( * ) SI_UNIT ( $, .METRE. ) );
#25341 = EDGE_CURVE ( 'NONE', #16916, #11170, #20780, .T. ) ;
#25342 = B_SPLINE_CURVE_WITH_KNOTS ( 'NONE', 3,
 ( #11472, #8370, #29780, #2420 ),
 .UNSPECIFIED., .F., .F.,
 ( 4, 4 ),
 ( 3.469446951953613804E-18, 0.0002990235347002869089 ),
 .UNSPECIFIED. ) ;
#25343 = CARTESIAN_POINT ( 'NONE',  ( 0.03170953572519073088, -0.3312786565686222096, 0.3635309226454363496 ) ) ;
#25344 = ADVANCED_FACE ( 'NONE', ( #38841 ), #1645, .T. ) ;
#25345 = FACE_OUTER_BOUND ( 'NONE', #35120, .T. ) ;
#25346 = CARTESIAN_POINT ( 'NONE',  ( 0.1040330991377019648, -1.397689221518311653, 0.6251921974533098947 ) ) ;
#25347 = APPROVAL_STATUS ( 'not_yet_approved' ) ;
#25348 = CARTESIAN_POINT ( 'NONE',  ( -0.03672447062657657052, 0.4430265621404759213, 0.1868507191434773673 ) ) ;
#25349 = AXIS2_PLACEMENT_3D ( 'NONE', #1981, #4438, #14110 ) ;
#25350 = AXIS2_PLACEMENT_3D ( 'NONE', #5575, #11955, #9828 ) ;
#25351 = CARTESIAN_POINT ( 'NONE',  ( 0.7071741867143577220, -1.496830158817513023, 0.5329102775952888615 ) ) ;
#25352 = EDGE_CURVE ( 'NONE', #30159, #20340, #30283, .T. ) ;
#25353 = ORIENTED_EDGE ( 'NONE', *, *, #15426, .T. ) ;
#25354 = CYLINDRICAL_SURFACE ( 'NONE', #40186, 0.08139150547213672149 ) ;
#25355 = ORIENTED_EDGE ( 'NONE', *, *, #4505, .F. ) ;
#25356 = DIRECTION ( 'NONE',  ( 0.4999999999999982792, 0.8489817559768471078, 0.1709677689462869299 ) ) ;
#25357 = SECURITY_CLASSIFICATION ( '', '', #34779 ) ;
#25358 = CARTESIAN_POINT ( 'NONE',  ( 0.2162209611966269818, -1.457820977148307051, 0.9280216023009758564 ) ) ;
#25359 = EDGE_CURVE ( 'NONE', #13009, #21906, #16495, .T. ) ;
#25360 = CARTESIAN_POINT ( 'NONE',  ( 0.1322362858526628659, -0.5735584538993211412, 0.2455366585897305887 ) ) ;
#25362 = VERTEX_POINT ( 'NONE', #33286 ) ;
#25361 = CARTESIAN_POINT ( 'NONE',  ( 0.3817257825202987065, -1.726009493650376259, 0.4251351636136782575 ) ) ;
#25363 = ADVANCED_FACE ( 'NONE', ( #20155 ), #36218, .T. ) ;
#25364 = CIRCLE ( 'NONE', #33902, 0.5515209409081858194 ) ;
#25366 = ORIENTED_EDGE ( 'NONE', *, *, #32928, .T. ) ;
#25365 = ORIENTED_EDGE ( 'NONE', *, *, #16448, .T. ) ;
#25367 = CARTESIAN_POINT ( 'NONE',  ( 0.4093192649698303431, -1.477391824278450061, -0.4706793243405929528 ) ) ;
#25368 =( BOUNDED_SURFACE ( )  B_SPLINE_SURFACE ( 3, 2, ( 
 ( #36652, #5162, #1719 ),
 ( #17715, #14236, #2310 ),
 ( #14629, #4965, #33544 ),
 ( #27200, #2092, #2511 ) ),
 .UNSPECIFIED., .F., .F., .T. ) 
 B_SPLINE_SURFACE_WITH_KNOTS ( ( 4, 4 ),
 ( 3, 3 ),
 ( -2.862293735361731706E-17, 0.001825051142017923740 ),
 ( 0.000000000000000000, 1.000000000000000000 ),
 .UNSPECIFIED. ) 
 GEOMETRIC_REPRESENTATION_ITEM ( )  RATIONAL_B_SPLINE_SURFACE ( (
 ( 1.000000000000000000, 0.7061763356917307721, 1.000000000000000000),
 ( 1.000000000000000000, 0.7067362331337545545, 1.000000000000000000),
 ( 1.000000000000000000, 0.7071034392571972083, 1.000000000000000000),
 ( 1.000000000000000000, 0.7071067811865461294, 1.000000000000000000) ) ) 
 REPRESENTATION_ITEM ( '' )  SURFACE ( )  );
#25369 = ORIENTED_EDGE ( 'NONE', *, *, #29125, .F. ) ;
#25370 = EDGE_CURVE ( 'NONE', #9409, #18158, #23723, .T. ) ;
#25371 = CARTESIAN_POINT ( 'NONE',  ( 0.6277577389591226797, -1.601617165483917971, -0.5786592524461142695 ) ) ;
#25372 = DATE_AND_TIME ( #18786, #13543 ) ;
#25373 = CARTESIAN_POINT ( 'NONE',  ( -0.05464101615137787610, -2.183180860297908144, -0.4937760292030871079 ) ) ;
#25374 = EDGE_LOOP ( 'NONE', ( #734, #33075 ) ) ;
#25375 = CARTESIAN_POINT ( 'NONE',  ( 0.08538299691383864631, -0.7671892257780278390, 0.1457185332388683252 ) ) ;
#25376 = CARTESIAN_POINT ( 'NONE',  ( 0.4358024118727818474, -1.610872297623142879, -0.3687891571712654804 ) ) ;
#25377 = CARTESIAN_POINT ( 'NONE',  ( 0.5265351747158187878, -1.525993753803500663, 0.6091402573601836234 ) ) ;
#25378 = DIRECTION ( 'NONE',  ( 1.000000000000000000, 0.000000000000000000, 0.000000000000000000 ) ) ;
#25379 = DIRECTION ( 'NONE',  ( 1.000000000000000000, 2.280301054154495132E-31, -1.664003471950577689E-31 ) ) ;
#25380 = VERTEX_POINT ( 'NONE', #8189 ) ;
#25381 = CARTESIAN_POINT ( 'NONE',  ( 0.4419048264408250715, -1.686280600454902245, 0.4284299735159858291 ) ) ;
#25382 = CLOSED_SHELL ( 'NONE', ( #14807, #18979, #14434, #30851, #35535, #34089, #9434, #38811, #37285, #23077, #37309, #9124, #39215, #37618, #26775, #4476 ) ) ;
#25383 = CARTESIAN_POINT ( 'NONE',  ( 0.6879396389015977054, -1.414347470100213666, 0.6986533948158418772 ) ) ;
#25384 = AXIS2_PLACEMENT_3D ( 'NONE', #12013, #2751, #5627 ) ;
#25385 = ORIENTED_EDGE ( 'NONE', *, *, #31048, .F. ) ;
#25386 = DIRECTION ( 'NONE',  ( 0.000000000000000000, -0.8834504764629538265, -0.4685245517978538499 ) ) ;
#25387 = CARTESIAN_POINT ( 'NONE',  ( 0.1348063704134844498, -0.5683947605430353933, 0.2284001142341055557 ) ) ;
#25388 = CARTESIAN_POINT ( 'NONE',  ( 0.05999999999999990757, -0.01787811284557883421, -0.1489307660662511357 ) ) ;
#25389 = SECURITY_CLASSIFICATION ( '', '', #5194 ) ;
#25390 = EDGE_CURVE ( 'NONE', #19429, #21211, #1438, .T. ) ;
#25391 = CARTESIAN_POINT ( 'NONE',  ( 0.1435064959217801916, -1.283467536720964697, 0.5197417262808780025 ) ) ;
#25392 = CARTESIAN_POINT ( 'NONE',  ( 0.04154009738085429754, -0.4523583096281913463, -0.1287716261385816463 ) ) ;
#25393 = EDGE_CURVE ( 'NONE', #8912, #5500, #2104, .T. ) ;
#25394 = AXIS2_PLACEMENT_3D ( 'NONE', #7893, #40401, #14903 ) ;
#25395 = CARTESIAN_POINT ( 'NONE',  ( 0.008926059106093127415, -1.005466151381485762, 0.5191422350400326513 ) ) ;
#25396 = CARTESIAN_POINT ( 'NONE',  ( 0.5135568109339374576, -1.117989077717415292, 0.5796127612779116145 ) ) ;
#25397 = PERSON_AND_ORGANIZATION ( #28500, #32463 ) ;
#25398 = FACE_OUTER_BOUND ( 'NONE', #40561, .T. ) ;
#25399 = CARTESIAN_POINT ( 'NONE',  ( 0.5138082349489954126, -1.531582140144923443, 0.5361777791604406262 ) ) ;
#25400 = CARTESIAN_POINT ( 'NONE',  ( -0.03478556507500938505, 0.07228131100493534467, 0.5113607228826224649 ) ) ;
#25401 = ORIENTED_EDGE ( 'NONE', *, *, #34575, .T. ) ;
#25402 = CARTESIAN_POINT ( 'NONE',  ( -0.08000000000000000167, -1.699711333021935777, -0.9366211149475224262 ) ) ;
#25403 = FACE_BOUND ( 'NONE', #19559, .T. ) ;
#25404 = CARTESIAN_POINT ( 'NONE',  ( 0.1893571754530913309, -0.8322940459586247730, 0.2468763379997500618 ) ) ;
#25405 = ORIENTED_EDGE ( 'NONE', *, *, #35525, .T. ) ;
#25406 = CIRCLE ( 'NONE', #493, 0.01500000000000005496 ) ;
#25407 = CARTESIAN_POINT ( 'NONE',  ( 0.4971920908461615607, -1.080069027881642052, 0.4687417262808780127 ) ) ;
#25408 = CARTESIAN_POINT ( 'NONE',  ( -0.002729411228280882208, -0.9128323640382212112, 0.5539659124371107968 ) ) ;
#25410 = ORIENTED_EDGE ( 'NONE', *, *, #18481, .T. ) ;
#25409 = ORIENTED_EDGE ( 'NONE', *, *, #13943, .F. ) ;
#25411 = DIRECTION ( 'NONE',  ( 0.000000000000000000, -0.9901182710308679136, 0.1402348365094949756 ) ) ;
#25412 = DIRECTION ( 'NONE',  ( -0.8660512985181135770, -0.4999551463232370097, 0.000000000000000000 ) ) ;
#25413 = APPLIED_APPROVAL_ASSIGNMENT ( #36670, ( #18145 ) ) ;
#25414 = CARTESIAN_POINT ( 'NONE',  ( 0.2988334432509203720, -1.539938620923237300, -0.3360421071361874845 ) ) ;
#25416 = CARTESIAN_POINT ( 'NONE',  ( 0.6413879784614744395, -1.405912376546664122, -0.6250000000000000000 ) ) ;
#25415 = CARTESIAN_POINT ( 'NONE',  ( 0.03877220711929791480, 0.4416859332762684276, 0.1784371778270431863 ) ) ;
#25417 = CARTESIAN_POINT ( 'NONE',  ( 0.04157078424165335656, -0.2624491172974833808, -0.3902147976630872539 ) ) ;
#25418 = ORIENTED_EDGE ( 'NONE', *, *, #40125, .T. ) ;
#25419 = CARTESIAN_POINT ( 'NONE',  ( -0.03664605387828200056, 0.2484618661253114036, -0.4118464167359224271 ) ) ;
#25420 = ORIENTED_EDGE ( 'NONE', *, *, #38315, .T. ) ;
#25421 = ORIENTED_EDGE ( 'NONE', *, *, #21749, .T. ) ;
#25422 = AXIS2_PLACEMENT_3D ( 'NONE', #14325, #36124, #7932 ) ;
#25423 = CARTESIAN_POINT ( 'NONE',  ( 0.09255270613366611832, -0.5765971826892936081, 0.2511563476660008676 ) ) ;
#25424 = ORIENTED_EDGE ( 'NONE', *, *, #4146, .T. ) ;
#25425 = ORIENTED_EDGE ( 'NONE', *, *, #31326, .T. ) ;
#25426 = CARTESIAN_POINT ( 'NONE',  ( 2.155092840285021536E-05, -0.4374981960197986131, 0.2330919378759825356 ) ) ;
#25427 = CARTESIAN_POINT ( 'NONE',  ( 0.3368577323154672287, -1.280641800761222360, 0.8706439758358487380 ) ) ;
#25429 = CARTESIAN_POINT ( 'NONE',  ( -0.1743922129835733803, -0.5166151207188712791, 0.3749999999999999445 ) ) ;
#25428 = CARTESIAN_POINT ( 'NONE',  ( 0.4625514705274676452, -1.592010743194695932, -0.4306025673467906434 ) ) ;
#25430 = CARTESIAN_POINT ( 'NONE',  ( 0.005980720888701209978, -0.8455916207747946611, 0.1457185332388707122 ) ) ;
#25431 = CARTESIAN_POINT ( 'NONE',  ( 0.4929465528686921560, -1.082715557938388029, 0.5682417262808779901 ) ) ;
#25432 = CARTESIAN_POINT ( 'NONE',  ( 0.3999999999999785949, -2.097675824466503247, -0.7286991843995642704 ) ) ;
#25433 = CARTESIAN_POINT ( 'NONE',  ( 0.1897112079047662825, -0.5340520988485676357, 0.1406012133455345203 ) ) ;
#25434 = CARTESIAN_POINT ( 'NONE',  ( 0.5814726822843937493, -1.495195014991375304, 0.5853331262226206810 ) ) ;
#25435 = CARTESIAN_POINT ( 'NONE',  ( -0.05252359774140038379, 0.2683439431814198528, -0.3847367734645201209 ) ) ;
#25436 = CARTESIAN_POINT ( 'NONE',  ( -0.02000000000000000042, -2.092549851682985018, -0.5406114768595331466 ) ) ;
#25437 = CARTESIAN_POINT ( 'NONE',  ( -0.01899468245561210245, -0.4667220838189795051, -0.2292241428221102884 ) ) ;
#25438 = CARTESIAN_POINT ( 'NONE',  ( 0.07161007277227926515, -0.5641287990778131034, 0.2518656736807903807 ) ) ;
#25439 = LINE ( 'NONE', #28718, #9565 ) ;
#25440 = CIRCLE ( 'NONE', #39869, 0.1000000000000000194 ) ;
#25441 = CARTESIAN_POINT ( 'NONE',  ( 0.2097017171917790468, -0.6397877375661684685, 0.3875311123790295409 ) ) ;
#25442 = FACE_OUTER_BOUND ( 'NONE', #20723, .T. ) ;
#25443 = CARTESIAN_POINT ( 'NONE',  ( 0.06380316775577042632, -1.284647545824749049, 0.6326371944557522831 ) ) ;
#25444 = CARTESIAN_POINT ( 'NONE',  ( 0.03174060074382212965, 0.4701996045334482233, -0.2325360656123031111 ) ) ;
#25445 = CARTESIAN_POINT ( 'NONE',  ( 0.4780249079440049287, -1.118244978643492260, -0.3962549247049245715 ) ) ;
#25446 = CARTESIAN_POINT ( 'NONE',  ( 0.1950551304375616468, -0.8882144403296816648, 0.6132150535162333993 ) ) ;
#25447 = CARTESIAN_POINT ( 'NONE',  ( 0.3663975874019590462, -1.157438136726378408, 0.4269148889825721827 ) ) ;
#25448 = CARTESIAN_POINT ( 'NONE',  ( -0.02000000000000000042, -2.070343076906777213, -0.2454056712452573896 ) ) ;
#25449 = VERTEX_POINT ( 'NONE', #14780 ) ;
#25450 = CYLINDRICAL_SURFACE ( 'NONE', #25979, 0.08749999999977552123 ) ;
#25451 = CARTESIAN_POINT ( 'NONE',  ( 0.2382400519805366879, -0.9170320373645088896, 0.6858731337248115123 ) ) ;
#25452 = DIRECTION ( 'NONE',  ( -1.000000000000000000, 0.000000000000000000, -7.847494366974319310E-16 ) ) ;
#25453 = DIRECTION ( 'NONE',  ( 0.000000000000000000, 0.000000000000000000, 1.000000000000000000 ) ) ;
#25454 = FACE_OUTER_BOUND ( 'NONE', #4286, .T. ) ;
#25455 = VERTEX_POINT ( 'NONE', #9402 ) ;
#25456 = CARTESIAN_POINT ( 'NONE',  ( 0.5350387257620740078, -1.658384496898128724, -0.5719998859210704278 ) ) ;
#25457 = CARTESIAN_POINT ( 'NONE',  ( 0.2955290772965331048, -1.312059711113043869, 0.4171601467298353683 ) ) ;
#25458 = DIRECTION ( 'NONE',  ( 0.000000000000000000, 0.8834504764630464191, -0.4685245517976792673 ) ) ;
#25459 = CARTESIAN_POINT ( 'NONE',  ( 0.1443375672974070711, 0.07999999999999969635, 0.000000000000000000 ) ) ;
#25460 = CARTESIAN_POINT ( 'NONE',  ( 0.4990439851886846467, -1.290753470885830367, 0.6181967010847094768 ) ) ;
#25462 = CARTESIAN_POINT ( 'NONE',  ( 0.3206961510659663839, -1.761846847463105714, 0.5004172992779960527 ) ) ;
#25461 = CARTESIAN_POINT ( 'NONE',  ( 0.06980746140711582837, 5.828670879282072084E-17, 0.1749999999999999889 ) ) ;
#25463 = CARTESIAN_POINT ( 'NONE',  ( 0.4903202831852248589, -1.081274614053407523, 0.5895842322316532380 ) ) ;
#25464 = VERTEX_POINT ( 'NONE', #21157 ) ;
#25465 = DATE_AND_TIME ( #20659, #18806 ) ;
#25466 = DIRECTION ( 'NONE',  ( -0.4999551463231795001, 0.8660512985181467727, -4.414622697374767230E-14 ) ) ;
#25467 = ORIENTED_EDGE ( 'NONE', *, *, #26110, .T. ) ;
#25468 = CARTESIAN_POINT ( 'NONE',  ( 0.1074504339463943636, -0.8508434056105943499, 0.7040215940812857287 ) ) ;
#25470 = DIRECTION ( 'NONE',  ( 0.4999551463232377313, -0.8660512985181132439, -0.000000000000000000 ) ) ;
#25469 = CARTESIAN_POINT ( 'NONE',  ( 0.08520265857480655014, -0.8310134553494858967, 0.1293978458592746628 ) ) ;
#25471 = CARTESIAN_POINT ( 'NONE',  ( 0.3425551896464547053, -1.643320776792971616, -0.3792307086401233152 ) ) ;
#25472 = ORIENTED_EDGE ( 'NONE', *, *, #9934, .F. ) ;
#25473 = EDGE_LOOP ( 'NONE', ( #12706, #6378 ) ) ;
#25474 = DIRECTION ( 'NONE',  ( -0.5196387294542602620, 0.8543860900384334656, 0.000000000000000000 ) ) ;
#25475 = CARTESIAN_POINT ( 'NONE',  ( 0.1193658396322129084, -0.5857129773433993325, 0.2871785300524037909 ) ) ;
#25476 = ORIENTED_EDGE ( 'NONE', *, *, #32500, .T. ) ;
#25477 = CARTESIAN_POINT ( 'NONE',  ( 0.07082949537098930104, -1.327879666565185968, 0.4918166835856172536 ) ) ;
#25478 = CARTESIAN_POINT ( 'NONE',  ( 0.1619657438594586940, -1.395601528504655020, -0.3525121130699213623 ) ) ;
#25479 = DIRECTION ( 'NONE',  ( -0.4999999999999988898, -0.7377595849475285794, -0.4535535192433760576 ) ) ;
#25480 = CARTESIAN_POINT ( 'NONE',  ( 0.3513236816452379729, -1.665692895111267058, -0.7210133640968660051 ) ) ;
#25481 = DIRECTION ( 'NONE',  ( 0.4999551463232372317, -0.8660512985181134660, 0.000000000000000000 ) ) ;
#25482 = CARTESIAN_POINT ( 'NONE',  ( 0.02953079040095700838, 0.3810518745593862167, -0.3687679460475775106 ) ) ;
#25483 = CARTESIAN_POINT ( 'NONE',  ( 0.08509945581906654122, -0.7689446773063483009, 0.1451249978468672763 ) ) ;
#25484 = CARTESIAN_POINT ( 'NONE',  ( 0.6320591615222423965, -1.324690328322339239, 0.8595101463142521547 ) ) ;
#25485 = CARTESIAN_POINT ( 'NONE',  ( 0.1974703294706521284, -2.027200055516245047, -0.7082635437208197882 ) ) ;
#25486 = CARTESIAN_POINT ( 'NONE',  ( 0.08591898661219740663, -1.312985777298583567, 0.5876069855766993255 ) ) ;
#25487 = ADVANCED_FACE ( 'NONE', ( #8580 ), #24401, .F. ) ;
#25488 = DIRECTION ( 'NONE',  ( 1.000000000000000000, 1.517693329813464577E-15, -7.588466649067322887E-16 ) ) ;
#25489 = SPHERICAL_SURFACE ( 'NONE', #39567, 0.01499999999999999944 ) ;
#25490 = PERSON_AND_ORGANIZATION ( #28500, #32463 ) ;
#25491 = APPLIED_DATE_AND_TIME_ASSIGNMENT ( #27021, #2341, ( #31951 ) ) ;
#25492 = CARTESIAN_POINT ( 'NONE',  ( 0.3535325904207607950, -1.006223909752091972, 0.6094712593526115940 ) ) ;
#25493 = DIRECTION ( 'NONE',  ( -1.000000000000000000, 0.000000000000000000, 0.000000000000000000 ) ) ;
#25494 = CARTESIAN_POINT ( 'NONE',  ( 0.06486042810549992599, -1.341249661891149803, 0.5682417262808776570 ) ) ;
#25495 = CARTESIAN_POINT ( 'NONE',  ( 0.2626492960486415673, -1.683514498680941607, 0.5584510130552119422 ) ) ;
#25496 = CARTESIAN_POINT ( 'NONE',  ( -0.003124719664520056797, -0.8057675726412014683, 0.1627348865840318737 ) ) ;
#25497 = CARTESIAN_POINT ( 'NONE',  ( 0.0003398915440874476107, -0.4642088512194108563, 0.03525733416984885848 ) ) ;
#25498 = FACE_OUTER_BOUND ( 'NONE', #21868, .T. ) ;
#25499 = CARTESIAN_POINT ( 'NONE',  ( -0.1743922129835733803, -0.5166151207188712791, 0.3749999999999999445 ) ) ;
#25500 = AXIS2_PLACEMENT_3D ( 'NONE', #10236, #29361, #20109 ) ;
#25501 = ORIENTED_EDGE ( 'NONE', *, *, #11146, .T. ) ;
#25502 = ORIENTED_EDGE ( 'NONE', *, *, #36182, .F. ) ;
#25503 = DIRECTION ( 'NONE',  ( 1.000000000000000000, 0.000000000000000000, 0.000000000000000000 ) ) ;
#25504 = ORIENTED_EDGE ( 'NONE', *, *, #4202, .T. ) ;
#25505 = CARTESIAN_POINT ( 'NONE',  ( -0.03868649100028202781, 0.03360400204099593668, 0.4753701585314237255 ) ) ;
#25506 = CARTESIAN_POINT ( 'NONE',  ( 0.02869942827333547136, 0.3396431753871657078, 0.3648167270360635484 ) ) ;
#25507 = FACE_OUTER_BOUND ( 'NONE', #33127, .T. ) ;
#25509 = ORIENTED_EDGE ( 'NONE', *, *, #6197, .T. ) ;
#25508 = DIRECTION ( 'NONE',  ( -1.000000000000000000, -2.341930812374887555E-31, 1.664003471950578127E-31 ) ) ;
#25510 = ADVANCED_FACE ( 'NONE', ( #34298 ), #5499, .T. ) ;
#25511 = ORIENTED_EDGE ( 'NONE', *, *, #27649, .T. ) ;
#25512 = FACE_OUTER_BOUND ( 'NONE', #22802, .T. ) ;
#25513 = EDGE_CURVE ( 'NONE', #7962, #22322, #17849, .T. ) ;
#25514 = ORIENTED_EDGE ( 'NONE', *, *, #6126, .F. ) ;
#25515 = CARTESIAN_POINT ( 'NONE',  ( 0.2970205159420773455, -1.628083574653397481, 0.7594346419547136628 ) ) ;
#25517 = DIRECTION ( 'NONE',  ( 0.4999551463232372317, -0.8660512985181134660, 0.000000000000000000 ) ) ;
#25516 = DIRECTION ( 'NONE',  ( -1.355854680848614260E-31, 3.330669073875470114E-16, 1.000000000000000000 ) ) ;
#25518 = CYLINDRICAL_SURFACE ( 'NONE', #39805, 0.06000000000000045575 ) ;
#25519 = CARTESIAN_POINT ( 'NONE',  ( 0.05999999999999990757, 0.1428018198284763673, -0.1638325989215043410 ) ) ;
#25520 = CONTEXT_DEPENDENT_SHAPE_REPRESENTATION ( #14519, #1607 ) ;
#25521 = EDGE_CURVE ( 'NONE', #12802, #33134, #21379, .T. ) ;
#25522 = EDGE_CURVE ( 'NONE', #3740, #29449, #38825, .T. ) ;
#25523 = CARTESIAN_POINT ( 'NONE',  ( -0.1126900943355985951, -0.5191528601549348920, 0.3070571034469349869 ) ) ;
#25525 = ORIENTED_EDGE ( 'NONE', *, *, #274, .F. ) ;
#25524 = ORIENTED_EDGE ( 'NONE', *, *, #25793, .T. ) ;
#25526 = ADVANCED_FACE ( 'NONE', ( #30813, #24447, #2634 ), #37579, .T. ) ;
#25527 = DIRECTION ( 'NONE',  ( -1.028089648204243318E-15, 0.7692307692307690514, 0.6389710663783134681 ) ) ;
#25528 = CARTESIAN_POINT ( 'NONE',  ( 0.1109098225493666129, -0.9286357918493259866, 0.1499897478545695051 ) ) ;
#25529 = DIRECTION ( 'NONE',  ( 8.881784197001245421E-16, -2.361472542561082612E-16, 1.000000000000000000 ) ) ;
#25530 = CARTESIAN_POINT ( 'NONE',  ( 0.5676195825672284423, -1.407416061909668725, 0.7341546013530008130 ) ) ;
#25531 = CARTESIAN_POINT ( 'NONE',  ( 0.3607701097029427095, -1.124548115609032672, 0.7351652811684338262 ) ) ;
#25532 = CARTESIAN_POINT ( 'NONE',  ( 0.01251508115950892945, -0.5804186138772022829, 0.3264740463578477137 ) ) ;
#25533 = CARTESIAN_POINT ( 'NONE',  ( 0.4784772001453526657, -1.116132439391088749, 0.5343330151343557155 ) ) ;
#25534 = DIRECTION ( 'NONE',  ( -1.355854680848614260E-31, 3.330669073875470114E-16, 1.000000000000000000 ) ) ;
#25535 = DIRECTION ( 'NONE',  ( 0.4999551463232372317, -0.8660512985181135770, 0.000000000000000000 ) ) ;
#25536 = CARTESIAN_POINT ( 'NONE',  ( 0.4647870327407357394, -1.232526483438142861, 0.6307241740363012106 ) ) ;
#25537 = EDGE_CURVE ( 'NONE', #20247, #16911, #15170, .T. ) ;
#25538 = DIRECTION ( 'NONE',  ( -1.188678714063518227E-15, 1.000000000000000000, 3.263080277421930985E-16 ) ) ;
#25539 = CARTESIAN_POINT ( 'NONE',  ( 0.000000000000000000, 0.000000000000000000, 0.000000000000000000 ) ) ;
#25540 = CARTESIAN_POINT ( 'NONE',  ( 0.02881195911414956984, -0.3393447726770147943, 0.3647551865608084642 ) ) ;
#25541 = CARTESIAN_POINT ( 'NONE',  ( 0.02385183771220368218, -0.6100559285722760849, 0.5958381505304063408 ) ) ;
#25542 = CARTESIAN_POINT ( 'NONE',  ( 0.1036797529164252135, -1.395233841299822419, 0.6304550959310950553 ) ) ;
#25543 = DATE_TIME_ROLE ( 'creation_date' ) ;
#25544 = CARTESIAN_POINT ( 'NONE',  ( 0.1856681452801951515, -1.696504954290812606, -0.6536319978138861453 ) ) ;
#25545 = CARTESIAN_POINT ( 'NONE',  ( -0.04575185649131228993, 0.4792489163483339421, 0.08731931755212994639 ) ) ;
#25546 = CARTESIAN_POINT ( 'NONE',  ( -0.2399999999999999079, -2.183180860297908144, -0.4312760292030870524 ) ) ;
#25547 = EDGE_CURVE ( 'NONE', #17210, #14594, #15596, .T. ) ;
#25548 = ORIENTED_EDGE ( 'NONE', *, *, #39220, .F. ) ;
#25549 = CARTESIAN_POINT ( 'NONE',  ( 0.3777575235213288529, -1.142457055047713110, 0.4315219747622728863 ) ) ;
#25550 = VERTEX_POINT ( 'NONE', #21574 ) ;
#25551 = CYLINDRICAL_SURFACE ( 'NONE', #17815, 0.5399999999999999245 ) ;
#25552 = CARTESIAN_POINT ( 'NONE',  ( 0.000000000000000000, -0.3767386922704979990, -0.2665524483967541269 ) ) ;
#25553 = CARTESIAN_POINT ( 'NONE',  ( 0.5949237905379889391, -1.487194157178949094, 0.5729122955301783060 ) ) ;
#25555 = EDGE_LOOP ( 'NONE', ( #15628, #27715, #29305, #22997, #37591, #6753 ) ) ;
#25554 = DIRECTION ( 'NONE',  ( -8.881784197001246407E-16, 2.361472542561082612E-16, -1.000000000000000000 ) ) ;
#25557 = VERTEX_POINT ( 'NONE', #9013 ) ;
#25556 = ORIENTED_EDGE ( 'NONE', *, *, #9802, .T. ) ;
#25558 = CARTESIAN_POINT ( 'NONE',  ( 0.6233902549407862592, -1.444966001498531272, 0.8349750966499661642 ) ) ;
#25559 = EDGE_CURVE ( 'NONE', #15099, #29592, #37499, .T. ) ;
#25560 = VERTEX_POINT ( 'NONE', #18460 ) ;
#25561 = CARTESIAN_POINT ( 'NONE',  ( -0.1603938765018537715, 0.4636889572247753222, 0.1178658435936994903 ) ) ;
#25562 = CONTEXT_DEPENDENT_SHAPE_REPRESENTATION ( #34219, #5192 ) ;
#25563 = EDGE_CURVE ( 'NONE', #36473, #4497, #38885, .T. ) ;
#25564 = CARTESIAN_POINT ( 'NONE',  ( 0.3099339588126717171, -1.765677022123078421, 0.5623500827625801390 ) ) ;
#25565 = ORIENTED_EDGE ( 'NONE', *, *, #30846, .F. ) ;
#25566 = EDGE_CURVE ( 'NONE', #20672, #21212, #19779, .T. ) ;
#25567 = CARTESIAN_POINT ( 'NONE',  ( 0.09437040392396874033, -0.7574139486114807029, 0.2971058147919648507 ) ) ;
#25568 = CARTESIAN_POINT ( 'NONE',  ( 0.08990536851188153655, -0.5646295468556791208, 0.1460913089649357455 ) ) ;
#25569 = CARTESIAN_POINT ( 'NONE',  ( 0.4943412959198616452, -1.443455042774087760, 0.7864209901413284909 ) ) ;
#25570 = CARTESIAN_POINT ( 'NONE',  ( 0.000000000000000000, 0.2463462108298974940, -0.03520871226632921180 ) ) ;
#25571 = CARTESIAN_POINT ( 'NONE',  ( -0.1638606670177142899, 0.5090623078239778776, 0.1147396705136388417 ) ) ;
#25572 = CARTESIAN_POINT ( 'NONE',  ( 0.6806522551434478485, -1.498521771693993587, 0.4238695236950315026 ) ) ;
#25573 = ORIENTED_EDGE ( 'NONE', *, *, #3621, .T. ) ;
#25574 = FACE_OUTER_BOUND ( 'NONE', #13410, .T. ) ;
#25575 = CARTESIAN_POINT ( 'NONE',  ( 0.7432499820993477835, -1.511365401434814570, 0.6392776140757149284 ) ) ;
#25576 = ORIENTED_EDGE ( 'NONE', *, *, #24046, .F. ) ;
#25577 = DIRECTION ( 'NONE',  ( 0.4999551463232371762, -0.8660512985181134660, 0.000000000000000000 ) ) ;
#25578 = CARTESIAN_POINT ( 'NONE',  ( 0.6089010132592387325, -1.475778064326142003, 0.6288872192019396845 ) ) ;
#25579 = CARTESIAN_POINT ( 'NONE',  ( 0.05561176441985648394, -0.4316390549698289059, 0.1616802657107465069 ) ) ;
#25580 = EDGE_CURVE ( 'NONE', #19429, #34796, #17807, .T. ) ;
#25581 =( LENGTH_UNIT ( ) NAMED_UNIT ( * ) SI_UNIT ( $, .METRE. ) );
#25582 = EDGE_CURVE ( 'NONE', #10550, #8335, #37797, .T. ) ;
#25583 = DIRECTION ( 'NONE',  ( -0.000000000000000000, 0.9246857012436752177, -0.3807313408632030383 ) ) ;
#25584 = EDGE_CURVE ( 'NONE', #9058, #33739, #5306, .T. ) ;
#25585 = DIRECTION ( 'NONE',  ( -7.771561172376107616E-16, 7.170354002788761615E-17, -1.000000000000000000 ) ) ;
#25586 = CARTESIAN_POINT ( 'NONE',  ( 0.003677659035771949428, -0.9373694290314303901, 0.4460629830528545781 ) ) ;
#25587 = CARTESIAN_POINT ( 'NONE',  ( 0.3909368226714677319, -0.9916197579736178991, 0.6726537802841677793 ) ) ;
#25588 = APPROVAL_ROLE ( '' ) ;
#25589 = CARTESIAN_POINT ( 'NONE',  ( 0.1626176757286639796, -0.6782218769987641283, 0.05683303076865411224 ) ) ;
#25590 = CARTESIAN_POINT ( 'NONE',  ( -0.02235124290213108197, 0.4612278572487595873, -0.2234747101372520361 ) ) ;
#25591 = CARTESIAN_POINT ( 'NONE',  ( -0.04308745346420495698, 0.05688354191225430956, 0.4910214150057473081 ) ) ;
#25592 = B_SPLINE_CURVE_WITH_KNOTS ( 'NONE', 3,
 ( #11346, #14848, #11753, #40124, #17914, #23916 ),
 .UNSPECIFIED., .F., .F.,
 ( 4, 2, 4 ),
 ( 0.0001712049647610483895, 0.0007981265351246958793, 0.001425048105488343261 ),
 .UNSPECIFIED. ) ;
#25593 =( BOUNDED_SURFACE ( )  B_SPLINE_SURFACE ( 3, 2, ( 
 ( #4662, #7568, #37125 ),
 ( #33841, #26721, #39041 ),
 ( #13735, #40194, #20337 ),
 ( #33069, #10659, #26508 ),
 ( #29392, #11072, #39250 ),
 ( #19922, #17238, #4283 ),
 ( #26302, #23230, #38827 ),
 ( #18196, #1236, #23633 ),
 ( #36151, #16850, #7960 ),
 ( #4875, #20535, #2566 ),
 ( #35755, #7770, #20143 ),
 ( #29787, #17446, #29998 ),
 ( #39442, #32858, #15101 ),
 ( #32669, #23835, #17041 ),
 ( #1629, #1831, #4475 ),
 ( #29580, #14347, #11267 ),
 ( #36911, #1424, #8721 ),
 ( #13938, #21300, #5642 ),
 ( #30746, #35963, #10873 ),
 ( #23446, #27662, #12027 ),
 ( #15918, #31164, #6037 ),
 ( #15526, #31366, #18389 ) ),
 .UNSPECIFIED., .F., .F., .F. ) 
 B_SPLINE_SURFACE_WITH_KNOTS ( ( 4, 2, 2, 2, 2, 2, 2, 2, 2, 2, 4 ),
 ( 3, 3 ),
 ( 0.002013519961495848290, 0.002780892266055755638, 0.003548264570615663419, 0.004315636875175571201, 0.004699323027455524875, 0.005083009179735478549, 0.005466695332015433090, 0.005850381484295386764, 0.006617753788855294111, 0.007385126093415201459, 0.008152498397975108807 ),
 ( 0.000000000000000000, 1.000000000000000000 ),
 .UNSPECIFIED. ) 
 GEOMETRIC_REPRESENTATION_ITEM ( )  RATIONAL_B_SPLINE_SURFACE ( (
 ( 1.000000000000000000, 0.7283825911960400967, 1.000000000000000000),
 ( 1.000000000000000000, 0.7404375345926941243, 1.000000000000000000),
 ( 1.000000000000000000, 0.7521483142436122815, 1.000000000000000000),
 ( 1.000000000000000000, 0.7744460733776301620, 1.000000000000000000),
 ( 1.000000000000000000, 0.7845612039380656100, 1.000000000000000000),
 ( 1.000000000000000000, 0.8022035258263469082, 1.000000000000000000),
 ( 1.000000000000000000, 0.8093965293321139232, 1.000000000000000000),
 ( 1.000000000000000000, 0.8169028692725751606, 1.000000000000000000),
 ( 1.000000000000000000, 0.8188329634862675510, 1.000000000000000000),
 ( 1.000000000000000000, 0.8214004505364708164, 1.000000000000000000),
 ( 1.000000000000000000, 0.8220602406261015016, 1.000000000000000000),
 ( 1.000000000000000000, 0.8220736605435605693, 1.000000000000000000),
 ( 1.000000000000000000, 0.8214126668415207000, 1.000000000000000000),
 ( 1.000000000000000000, 0.8188520474558780293, 1.000000000000000000),
 ( 1.000000000000000000, 0.8169545908333755158, 1.000000000000000000),
 ( 1.000000000000000000, 0.8094771004220964183, 1.000000000000000000),
 ( 1.000000000000000000, 0.8022723753809752889, 1.000000000000000000),
 ( 1.000000000000000000, 0.7845733350635248904, 1.000000000000000000),
 ( 1.000000000000000000, 0.7744472902493149125, 1.000000000000000000),
 ( 1.000000000000000000, 0.7522916829163579511, 1.000000000000000000),
 ( 1.000000000000000000, 0.7403553004665739401, 1.000000000000000000),
 ( 1.000000000000000000, 0.7283825911960407629, 1.000000000000000000) ) ) 
 REPRESENTATION_ITEM ( '' )  SURFACE ( )  );
#25594 = ORIENTED_EDGE ( 'NONE', *, *, #8121, .F. ) ;
#25595 = CARTESIAN_POINT ( 'NONE',  ( 0.2511799810870077310, -1.337738304023724512, -0.3144976166544468099 ) ) ;
#25596 = FACE_OUTER_BOUND ( 'NONE', #26165, .T. ) ;
#25597 = DIRECTION ( 'NONE',  ( 0.000000000000000000, 0.5365213554527455964, -0.8438867430782097667 ) ) ;
#25598 = ORIENTED_EDGE ( 'NONE', *, *, #1259, .T. ) ;
#25599 = CARTESIAN_POINT ( 'NONE',  ( 0.3208715077212234701, -1.182672892261233732, 0.4687417262808780127 ) ) ;
#25600 = CARTESIAN_POINT ( 'NONE',  ( 0.1669163231849704332, -1.368600478287528288, 0.6337086473961658362 ) ) ;
#25602 = EDGE_LOOP ( 'NONE', ( #1383, #7267, #40199, #23805 ) ) ;
#25601 = ORIENTED_EDGE ( 'NONE', *, *, #13558, .T. ) ;
#25603 = DIRECTION ( 'NONE',  ( 9.244463733058732095E-32, -0.1402348365094961968, -0.9901182710308678026 ) ) ;
#25604 = CYLINDRICAL_SURFACE ( 'NONE', #30932, 0.1000000000000000194 ) ;
#25605 = DIRECTION ( 'NONE',  ( 0.8660512985181133550, 0.4999551463232373982, 0.000000000000000000 ) ) ;
#25606 = ADVANCED_FACE ( 'NONE', ( #26081 ), #26369, .F. ) ;
#25607 = CARTESIAN_POINT ( 'NONE',  ( 0.04947837552028769292, 0.4418396724781423202, 0.1804413675089291402 ) ) ;
#25608 = CARTESIAN_POINT ( 'NONE',  ( -0.2399999999999999079, -3.840189043187996809, -0.1239867222638698224 ) ) ;
#25609 = ORIENTED_EDGE ( 'NONE', *, *, #8505, .F. ) ;
#25610 = CARTESIAN_POINT ( 'NONE',  ( 0.3098984767712536503, -1.765718780359063267, 0.5682417262808792113 ) ) ;
#25611 = VERTEX_POINT ( 'NONE', #797 ) ;
#25612 = CARTESIAN_POINT ( 'NONE',  ( 0.1991057831364872188, -0.8359650798049160780, 0.6453486718655260246 ) ) ;
#25613 = ORIENTED_EDGE ( 'NONE', *, *, #4117, .T. ) ;
#25614 = CARTESIAN_POINT ( 'NONE',  ( 0.02277869702299618881, -0.6155849950919007885, 0.5815368015377633260 ) ) ;
#25615 = CARTESIAN_POINT ( 'NONE',  ( 0.1228925711962478157, -0.7562269421748776255, 0.5887331513672725558 ) ) ;
#25617 = CARTESIAN_POINT ( 'NONE',  ( -0.1112012347075035518, -0.5082045352552144735, 0.3316257441459521949 ) ) ;
#25616 = CARTESIAN_POINT ( 'NONE',  ( 0.4243666725459965261, -1.591076223527387423, -0.4156371400837811647 ) ) ;
#25618 = CARTESIAN_POINT ( 'NONE',  ( 0.3139698647411150456, -1.647750188186495768, -0.3722908259404185127 ) ) ;
#25619 = CARTESIAN_POINT ( 'NONE',  ( 0.1875000000000002220, -0.9151275355372970877, 0.1608123706567810285 ) ) ;
#25620 = ORIENTED_EDGE ( 'NONE', *, *, #4920, .F. ) ;
#25621 = CARTESIAN_POINT ( 'NONE',  ( 0.1989976604547400996, -2.047409678865566018, -0.7132172901365276818 ) ) ;
#25622 = CARTESIAN_POINT ( 'NONE',  ( 0.1887412855916308085, -0.4595320686313653646, 0.1436109887884128300 ) ) ;
#25623 = CARTESIAN_POINT ( 'NONE',  ( 0.1718105009781868697, -0.7246503184330945757, 0.5294875450235927428 ) ) ;
#25624 = CARTESIAN_POINT ( 'NONE',  ( -0.05561176441985807989, 0.2541700551350232762, 0.3845131534397769890 ) ) ;
#25625 = FACE_OUTER_BOUND ( 'NONE', #33685, .T. ) ;
#25626 = EDGE_CURVE ( 'NONE', #36967, #10025, #19679, .T. ) ;
#25627 = APPLIED_PERSON_AND_ORGANIZATION_ASSIGNMENT ( #19184, #16111, ( #9595 ) ) ;
#25628 = DIRECTION ( 'NONE',  ( 0.000000000000000000, 0.000000000000000000, -1.000000000000000000 ) ) ;
#25629 = EDGE_CURVE ( 'NONE', #14919, #23555, #19152, .T. ) ;
#25630 = CARTESIAN_POINT ( 'NONE',  ( 0.1963745812722482442, -0.6060194383687296238, 0.2878283022669332891 ) ) ;
#25631 = EDGE_CURVE ( 'NONE', #28758, #40101, #29142, .T. ) ;
#25632 = CARTESIAN_POINT ( 'NONE',  ( 0.5111972025864910396, -1.114343631621611763, 0.5700687535673305550 ) ) ;
#25633 = CARTESIAN_POINT ( 'NONE',  ( 0.03810263172085913419, -1.166682418185958525, 0.6773769210087452475 ) ) ;
#25634 = AXIS2_PLACEMENT_3D ( 'NONE', #8231, #36810, #27573 ) ;
#25635 = CARTESIAN_POINT ( 'NONE',  ( 0.04946426091937942970, 0.4635716124040155650, -0.1136627969334498417 ) ) ;
#25636 = CARTESIAN_POINT ( 'NONE',  ( 0.1999999999999789724, -2.183180860297921466, -0.4937760292030871079 ) ) ;
#25637 = CARTESIAN_POINT ( 'NONE',  ( 0.4315008625312996560, -1.186182859931574685, 0.6815412659474554546 ) ) ;
#25638 = CARTESIAN_POINT ( 'NONE',  ( 0.04230188431063452298, 0.008729788072061312257, 0.4686063437799718456 ) ) ;
#25639 = B_SPLINE_CURVE_WITH_KNOTS ( 'NONE', 3,
 ( #36743, #6287, #30587, #33879, #24631, #37162 ),
 .UNSPECIFIED., .F., .F.,
 ( 4, 2, 4 ),
 ( 0.004447844280125260071, 0.005140701078120121607, 0.005833557876114983144 ),
 .UNSPECIFIED. ) ;
#25640 = CARTESIAN_POINT ( 'NONE',  ( 0.7031996424904172205, -1.495314321248880862, 0.5017627394515868922 ) ) ;
#25641 = AXIS2_PLACEMENT_3D ( 'NONE', #23883, #23282, #35804 ) ;
#25642 = ORIENTED_EDGE ( 'NONE', *, *, #7554, .F. ) ;
#25643 = DIRECTION ( 'NONE',  ( 0.000000000000000000, 0.000000000000000000, -1.000000000000000000 ) ) ;
#25644 = CARTESIAN_POINT ( 'NONE',  ( 0.5202166948571674832, -1.331060376252395816, 0.7806648288483002407 ) ) ;
#25645 = B_SPLINE_CURVE_WITH_KNOTS ( 'NONE', 3,
 ( #20251, #20439, #38950, #35452 ),
 .UNSPECIFIED., .F., .F.,
 ( 4, 4 ),
 ( 0.000000000000000000, 0.001408481125205278926 ),
 .UNSPECIFIED. ) ;
#25646 = CARTESIAN_POINT ( 'NONE',  ( -0.2600000000000003419, 0.5182417262804733804, 0.3749999999999999445 ) ) ;
#25647 = CARTESIAN_POINT ( 'NONE',  ( 0.3751813939980868096, -1.114089948641664440, 0.6058345290201684330 ) ) ;
#25648 = ORIENTED_EDGE ( 'NONE', *, *, #10680, .F. ) ;
#25649 = CARTESIAN_POINT ( 'NONE',  ( -0.1623927644724277586, 0.5045516355107052542, 0.3253307341376578954 ) ) ;
#25650 = CARTESIAN_POINT ( 'NONE',  ( 0.3317329491067714242, -1.291263278213948817, 0.4170592068404440633 ) ) ;
#25651 = CARTESIAN_POINT ( 'NONE',  ( 0.01548846960707511190, -0.5346638663566692928, 0.07572681171513533094 ) ) ;
#25652 = CARTESIAN_POINT ( 'NONE',  ( 0.3991893380402145586, -1.748812823822652129, -0.5227832640171824474 ) ) ;
#25653 = CARTESIAN_POINT ( 'NONE',  ( 0.4956954725223758351, -1.285442406743084964, 0.6670609216475702485 ) ) ;
#25654 = EDGE_CURVE ( 'NONE', #21190, #16265, #1422, .T. ) ;
#25656 = CARTESIAN_POINT ( 'NONE',  ( 0.2632752295237112405, -1.677058126094923329, 0.5210370874354662840 ) ) ;
#25655 = DIRECTION ( 'NONE',  ( 7.771561172376107616E-16, -7.170354002788761615E-17, 1.000000000000000000 ) ) ;
#25657 = CARTESIAN_POINT ( 'NONE',  ( 0.4929465528686921560, -1.082715557938388029, 0.5685663778595840823 ) ) ;
#25658 = ORIENTED_EDGE ( 'NONE', *, *, #31377, .T. ) ;
#25659 = SECURITY_CLASSIFICATION_LEVEL ( 'unclassified' ) ;
#25660 = CARTESIAN_POINT ( 'NONE',  ( 0.06254816942709211236, -1.140419159346305777, 0.7531148659283598557 ) ) ;
#25661 = ORIENTED_EDGE ( 'NONE', *, *, #39, .F. ) ;
#25662 = CARTESIAN_POINT ( 'NONE',  ( 0.3317989971924339421, -1.461076630628523665, 0.8685545625247669266 ) ) ;
#25664 = CARTESIAN_POINT ( 'NONE',  ( 0.1981136876533342028, -0.5988876534399234508, 0.3156152556879199267 ) ) ;
#25663 = CARTESIAN_POINT ( 'NONE',  ( 0.08572706863110483855, -0.8134827521777350245, 0.07519561625211983180 ) ) ;
#25665 = DIRECTION ( 'NONE',  ( 0.000000000000000000, -1.951319995474460317E-15, -1.000000000000000000 ) ) ;
#25666 = ORIENTED_EDGE ( 'NONE', *, *, #27291, .F. ) ;
#25667 = VECTOR ( 'NONE', #30230, 39.37007874015748854 ) ;
#25668 = ORIENTED_EDGE ( 'NONE', *, *, #8817, .T. ) ;
#25669 = VERTEX_POINT ( 'NONE', #26876 ) ;
#25670 = CYLINDRICAL_SURFACE ( 'NONE', #10971, 0.2000000000000000389 ) ;
#25671 = CARTESIAN_POINT ( 'NONE',  ( 0.5668833231537255823, -1.503228122861213878, 0.5723226605073136186 ) ) ;
#25672 = EDGE_LOOP ( 'NONE', ( #6659, #24287, #40252, #30822 ) ) ;
#25673 = CARTESIAN_POINT ( 'NONE',  ( 0.3838614819971074565, -1.826137710545491899, -0.5214446907161387479 ) ) ;
#25674 = DIRECTION ( 'NONE',  ( 1.000000000000000000, 0.000000000000000000, 0.000000000000000000 ) ) ;
#25675 = DIRECTION ( 'NONE',  ( 0.000000000000000000, -0.9510565162951545304, -0.3090169943749443426 ) ) ;
#25676 = CIRCLE ( 'NONE', #17118, 0.01499999999999999424 ) ;
#25677 = FACE_OUTER_BOUND ( 'NONE', #5900, .T. ) ;
#25678 = CARTESIAN_POINT ( 'NONE',  ( -0.3000000000000000999, -3.941790907013290823, -0.4709369376873030477 ) ) ;
#25679 = AXIS2_PLACEMENT_3D ( 'NONE', #40433, #24997, #9151 ) ;
#25680 = CARTESIAN_POINT ( 'NONE',  ( 0.03333333333331219700, -2.097675824466503691, -0.2588528740066097233 ) ) ;
#25681 = CARTESIAN_POINT ( 'NONE',  ( -0.1212602504878774051, -0.5073146173917496560, 0.1528658435937000626 ) ) ;
#25682 = DIRECTION ( 'NONE',  ( 0.4999551463232372317, -0.8660512985181134660, 0.000000000000000000 ) ) ;
#25683 = DIRECTION ( 'NONE',  ( 0.4999551463232372317, -0.8660512985181133550, 0.000000000000000000 ) ) ;
#25684 = DIRECTION ( 'NONE',  ( 0.3468893892380646715, 0.2594111197898561483, -0.9013177145509876365 ) ) ;
#25685 = CARTESIAN_POINT ( 'NONE',  ( 0.3391087009220875581, -1.665264393586757485, -0.3926146152733260286 ) ) ;
#25686 = PERSON_AND_ORGANIZATION ( #28500, #32463 ) ;
#25687 = DIRECTION ( 'NONE',  ( 0.000000000000000000, 3.330669073875470114E-16, 1.000000000000000000 ) ) ;
#25688 = CARTESIAN_POINT ( 'NONE',  ( -0.01548846960707463312, 0.2306506793134060762, 0.4716198300880322658 ) ) ;
#25689 = CARTESIAN_POINT ( 'NONE',  ( 0.5193158764790237747, -1.143105642405225053, 0.8514134314631569556 ) ) ;
#25690 = DIRECTION ( 'NONE',  ( 1.000000000000000000, 6.779273404243070203E-32, 4.314083075427408311E-32 ) ) ;
#25691 = CARTESIAN_POINT ( 'NONE',  ( 9.714451465470134135E-19, -6.434085166993905626E-18, -0.01750000000000000513 ) ) ;
#25692 = CARTESIAN_POINT ( 'NONE',  ( 0.2190338188766751681, -1.487106827364948147, 0.9008211596871106286 ) ) ;
#25693 = CARTESIAN_POINT ( 'NONE',  ( 0.0001425719452660938885, -0.5630222807798194173, -0.07015382250872513603 ) ) ;
#25694 = CARTESIAN_POINT ( 'NONE',  ( 0.4208428299034849274, -1.590742573860040920, -0.4148732612168254397 ) ) ;
#25695 = CIRCLE ( 'NONE', #37477, 0.1000000000000000194 ) ;
#25696 = DIRECTION ( 'NONE',  ( -0.4999999999999973910, -0.5006794435238203222, 0.7066258520834629575 ) ) ;
#25697 = ORIENTED_EDGE ( 'NONE', *, *, #38312, .T. ) ;
#25698 = VERTEX_POINT ( 'NONE', #17199 ) ;
#25699 = CARTESIAN_POINT ( 'NONE',  ( 0.3760351885562676078, -1.762179279381405061, -0.5696997652324907735 ) ) ;
#25700 = ORIENTED_EDGE ( 'NONE', *, *, #27504, .F. ) ;
#25701 = DIRECTION ( 'NONE',  ( -0.000000000000000000, -0.9343694307158671997, 0.3563057211773427713 ) ) ;
#25702 = DIRECTION ( 'NONE',  ( 1.000000000000000000, 0.000000000000000000, 0.000000000000000000 ) ) ;
#25703 = AXIS2_PLACEMENT_3D ( 'NONE', #15132, #17944, #26628 ) ;
#25704 = CARTESIAN_POINT ( 'NONE',  ( 0.5980105188037525554, -1.461600014062093722, 0.6143516452787856075 ) ) ;
#25706 = VERTEX_POINT ( 'NONE', #35928 ) ;
#25705 = FACE_OUTER_BOUND ( 'NONE', #6270, .T. ) ;
#25707 = ORIENTED_EDGE ( 'NONE', *, *, #23350, .T. ) ;
#25708 = CARTESIAN_POINT ( 'NONE',  ( 0.4149386519513223459, -1.589462803974980076, -0.6474370376047597908 ) ) ;
#25709 = VERTEX_POINT ( 'NONE', #29545 ) ;
#25710 = CARTESIAN_POINT ( 'NONE',  ( 0.2971099084452207273, -1.656645455338934481, 0.5725024039952387733 ) ) ;
#25712 = CARTESIAN_POINT ( 'NONE',  ( 0.2625876981780432828, -0.6796766824346859304, 0.2386862984125060760 ) ) ;
#25711 = CARTESIAN_POINT ( 'NONE',  ( 0.6480958352246775078, -1.555737386339220762, 0.4265722068199431227 ) ) ;
#25713 = CARTESIAN_POINT ( 'NONE',  ( 0.3174184176267851876, -1.762933076790994757, 0.5319023928052664107 ) ) ;
#25714 = CARTESIAN_POINT ( 'NONE',  ( 0.1856782277538235604, -0.8266995537623093027, 0.008518417185872217273 ) ) ;
#25715 = CARTESIAN_POINT ( 'NONE',  ( 0.03069864901531152435, -1.915872880763735742, -0.3084851516908380664 ) ) ;
#25717 = ORIENTED_EDGE ( 'NONE', *, *, #11664, .T. ) ;
#25716 = VERTEX_POINT ( 'NONE', #29746 ) ;
#25718 = AXIS2_PLACEMENT_3D ( 'NONE', #16602, #22987, #32641 ) ;
#25719 = CARTESIAN_POINT ( 'NONE',  ( 0.5399038930177495477, -1.667580954481910904, -0.5371941175943450997 ) ) ;
#25720 = CARTESIAN_POINT ( 'NONE',  ( 0.1947361823824516613, -0.9199698176769123270, 0.2890873638243558474 ) ) ;
#25721 = B_SPLINE_CURVE_WITH_KNOTS ( 'NONE', 3,
 ( #8405, #17665, #30030, #21172, #10906, #1663, #26749, #24264, #23475, #23660 ),
 .UNSPECIFIED., .F., .F.,
 ( 4, 2, 2, 2, 4 ),
 ( 0.000000000000000000, 0.0006458916093408944735, 0.001291783218681788947, 0.001937674828022683312, 0.002583566437363577894 ),
 .UNSPECIFIED. ) ;
#25722 = CARTESIAN_POINT ( 'NONE',  ( -0.04154009738085504000, 0.01731731106881310295, -0.4700109389422700845 ) ) ;
#25723 = CARTESIAN_POINT ( 'NONE',  ( 0.5614343097231884183, -1.437874780063664426, 0.7463454611595057298 ) ) ;
#25724 = CARTESIAN_POINT ( 'NONE',  ( 0.1315959483921021189, -0.8604525307240751264, 0.4681842845926359464 ) ) ;
#25725 = DIRECTION ( 'NONE',  ( -4.930380657631319405E-32, 0.5237184928541299689, -0.8518913899333638851 ) ) ;
#25726 = AXIS2_PLACEMENT_3D ( 'NONE', #32470, #15277, #27832 ) ;
#25727 = CARTESIAN_POINT ( 'NONE',  ( 0.1810308432981227733, -0.8729890291813854342, 0.1457080207793099436 ) ) ;
#25728 = VECTOR ( 'NONE', #8401, 39.37007874015748143 ) ;
#25729 = DIRECTION ( 'NONE',  ( -0.6278132875326316586, 0.7783639739848378092, 0.000000000000000000 ) ) ;
#25730 = AXIS2_PLACEMENT_3D ( 'NONE', #23740, #5393, #8083 ) ;
#25731 = CARTESIAN_POINT ( 'NONE',  ( 0.3249483201304784741, -1.768002432019315728, 0.5182417262812728520 ) ) ;
#25732 = CARTESIAN_POINT ( 'NONE',  ( 0.03650581953630612636, 0.5059763899182371238, 0.07647306779615405115 ) ) ;
#25733 = CARTESIAN_POINT ( 'NONE',  ( 0.1625982857068778153, -0.6782215948270849948, 0.2386756342038218459 ) ) ;
#25734 = DIRECTION ( 'NONE',  ( 0.000000000000000000, 0.000000000000000000, 1.000000000000000000 ) ) ;
#25735 = CIRCLE ( 'NONE', #24414, 0.01999999999999927530 ) ;
#25736 = AXIS2_PLACEMENT_3D ( 'NONE', #16693, #19769, #38283 ) ;
#25737 = CARTESIAN_POINT ( 'NONE',  ( 0.04762035657658286042, -0.3170509070583802935, 0.3633072608571672468 ) ) ;
#25738 = ADVANCED_FACE ( 'NONE', ( #23193 ), #38786, .T. ) ;
#25739 = CARTESIAN_POINT ( 'NONE',  ( 0.01602427940967538628, -0.5690816651727684805, 0.5319142476028417832 ) ) ;
#25740 = CARTESIAN_POINT ( 'NONE',  ( 0.1173773673404726187, -1.400925278984374689, 0.6274554870938690021 ) ) ;
#25741 = EDGE_CURVE ( 'NONE', #23612, #31054, #14317, .T. ) ;
#25742 = DATE_AND_TIME ( #13171, #3031 ) ;
#25743 = CARTESIAN_POINT ( 'NONE',  ( 0.4226000438817392180, -1.709616762427842218, 0.4282184315516496809 ) ) ;
#25744 = CARTESIAN_POINT ( 'NONE',  ( 0.3740582401036630644, -1.700298052928095549, -0.6903158886021862894 ) ) ;
#25745 = EDGE_CURVE ( 'NONE', #3583, #16852, #20696, .T. ) ;
#25746 = CARTESIAN_POINT ( 'NONE',  ( -0.05561310505367114687, 0.4442420632723341201, 0.1228816621031162265 ) ) ;
#25747 = CIRCLE ( 'NONE', #32979, 2.001674066779353556 ) ;
#25748 = CARTESIAN_POINT ( 'NONE',  ( 0.1424029337235096226, -1.400533250147911746, -0.3244367222852112542 ) ) ;
#25749 = EDGE_CURVE ( 'NONE', #8719, #23287, #29055, .T. ) ;
#25750 = B_SPLINE_CURVE_WITH_KNOTS ( 'NONE', 3,
 ( #24779, #14470, #11799, #30318, #8314, #39979, #11401 ),
 .UNSPECIFIED., .F., .F.,
 ( 4, 3, 4 ),
 ( 2.353093408709756909E-17, 3.509865184711082858E-06, 6.918258478235508878E-06 ),
 .UNSPECIFIED. ) ;
#25751 = ORIENTED_EDGE ( 'NONE', *, *, #3328, .F. ) ;
#25752 = CARTESIAN_POINT ( 'NONE',  ( 0.4772201074466940196, -1.128262804531645402, 0.4802508068224435878 ) ) ;
#25753 = EDGE_LOOP ( 'NONE', ( #2173, #33144, #26884, #20879 ) ) ;
#25754 = CARTESIAN_POINT ( 'NONE',  ( 0.1121769144737377738, -1.416522762178338279, 0.5260910154307498754 ) ) ;
#25755 = CARTESIAN_POINT ( 'NONE',  ( -0.2399999999999999079, -2.341127044584462968, -0.9908042926600856282 ) ) ;
#25756 = AXIS2_PLACEMENT_3D ( 'NONE', #1260, #13579, #10080 ) ;
#25757 = CARTESIAN_POINT ( 'NONE',  ( 0.5698225495787666572, -1.450209349364527389, 0.7310466856332464847 ) ) ;
#25759 = ORIENTED_EDGE ( 'NONE', *, *, #24263, .T. ) ;
#25758 = DIRECTION ( 'NONE',  ( -8.881784197001246407E-16, 2.361472542561082612E-16, -1.000000000000000000 ) ) ;
#25761 = ORIENTED_EDGE ( 'NONE', *, *, #21625, .T. ) ;
#25760 = ORIENTED_EDGE ( 'NONE', *, *, #21085, .F. ) ;
#25762 = DIRECTION ( 'NONE',  ( 0.4999551463232377313, -0.8660512985181132439, -0.000000000000000000 ) ) ;
#25763 = AXIS2_PLACEMENT_3D ( 'NONE', #30771, #18414, #4901 ) ;
#25764 = VERTEX_POINT ( 'NONE', #7308 ) ;
#25765 = CIRCLE ( 'NONE', #39532, 0.1699999999999999845 ) ;
#25766 = EDGE_CURVE ( 'NONE', #25255, #990, #39004, .T. ) ;
#25767 = LINE ( 'NONE', #18403, #119 ) ;
#25768 = PRODUCT_DEFINITION ( 'UNKNOWN', '', #30575, #22066 ) ;
#25769 = CARTESIAN_POINT ( 'NONE',  ( -0.1710642718812833418, 0.4986889572247755753, 0.1528658435937000626 ) ) ;
#25770 = APPROVAL_ROLE ( '' ) ;
#25771 = CONICAL_SURFACE ( 'NONE', #4736, 0.01999999999999927530, 1.047197551196601184 ) ;
#25772 = CARTESIAN_POINT ( 'NONE',  ( 0.05999999999999990757, 0.1428018198284763673, -0.2638325989215043466 ) ) ;
#25773 = ORIENTED_EDGE ( 'NONE', *, *, #31035, .T. ) ;
#25774 = CARTESIAN_POINT ( 'NONE',  ( 0.2669582311511931594, -0.9789240833730817881, 0.6944203207930329524 ) ) ;
#25775 = B_SPLINE_SURFACE_WITH_KNOTS ( 'NONE', 3, 3, ( 
 ( #28951, #22999, #12715, #38416 ),
 ( #34724, #31643, #28563, #25483 ),
 ( #25277, #22207, #10251, #29162 ),
 ( #38019, #22820, #32231, #35341 ),
 ( #7130, #22400, #13536, #19310 ),
 ( #20932, #36552, #13913, #36340 ),
 ( #17429, #14334, #35948, #7754 ) ),
 .UNSPECIFIED., .F., .F., .F.,
 ( 4, 3, 4 ),
 ( 4, 4 ),
 ( -3.173847279484519390, -0.01167112848645035506, 3.150505022511618680 ),
 ( -1.323227062466913795, 1.838851490560286184 ),
 .UNSPECIFIED. ) ;
#25776 = CARTESIAN_POINT ( 'NONE',  ( 0.06924657340762380153, -0.5400045880099016982, 0.1389823447417335711 ) ) ;
#25777 = CARTESIAN_POINT ( 'NONE',  ( 0.5386835852938653968, -1.518924006319621434, 0.5659150387024363127 ) ) ;
#25778 = ORIENTED_EDGE ( 'NONE', *, *, #14283, .F. ) ;
#25779 = CARTESIAN_POINT ( 'NONE',  ( 0.6379434532176896377, -1.610984557999281419, -0.4725373545200265979 ) ) ;
#25780 = CARTESIAN_POINT ( 'NONE',  ( -0.1608166228773026118, 0.4995225507409988275, 0.1237952727409415976 ) ) ;
#25781 = CARTESIAN_POINT ( 'NONE',  ( -0.1589779575897101449, 0.4935643744415435519, 0.1021333108076154655 ) ) ;
#25782 = DIRECTION ( 'NONE',  ( 0.9378410757839514833, 0.2807814858886687470, 0.2039996905746478406 ) ) ;
#25783 = CARTESIAN_POINT ( 'NONE',  ( 0.6835936161259937860, -1.406830003848978050, 0.7131562199467919028 ) ) ;
#25784 = CARTESIAN_POINT ( 'NONE',  ( 0.4738838377074015562, -1.632444973519838971, -0.6081242360855458884 ) ) ;
#25785 = CARTESIAN_POINT ( 'NONE',  ( 0.1727685491708599863, -0.7001921779997841710, 0.4913863249289630031 ) ) ;
#25786 = CARTESIAN_POINT ( 'NONE',  ( 0.03654364704248813656, -0.5058694728073483970, 0.07650507870000912425 ) ) ;
#25787 = SHAPE_REPRESENTATION_RELATIONSHIP ( 'NONE' , 'NONE' ,  #17542, #14726 ) ;
#25788 = CONICAL_SURFACE ( 'NONE', #8019, 0.4615209409081865166, 1.047197551196600740 ) ;
#25789 = DIRECTION ( 'NONE',  ( 0.000000000000000000, 0.000000000000000000, 1.000000000000000000 ) ) ;
#25790 = CARTESIAN_POINT ( 'NONE',  ( 0.4631130424841433668, -1.102114521487385757, -0.3875800985506998031 ) ) ;
#25791 = CARTESIAN_POINT ( 'NONE',  ( 6.608588869366793274E-05, -0.9486129085773968850, 0.1942756810714297844 ) ) ;
#25792 = CARTESIAN_POINT ( 'NONE',  ( 0.4930347527585871026, -1.093336683456308078, 0.6301225560750347565 ) ) ;
#25793 = EDGE_CURVE ( 'NONE', #19197, #27945, #10616, .T. ) ;
#25794 = SECURITY_CLASSIFICATION_LEVEL ( 'unclassified' ) ;
#25795 = AXIS2_PLACEMENT_3D ( 'NONE', #9071, #37870, #6782 ) ;
#25796 = AXIS2_PLACEMENT_3D ( 'NONE', #38069, #28209, #34984 ) ;
#25797 = DIRECTION ( 'NONE',  ( 0.000000000000000000, 8.195543980992787683E-15, -1.000000000000000000 ) ) ;
#25798 = AXIS2_PLACEMENT_3D ( 'NONE', #17095, #4343, #26573 ) ;
#25799 = ADVANCED_FACE ( 'NONE', ( #19886 ), #27072, .T. ) ;
#25800 = B_SPLINE_CURVE_WITH_KNOTS ( 'NONE', 3,
 ( #9142, #12436, #18212, #21317 ),
 .UNSPECIFIED., .F., .F.,
 ( 4, 4 ),
 ( 1.058749929371489123E-17, 0.0008450547985826826515 ),
 .UNSPECIFIED. ) ;
#25801 = CARTESIAN_POINT ( 'NONE',  ( -0.01548846960712776770, 0.5203207976466729390, -0.08861466064782422269 ) ) ;
#25802 = EDGE_CURVE ( 'NONE', #38544, #23685, #18518, .T. ) ;
#25803 = CARTESIAN_POINT ( 'NONE',  ( -0.05138886601528163539, 0.02227547295149007178, 0.4715784802958499777 ) ) ;
#25804 = ORIENTED_EDGE ( 'NONE', *, *, #23769, .F. ) ;
#25805 = CARTESIAN_POINT ( 'NONE',  ( 0.1796683189498666788, -1.379020643267101498, -0.3452591383903352851 ) ) ;
#25806 = CARTESIAN_POINT ( 'NONE',  ( 0.002379513690175749652, -0.5300039046122766440, 0.1723549453226513595 ) ) ;
#25807 = CARTESIAN_POINT ( 'NONE',  ( 0.1855767734282748604, -0.8171754376128953501, 0.2578515647343493922 ) ) ;
#25808 = VERTEX_POINT ( 'NONE', #1384 ) ;
#25809 = CARTESIAN_POINT ( 'NONE',  ( 0.01548846960707511190, -0.09061086148576411037, -0.5171215251571027460 ) ) ;
#25810 = CARTESIAN_POINT ( 'NONE',  ( 0.6742391038958878147, -1.391540648348956966, 0.6661449684938977045 ) ) ;
#25812 = ORIENTED_EDGE ( 'NONE', *, *, #17128, .F. ) ;
#25811 = ORIENTED_EDGE ( 'NONE', *, *, #39551, .T. ) ;
#25813 = DIRECTION ( 'NONE',  ( 0.000000000000000000, -0.5877852522924708056, 0.8090169943749491166 ) ) ;
#25814 = ORIENTED_EDGE ( 'NONE', *, *, #274, .T. ) ;
#25815 = DIRECTION ( 'NONE',  ( 1.000000000000000000, -0.000000000000000000, -0.000000000000000000 ) ) ;
#25816 = EDGE_CURVE ( 'NONE', #21695, #30066, #31976, .T. ) ;
#25817 = CARTESIAN_POINT ( 'NONE',  ( 0.5902548269665799374, -1.489241228028834296, 0.5558766452402442715 ) ) ;
#25818 = CIRCLE ( 'NONE', #31060, 0.1400000000000013456 ) ;
#25819 = CARTESIAN_POINT ( 'NONE',  ( 0.04285427992854216883, -0.2295125098185414325, -0.4383721679652327619 ) ) ;
#25820 = ORIENTED_EDGE ( 'NONE', *, *, #8878, .F. ) ;
#25821 = CARTESIAN_POINT ( 'NONE',  ( 0.6315986430998083989, -1.581773586513405716, 0.5682417262808788783 ) ) ;
#25822 = CARTESIAN_POINT ( 'NONE',  ( 0.1488906047797098897, -0.7556912933748931582, 0.5388018373693193031 ) ) ;
#25823 = AXIS2_PLACEMENT_3D ( 'NONE', #7806, #1868, #20376 ) ;
#25824 = CARTESIAN_POINT ( 'NONE',  ( 2.583436045986187992E-05, -0.4262564429027325685, 0.1457185332388686583 ) ) ;
#25825 = VECTOR ( 'NONE', #24695, 39.37007874015748143 ) ;
#25826 = CARTESIAN_POINT ( 'NONE',  ( 0.09071160229062831537, -0.5913197634106368561, 0.3153209778789223261 ) ) ;
#25828 = CYLINDRICAL_SURFACE ( 'NONE', #18954, 0.08139150547213669373 ) ;
#25827 = CARTESIAN_POINT ( 'NONE',  ( 0.4390726440607947700, -1.640987763579620617, -0.4103404039523522728 ) ) ;
#25829 = CARTESIAN_POINT ( 'NONE',  ( 0.6252338399778394340, -1.468100857423625838, 0.5182417262812428760 ) ) ;
#25830 = CARTESIAN_POINT ( 'NONE',  ( 0.1450424297082592573, -0.9270031065346044929, 0.2652761459977906466 ) ) ;
#25831 = ORIENTED_EDGE ( 'NONE', *, *, #7908, .T. ) ;
#25832 = AXIS2_PLACEMENT_3D ( 'NONE', #7208, #35224, #19773 ) ;
#25833 = DIRECTION ( 'NONE',  ( -0.5415634522278134355, 0.8406598760563588346, 0.000000000000000000 ) ) ;
#25834 = CARTESIAN_POINT ( 'NONE',  ( 0.1153477709767999210, -0.4466080377581258531, 0.1487152767197887637 ) ) ;
#25835 = CARTESIAN_POINT ( 'NONE',  ( -0.03309057659885149272, 0.3730661755626945020, 0.3633900220890601274 ) ) ;
#25836 = AXIS2_PLACEMENT_3D ( 'NONE', #27310, #5865, #37161 ) ;
#25837 = DIRECTION ( 'NONE',  ( 0.000000000000000000, 0.000000000000000000, -1.000000000000000000 ) ) ;
#25838 = CARTESIAN_POINT ( 'NONE',  ( -0.02000000000000000042, -2.177105168660885326, -0.3918349584362407212 ) ) ;
#25839 =( REPRESENTATION_RELATIONSHIP ('NONE','NONE', #27514, #33020 ) REPRESENTATION_RELATIONSHIP_WITH_TRANSFORMATION ( #14219 )SHAPE_REPRESENTATION_RELATIONSHIP( ) );
#25840 = EDGE_LOOP ( 'NONE', ( #17092, #25666, #30773, #18936 ) ) ;
#25841 = CARTESIAN_POINT ( 'NONE',  ( 0.6085831598237441131, -1.284018499374271371, 0.7837445821806681145 ) ) ;
#25842 = EDGE_CURVE ( 'NONE', #38396, #13846, #9975, .T. ) ;
#25843 =( BOUNDED_SURFACE ( )  B_SPLINE_SURFACE ( 3, 2, ( 
 ( #22043, #6565, #31680 ),
 ( #18519, #25523, #15644 ),
 ( #3501, #476, #27789 ),
 ( #34570, #5959, #28192 ) ),
 .UNSPECIFIED., .F., .F., .T. ) 
 B_SPLINE_SURFACE_WITH_KNOTS ( ( 4, 4 ),
 ( 3, 3 ),
 ( 0.001168341556843763198, 0.001551611072815416289 ),
 ( 0.000000000000000000, 1.000000000000000000 ),
 .UNSPECIFIED. ) 
 GEOMETRIC_REPRESENTATION_ITEM ( )  RATIONAL_B_SPLINE_SURFACE ( (
 ( 1.000000000000000000, 0.8989970956543276159, 1.000000000000000000),
 ( 1.000000000000000000, 0.8989738193133679500, 1.000000000000000000),
 ( 1.000000000000000000, 0.9033319494950450279, 1.000000000000000000),
 ( 1.000000000000000000, 0.9117915798252654858, 1.000000000000000000) ) ) 
 REPRESENTATION_ITEM ( '' )  SURFACE ( )  );
#25844 = CARTESIAN_POINT ( 'NONE',  ( 0.4663844447009264371, -1.139904246673989707, 0.4152358672995193900 ) ) ;
#25845 = CARTESIAN_POINT ( 'NONE',  ( 0.05683680956318425820, -1.285974083448843563, 0.6485881297286527625 ) ) ;
#25846 = AXIS2_PLACEMENT_3D ( 'NONE', #14185, #20368, #1859 ) ;
#25847 = EDGE_CURVE ( 'NONE', #23287, #13015, #11353, .T. ) ;
#25848 = CARTESIAN_POINT ( 'NONE',  ( 0.03474878377841050109, 0.4640666366555413203, -0.2268437812334264392 ) ) ;
#25849 = DIRECTION ( 'NONE',  ( 1.000000000000000000, 0.000000000000000000, 0.000000000000000000 ) ) ;
#25850 = ORIENTED_EDGE ( 'NONE', *, *, #23073, .T. ) ;
#25851 = CARTESIAN_POINT ( 'NONE',  ( 0.1931882296960396594, -0.9271356228379165065, 0.6359237722107926594 ) ) ;
#25852 = CARTESIAN_POINT ( 'NONE',  ( 0.000000000000000000, 0.000000000000000000, 0.000000000000000000 ) ) ;
#25853 = DIRECTION ( 'NONE',  ( 8.326672684688655318E-16, -2.361472542561083598E-16, 1.000000000000000000 ) ) ;
#25854 = AXIS2_PLACEMENT_3D ( 'NONE', #33462, #33892, #5269 ) ;
#25855 = CIRCLE ( 'NONE', #7466, 0.5543128707267515054 ) ;
#25856 = ORIENTED_EDGE ( 'NONE', *, *, #40410, .F. ) ;
#25857 = EDGE_CURVE ( 'NONE', #24860, #4952, #20490, .T. ) ;
#25858 = CARTESIAN_POINT ( 'NONE',  ( -2.112273405726188513E-14, -2.183180860297921466, -0.4937760292030871079 ) ) ;
#25859 = CARTESIAN_POINT ( 'NONE',  ( 0.4099162622095676722, -1.645682601181238436, -0.3971641022030795165 ) ) ;
#25860 = CARTESIAN_POINT ( 'NONE',  ( 0.3178512907186139547, -1.645949601790900774, 0.6057417262800831592 ) ) ;
#25861 = CARTESIAN_POINT ( 'NONE',  ( 0.3832417524780237228, -1.109934760635944651, 0.6055797275786368727 ) ) ;
#25862 = CIRCLE ( 'NONE', #37676, 0.04999999999999994726 ) ;
#25863 = ORIENTED_EDGE ( 'NONE', *, *, #34778, .F. ) ;
#25864 = CARTESIAN_POINT ( 'NONE',  ( -0.1684323895664757431, 0.5231977504175445715, 0.3032895567580804475 ) ) ;
#25865 = ADVANCED_FACE ( 'NONE', ( #4835 ), #13894, .T. ) ;
#25866 = VECTOR ( 'NONE', #8100, 39.37007874015748143 ) ;
#25867 = CARTESIAN_POINT ( 'NONE',  ( 0.1157172991699309123, -1.415943335782397616, 0.5180376455024461313 ) ) ;
#25868 = DIRECTION ( 'NONE',  ( 0.000000000000000000, 0.000000000000000000, -1.000000000000000000 ) ) ;
#25869 = EDGE_CURVE ( 'NONE', #23808, #14594, #36244, .T. ) ;
#25870 = CARTESIAN_POINT ( 'NONE',  ( -0.2746410161513779258, -2.761122741982423801, -0.2878817176880067996 ) ) ;
#25871 = CARTESIAN_POINT ( 'NONE',  ( 0.4903088652999874064, -1.276544129464578292, 0.5957393316629001623 ) ) ;
#25873 = CARTESIAN_POINT ( 'NONE',  ( 0.3122977225021427161, -1.758414370883746303, 0.5144731769190049597 ) ) ;
#25872 = CARTESIAN_POINT ( 'NONE',  ( -0.05464101615137769569, -2.274798198814180772, -0.3601501197397404264 ) ) ;
#25874 = CARTESIAN_POINT ( 'NONE',  ( 0.3310978894898223834, -0.9939147606493616838, 0.5922533870212514095 ) ) ;
#25875 = ORIENTED_EDGE ( 'NONE', *, *, #8194, .F. ) ;
#25876 = ADVANCED_FACE ( 'NONE', ( #18006 ), #15373, .F. ) ;
#25877 = CALENDAR_DATE ( 2026, 13, 10 ) ;
#25878 = CARTESIAN_POINT ( 'NONE',  ( -0.0007573580111799426817, -0.8643563613948842539, 0.3275742400162479084 ) ) ;
#25879 = ORIENTED_EDGE ( 'NONE', *, *, #27788, .F. ) ;
#25880 = CARTESIAN_POINT ( 'NONE',  ( 0.04837608321400507089, -0.5516968865674545253, 0.2272918774305557610 ) ) ;
#25882 = CARTESIAN_POINT ( 'NONE',  ( 0.1844539022421386454, -0.8492542210929743263, 0.1057280673965992485 ) ) ;
#25881 = CARTESIAN_POINT ( 'NONE',  ( 0.06467744696527351345, -0.8310922711372544791, 0.1095653288593454594 ) ) ;
#25883 = DIRECTION ( 'NONE',  ( -1.000000000000000000, 0.000000000000000000, 0.000000000000000000 ) ) ;
#25884 = ORIENTED_EDGE ( 'NONE', *, *, #14670, .T. ) ;
#25885 = CARTESIAN_POINT ( 'NONE',  ( 0.3291383425727634204, -1.292725137034694605, 0.5718629676982472931 ) ) ;
#25886 = CARTESIAN_POINT ( 'NONE',  ( 0.2320287850415546360, -0.8916748044001994167, 0.6999815254931482933 ) ) ;
#25887 = ORIENTED_EDGE ( 'NONE', *, *, #38868, .T. ) ;
#25888 = CARTESIAN_POINT ( 'NONE',  ( 0.1874542073597142144, -0.6896383861170264362, 0.05662353690727370270 ) ) ;
#25889 = B_SPLINE_CURVE_WITH_KNOTS ( 'NONE', 3,
 ( #30595, #14955, #27509, #39635, #36563, #40033 ),
 .UNSPECIFIED., .F., .F.,
 ( 4, 2, 4 ),
 ( 0.000000000000000000, 0.0008310496493514948207, 0.001662099298702989641 ),
 .UNSPECIFIED. ) ;
#25890 = CARTESIAN_POINT ( 'NONE',  ( 0.5431141991461047036, -1.169197578686003824, 0.5740594486805935537 ) ) ;
#25891 = AXIS2_PLACEMENT_3D ( 'NONE', #16526, #10549, #22924 ) ;
#25892 = CIRCLE ( 'NONE', #12102, 0.1333070866141734534 ) ;
#25893 = CARTESIAN_POINT ( 'NONE',  ( 0.3031943397128461504, -1.538683866714745996, -0.7284286296668287530 ) ) ;
#25894 = DIRECTION ( 'NONE',  ( -0.4999999999999970024, 0.7723146731083251337, 0.3918291026730708615 ) ) ;
#25895 = CARTESIAN_POINT ( 'NONE',  ( 0.4694587393328914504, -1.673455684603170290, 0.5834458924043449679 ) ) ;
#25896 = CARTESIAN_POINT ( 'NONE',  ( 0.1223045647424210181, -1.412159682085746271, 0.4849083929475432320 ) ) ;
#25897 = AXIS2_PLACEMENT_3D ( 'NONE', #27706, #40239, #37551 ) ;
#25898 = CARTESIAN_POINT ( 'NONE',  ( 0.6069176374591634948, -1.480164522464830990, 0.5706138896049881559 ) ) ;
#25899 = CARTESIAN_POINT ( 'NONE',  ( 0.1049118822781112403, -1.346279903101843534, -0.6713530932235223236 ) ) ;
#25900 = AXIS2_PLACEMENT_3D ( 'NONE', #16076, #22259, #28620 ) ;
#25901 = CARTESIAN_POINT ( 'NONE',  ( 0.3222894045021684195, -1.758215778056678724, 0.5682417262808792113 ) ) ;
#25902 = DIRECTION ( 'NONE',  ( 1.000000000000000000, 0.000000000000000000, 0.000000000000000000 ) ) ;
#25903 = DATE_AND_TIME ( #29380, #22696 ) ;
#25904 = EDGE_CURVE ( 'NONE', #8729, #354, #33437, .T. ) ;
#25905 = CARTESIAN_POINT ( 'NONE',  ( 0.6376027386425543453, -1.480971300301067384, -0.6353011510804285056 ) ) ;
#25906 = CYLINDRICAL_SURFACE ( 'NONE', #33807, 0.03749999999977545601 ) ;
#25907 = DIRECTION ( 'NONE',  ( -1.000000000000000000, -0.000000000000000000, -0.000000000000000000 ) ) ;
#25908 = EDGE_CURVE ( 'NONE', #12637, #2424, #35911, .T. ) ;
#25909 = LINE ( 'NONE', #32240, #33665 ) ;
#25910 = PLANE ( 'NONE',  #21238 ) ;
#25911 = CARTESIAN_POINT ( 'NONE',  ( 0.07933644511000853550, -0.9611106349790075054, 0.8249633512138372371 ) ) ;
#25912 = CARTESIAN_POINT ( 'NONE',  ( -6.654766911438814885E-05, -0.7522227857163925613, -0.09490634037222707431 ) ) ;
#25913 = AXIS2_PLACEMENT_3D ( 'NONE', #7300, #6913, #10223 ) ;
#25914 = CARTESIAN_POINT ( 'NONE',  ( 0.02999923155047439643, -2.091072551548296854, -0.2612331489864342937 ) ) ;
#25915 = CARTESIAN_POINT ( 'NONE',  ( 0.5605867575437351036, -1.621001144914625991, -0.5473203437262892379 ) ) ;
#25916 = CARTESIAN_POINT ( 'NONE',  ( 0.3030236983578167842, -1.192445529317704978, 0.4282496583016260905 ) ) ;
#25917 = VERTEX_POINT ( 'NONE', #2785 ) ;
#25918 = AXIS2_PLACEMENT_3D ( 'NONE', #2820, #37370, #9181 ) ;
#25919 = VERTEX_POINT ( 'NONE', #24813 ) ;
#25920 = AXIS2_PLACEMENT_3D ( 'NONE', #16384, #28925, #13300 ) ;
#25921 = DIRECTION ( 'NONE',  ( 0.000000000000000000, 0.000000000000000000, -1.000000000000000000 ) ) ;
#25922 = ORIENTED_EDGE ( 'NONE', *, *, #16449, .T. ) ;
#25923 = CARTESIAN_POINT ( 'NONE',  ( 0.01548846960703768524, -0.2306506793134120714, -0.4716198300880298233 ) ) ;
#25924 = CARTESIAN_POINT ( 'NONE',  ( 0.5887170121326058547, -1.595259432128637966, -0.4420053674003829314 ) ) ;
#25925 = CARTESIAN_POINT ( 'NONE',  ( 0.4528193024337852091, -1.225745371163585062, 0.7904948860725230508 ) ) ;
#25927 = VERTEX_POINT ( 'NONE', #27292 ) ;
#25926 = CARTESIAN_POINT ( 'NONE',  ( 0.5708999571285244823, -1.624164834895633236, 0.4874694594315064911 ) ) ;
#25928 = CARTESIAN_POINT ( 'NONE',  ( 0.5556676709287090565, -1.190831894458023177, 0.5757950255497361614 ) ) ;
#25929 = AXIS2_PLACEMENT_3D ( 'NONE', #22154, #21720, #37962 ) ;
#25930 = CARTESIAN_POINT ( 'NONE',  ( 0.3365096318212707494, -1.698808709566205444, -0.6091315585829111257 ) ) ;
#25931 = EDGE_LOOP ( 'NONE', ( #40244, #8309 ) ) ;
#25932 = CARTESIAN_POINT ( 'NONE',  ( 0.5947987396514448077, -1.485632953921246946, -0.6449812926602518370 ) ) ;
#25933 = ORIENTED_EDGE ( 'NONE', *, *, #21227, .T. ) ;
#25934 = VECTOR ( 'NONE', #28565, 39.37007874015748854 ) ;
#25935 = CARTESIAN_POINT ( 'NONE',  ( 0.2942755186928532329, -1.617995445140106403, 0.7842711939927167197 ) ) ;
#25937 = CARTESIAN_POINT ( 'NONE',  ( 0.1115213762701100647, -0.8962530768969190209, 0.02490635507620986289 ) ) ;
#25936 = CARTESIAN_POINT ( 'NONE',  ( 0.6462138998544783020, -1.567979845271513240, 0.4257847868880864084 ) ) ;
#25938 = CARTESIAN_POINT ( 'NONE',  ( -0.05464101615137762630, -2.032088213807425880, -0.4352898549974345555 ) ) ;
#25939 = CARTESIAN_POINT ( 'NONE',  ( 0.4952038534613475429, -1.196867906360179257, -0.6186948529734399571 ) ) ;
#25940 = LINE ( 'NONE', #23043, #23797 ) ;
#25941 = VERTEX_POINT ( 'NONE', #11833 ) ;
#25942 = FACE_OUTER_BOUND ( 'NONE', #36813, .T. ) ;
#25943 = CARTESIAN_POINT ( 'NONE',  ( 0.1893785600340663899, -0.9170734978138452842, 0.2340385483544073775 ) ) ;
#25944 = DIRECTION ( 'NONE',  ( 0.4999999999999997224, 6.656013887802294115E-31, 0.8660254037844388186 ) ) ;
#25945 = CARTESIAN_POINT ( 'NONE',  ( -0.2746410161513779258, -3.970782550070895311, -0.6634248229925526763 ) ) ;
#25946 = CARTESIAN_POINT ( 'NONE',  ( 0.1094640939228022636, -0.8354574151733522580, 0.3143190699821967748 ) ) ;
#25947 = CARTESIAN_POINT ( 'NONE',  ( 0.09725169381387938072, -1.017893544929620919, 0.8399287296596764651 ) ) ;
#25948 = VECTOR ( 'NONE', #13406, 39.37007874015748143 ) ;
#25949 = CARTESIAN_POINT ( 'NONE',  ( 0.4974456442574145543, -1.184401136727553094, 0.4224083929475455079 ) ) ;
#25950 = CIRCLE ( 'NONE', #3569, 0.1620173459747806799 ) ;
#25951 = CIRCLE ( 'NONE', #35790, 0.5400000000000012568 ) ;
#25952 = CARTESIAN_POINT ( 'NONE',  ( 0.4627725426138175058, -1.215611893628281592, 0.5482364631202992777 ) ) ;
#25953 = DIRECTION ( 'NONE',  ( 1.000000000000000000, 6.779273404243070203E-32, 4.314083075427408311E-32 ) ) ;
#25954 = CIRCLE ( 'NONE', #23978, 0.01500000000000004628 ) ;
#25955 = DIRECTION ( 'NONE',  ( 0.000000000000000000, 0.1725921171159214285, -0.9849933812515919707 ) ) ;
#25956 = DIRECTION ( 'NONE',  ( 5.551115123125790098E-17, -3.676620095425088700E-16, -1.000000000000000000 ) ) ;
#25957 = DIRECTION ( 'NONE',  ( 1.000000000000000000, 0.000000000000000000, 0.000000000000000000 ) ) ;
#25958 = LOCAL_TIME ( 0, 53, 7.000000000000000000, #10260 ) ;
#25959 = CARTESIAN_POINT ( 'NONE',  ( 0.05561375719525293859, -0.2541477197272140054, 0.3845235600768915352 ) ) ;
#25960 = DIRECTION ( 'NONE',  ( -0.000000000000000000, 0.5781348229923758408, -0.8159412518334724362 ) ) ;
#25961 = AXIS2_PLACEMENT_3D ( 'NONE', #13587, #34977, #10088 ) ;
#25962 = CARTESIAN_POINT ( 'NONE',  ( 0.2564068258101134812, -1.570482518261666183, -0.6784006763467468337 ) ) ;
#25963 = CARTESIAN_POINT ( 'NONE',  ( -0.1210148435730033917, -0.5061394519556894345, 0.1438724812234795092 ) ) ;
#25964 = CARTESIAN_POINT ( 'NONE',  ( 0.3665277588547195542, -1.753889016291175773, -0.6758757405868985879 ) ) ;
#25965 = DIRECTION ( 'NONE',  ( 1.000000000000000000, 2.341930812374887555E-31, -1.664003471950578127E-31 ) ) ;
#25966 = CARTESIAN_POINT ( 'NONE',  ( 0.7039831044528678250, -1.491019277299664214, 0.5110795091731726858 ) ) ;
#25967 = SHAPE_REPRESENTATION ( 'Top Pivot Bracket', ( #27819 ), #21247 ) ;
#25968 = DIRECTION ( 'NONE',  ( -0.8660512985181135770, -0.4999551463232369541, 0.000000000000000000 ) ) ;
#25969 = ORIENTED_EDGE ( 'NONE', *, *, #15292, .F. ) ;
#25970 = CARTESIAN_POINT ( 'NONE',  ( -0.2300000000000000100, 0.5182417262804744906, 0.3749999999999995559 ) ) ;
#25971 = VECTOR ( 'NONE', #5448, 39.37007874015748143 ) ;
#25972 = CARTESIAN_POINT ( 'NONE',  ( 0.5684515645774315118, -1.436290660855594314, 0.7423061315974909258 ) ) ;
#25974 = ORIENTED_EDGE ( 'NONE', *, *, #1723, .F. ) ;
#25973 = CARTESIAN_POINT ( 'NONE',  ( -0.08408070219615658425, -0.09959325338431362917, 0.3599999999999992095 ) ) ;
#25975 = AXIS2_PLACEMENT_3D ( 'NONE', #40174, #27453, #11614 ) ;
#25977 = EDGE_LOOP ( 'NONE', ( #6712, #8728, #1436, #23676, #37439 ) ) ;
#25976 = EDGE_LOOP ( 'NONE', ( #16814, #15071, #9563, #26280 ) ) ;
#25978 = CARTESIAN_POINT ( 'NONE',  ( 0.5383772456381804572, -1.668462259336880305, -0.5443662320918334352 ) ) ;
#25979 = AXIS2_PLACEMENT_3D ( 'NONE', #38769, #985, #395 ) ;
#25980 = ORIENTED_EDGE ( 'NONE', *, *, #26252, .T. ) ;
#25981 = DIRECTION ( 'NONE',  ( -0.4999551463232372317, 0.8660512985181135770, -0.000000000000000000 ) ) ;
#25982 = APPLIED_APPROVAL_ASSIGNMENT ( #22255, ( #6386 ) ) ;
#25983 = CARTESIAN_POINT ( 'NONE',  ( 0.6181169081387583031, -1.622430050042262817, -0.5225751115788848100 ) ) ;
#25984 = CALENDAR_DATE ( 2026, 13, 10 ) ;
#25985 = CARTESIAN_POINT ( 'NONE',  ( 0.0006767622704506771761, -0.6339827964191886434, -0.1178596299512805617 ) ) ;
#25986 = ORIENTED_EDGE ( 'NONE', *, *, #16955, .T. ) ;
#25987 = CARTESIAN_POINT ( 'NONE',  ( 0.2569009810042112707, -0.9727358380243329439, 0.6816368474424655544 ) ) ;
#25988 = VECTOR ( 'NONE', #36786, 39.37007874015748854 ) ;
#25989 = CARTESIAN_POINT ( 'NONE',  ( 0.08990936761266832278, -0.5436479961250927362, 0.1389823447417348756 ) ) ;
#25990 = CARTESIAN_POINT ( 'NONE',  ( 0.1687368033545940949, -0.7803388619690592165, 0.6016845811546662759 ) ) ;
#25991 = ORIENTED_EDGE ( 'NONE', *, *, #14966, .T. ) ;
#25992 = CARTESIAN_POINT ( 'NONE',  ( 0.06773272100053760736, -1.316698543382843978, 0.6004584978572466980 ) ) ;
#25993 = CARTESIAN_POINT ( 'NONE',  ( -2.070754768975509474, -0.09959325338431662678, 0.3750000000000004996 ) ) ;
#25994 = DIRECTION ( 'NONE',  ( 1.000000000000000000, 2.341930812374887555E-31, -1.664003471950578127E-31 ) ) ;
#25995 = EDGE_CURVE ( 'NONE', #27529, #2123, #12580, .T. ) ;
#25996 = CARTESIAN_POINT ( 'NONE',  ( 0.3416079711831710997, -1.748037889526394384, 0.5953977406395821736 ) ) ;
#25997 = CARTESIAN_POINT ( 'NONE',  ( 0.3974995447111917546, -1.636701680056106056, -0.6413756779823100995 ) ) ;
#25998 = CYLINDRICAL_SURFACE ( 'NONE', #15448, 0.03000000000000029379 ) ;
#25999 = CARTESIAN_POINT ( 'NONE',  ( 0.5369121333781083916, -1.380907096351134067, 0.7855338527398032511 ) ) ;
#26000 = CARTESIAN_POINT ( 'NONE',  ( -9.420476929099221768E-05, -0.7761415936933997450, -0.08716077457609966439 ) ) ;
#26001 = AXIS2_PLACEMENT_3D ( 'NONE', #2584, #24815, #146 ) ;
#26002 = CARTESIAN_POINT ( 'NONE',  ( 0.006119849279750269946, -0.8445422014862440374, 0.1249866068643721573 ) ) ;
#26003 = AXIS2_PLACEMENT_3D ( 'NONE', #30982, #37163, #40642 ) ;
#26004 = CARTESIAN_POINT ( 'NONE',  ( 0.02869712619511970847, -0.4519224903895654455, -0.2102851490355770736 ) ) ;
#26005 = CARTESIAN_POINT ( 'NONE',  ( 0.07670545266435074838, -1.210239791498856521, 0.7644951083879507614 ) ) ;
#26006 = CARTESIAN_POINT ( 'NONE',  ( 0.5067209442253272078, -1.108407892246341175, 0.6081930138323172752 ) ) ;
#26007 = CALENDAR_DATE ( 2026, 13, 10 ) ;
#26008 = DIRECTION ( 'NONE',  ( 0.8660512985181135770, 0.4999551463232368431, 0.000000000000000000 ) ) ;
#26009 = EDGE_CURVE ( 'NONE', #16210, #9524, #23788, .T. ) ;
#26010 = APPLIED_APPROVAL_ASSIGNMENT ( #4827, ( #3006 ) ) ;
#26011 = APPLIED_PERSON_AND_ORGANIZATION_ASSIGNMENT ( #25397, #22306, ( #35054 ) ) ;
#26012 = B_SPLINE_CURVE_WITH_KNOTS ( 'NONE', 3,
 ( #25932, #22854, #34559, #35373, #32263, #4082, #4683, #23244, #26523, #32472 ),
 .UNSPECIFIED., .F., .F.,
 ( 4, 2, 2, 2, 4 ),
 ( 0.000000000000000000, 0.0003584082070478624717, 0.0007168164140957249434, 0.001075224621143587361, 0.001433632828191449887 ),
 .UNSPECIFIED. ) ;
#26013 = CARTESIAN_POINT ( 'NONE',  ( 0.3844212907393982914, -1.715131551500115981, 0.4199026075312689010 ) ) ;
#26014 = AXIS2_PLACEMENT_3D ( 'NONE', #16671, #6788, #4509 ) ;
#26015 = DIRECTION ( 'NONE',  ( 0.000000000000000000, 0.7185945389471846134, -0.6954292836768403152 ) ) ;
#26016 = ORIENTED_EDGE ( 'NONE', *, *, #33563, .T. ) ;
#26017 = CARTESIAN_POINT ( 'NONE',  ( -0.02000000000000000042, -2.039407857756560638, -0.7963965713757412690 ) ) ;
#26018 = CARTESIAN_POINT ( 'NONE',  ( 0.002296835029420971411, -0.5198933010532057475, 0.1345257393686825342 ) ) ;
#26019 = CARTESIAN_POINT ( 'NONE',  ( 0.08937458818493072832, -0.5767519040287507615, 0.09166571991850554213 ) ) ;
#26020 = VERTEX_POINT ( 'NONE', #24393 ) ;
#26021 = FACE_OUTER_BOUND ( 'NONE', #18871, .T. ) ;
#26022 = CARTESIAN_POINT ( 'NONE',  ( 0.1998706582382908103, -0.5568697517490295290, 0.3524876158099713441 ) ) ;
#26024 = EDGE_LOOP ( 'NONE', ( #8543, #19079, #28039, #2836 ) ) ;
#26023 = VERTEX_POINT ( 'NONE', #8536 ) ;
#26025 = CARTESIAN_POINT ( 'NONE',  ( -0.02000000000000000042, -2.589364949149576933, -0.2950346662398796171 ) ) ;
#26026 = ORIENTED_EDGE ( 'NONE', *, *, #11893, .F. ) ;
#26027 = CARTESIAN_POINT ( 'NONE',  ( 0.3624061103390761596, -1.968824918581871808, -0.4968426515054794046 ) ) ;
#26028 = CARTESIAN_POINT ( 'NONE',  ( 0.5861528784094478528, -1.491558892450750129, 0.5551535569020163985 ) ) ;
#26029 = CARTESIAN_POINT ( 'NONE',  ( -0.05186792262757158878, 0.4530091620765398508, -0.1282979832840799583 ) ) ;
#26030 = ORIENTED_EDGE ( 'NONE', *, *, #1924, .T. ) ;
#26031 = CARTESIAN_POINT ( 'NONE',  ( 0.1406250000000003053, -0.4510478692700824466, 0.1457185332388695187 ) ) ;
#26032 = ADVANCED_FACE ( 'NONE', ( #21106 ), #33859, .F. ) ;
#26033 = CARTESIAN_POINT ( 'NONE',  ( 0.1225839179203127571, -0.7429807855966490404, 0.4493094660506182225 ) ) ;
#26034 = ADVANCED_FACE ( 'NONE', ( #34244 ), #11340, .F. ) ;
#26035 = CARTESIAN_POINT ( 'NONE',  ( 0.02807510720231470858, -0.5716849246173629773, 0.5309397757077717328 ) ) ;
#26036 = CARTESIAN_POINT ( 'NONE',  ( 0.3582932862619538916, -1.271006407676601224, 0.8606361610634840620 ) ) ;
#26038 = CARTESIAN_POINT ( 'NONE',  ( -0.1190701091186160687, -0.4967104654273769571, 0.3286746847624720802 ) ) ;
#26037 = CARTESIAN_POINT ( 'NONE',  ( 0.08855569358166180682, -1.004728779744561207, 0.8462681328029089123 ) ) ;
#26039 = CARTESIAN_POINT ( 'NONE',  ( 0.1057303466113572732, -1.090484623222926608, 0.6404094407937778177 ) ) ;
#26040 = APPROVAL_PERSON_ORGANIZATION ( #8798, #35281, #18268 ) ;
#26041 = VERTEX_POINT ( 'NONE', #2496 ) ;
#26042 = ADVANCED_FACE ( 'NONE', ( #30471 ), #26398, .T. ) ;
#26043 = EDGE_CURVE ( 'NONE', #38511, #5281, #8430, .T. ) ;
#26044 = DIRECTION ( 'NONE',  ( 0.8660512985181135770, 0.4999551463232371207, -3.316523347579165317E-14 ) ) ;
#26045 = CARTESIAN_POINT ( 'NONE',  ( 0.1164229267626636088, -0.4624049315941750615, 0.2417127322319602700 ) ) ;
#26046 = EDGE_CURVE ( 'NONE', #29847, #7589, #1454, .T. ) ;
#26047 = CONICAL_SURFACE ( 'NONE', #24721, 0.1600000000000004752, 1.047197551196598519 ) ;
#26048 = CARTESIAN_POINT ( 'NONE',  ( 0.1625982857068778153, -0.6782215948270849948, 0.2386756342038218459 ) ) ;
#26049 = CARTESIAN_POINT ( 'NONE',  ( -0.02000000000000000042, -1.622350287959229087, -0.08960079202753243321 ) ) ;
#26050 = CARTESIAN_POINT ( 'NONE',  ( 0.05999999999999990757, 0.000000000000000000, 0.000000000000000000 ) ) ;
#26051 = CARTESIAN_POINT ( 'NONE',  ( 0.6674886243000348607, -1.379560724353076306, 0.6935688206045713677 ) ) ;
#26052 = CARTESIAN_POINT ( 'NONE',  ( -2.070754768975504589, -0.09959325338431362917, 0.3599999999999976552 ) ) ;
#26053 = EDGE_CURVE ( 'NONE', #990, #21274, #18719, .T. ) ;
#26054 = CARTESIAN_POINT ( 'NONE',  ( 0.005974781735028359547, -0.8455926680078293955, 0.1457185332388710175 ) ) ;
#26055 = CARTESIAN_POINT ( 'NONE',  ( 0.05269111014006343241, 0.4484844745756971784, -0.1361491033660635341 ) ) ;
#26056 = CIRCLE ( 'NONE', #21453, 0.01500000000000003240 ) ;
#26057 = CARTESIAN_POINT ( 'NONE',  ( 0.4721942231302789228, -1.661553490448593351, -0.6136790096869797484 ) ) ;
#26058 = ORIENTED_EDGE ( 'NONE', *, *, #13374, .T. ) ;
#26059 = CARTESIAN_POINT ( 'NONE',  ( 0.3000183707936524002, -1.012959298482803305, 0.7233098648311757639 ) ) ;
#26060 = DIRECTION ( 'NONE',  ( -2.465190328815661892E-32, -1.000000000000000000, -6.656013887802287108E-31 ) ) ;
#26061 = CARTESIAN_POINT ( 'NONE',  ( -0.2399999999999999079, -2.183180860297908144, -0.4937760292030871079 ) ) ;
#26062 = CARTESIAN_POINT ( 'NONE',  ( 0.4498755731007036962, -1.064326126391425653, 0.5182417262812423209 ) ) ;
#26063 = VERTEX_POINT ( 'NONE', #15233 ) ;
#26064 = DIRECTION ( 'NONE',  ( 1.000000000000000000, 0.000000000000000000, 0.000000000000000000 ) ) ;
#26065 = CARTESIAN_POINT ( 'NONE',  ( -0.2399999999999999079, -3.384162466027138105, -0.4389494074304161608 ) ) ;
#26066 = DIRECTION ( 'NONE',  ( -1.000000000000000000, -0.000000000000000000, -0.000000000000000000 ) ) ;
#26067 = CARTESIAN_POINT ( 'NONE',  ( -0.01548846960721259221, -0.5203207976464859774, -0.08861466064783186936 ) ) ;
#26068 = CIRCLE ( 'NONE', #12254, 0.2000000000000000111 ) ;
#26069 = CARTESIAN_POINT ( 'NONE',  ( 0.1152323407702597613, -0.9559338739651589423, 0.6565232903784875562 ) ) ;
#26070 = VERTEX_POINT ( 'NONE', #36641 ) ;
#26071 = CARTESIAN_POINT ( 'NONE',  ( -0.1665334215456046041, 0.5173690063053929533, 0.3289428497172474652 ) ) ;
#26072 = CARTESIAN_POINT ( 'NONE',  ( 0.6496884796976931664, -1.552103590352501339, -0.4192475089069890859 ) ) ;
#26073 = CARTESIAN_POINT ( 'NONE',  ( 0.1864550573006002465, -0.7573172630633775437, 0.1903174488078394899 ) ) ;
#26074 = CARTESIAN_POINT ( 'NONE',  ( 0.1977770593140153743, -1.253111361966154469, -0.7170389795550398127 ) ) ;
#26075 = CARTESIAN_POINT ( 'NONE',  ( 0.3973402663755812858, -1.144813166135470350, 0.7100772268336156268 ) ) ;
#26077 = CARTESIAN_POINT ( 'NONE',  ( 0.3920841177027292179, -1.709814868753107175, 0.4185788730875646957 ) ) ;
#26076 = DIRECTION ( 'NONE',  ( 1.000000000000000000, 0.000000000000000000, 0.000000000000000000 ) ) ;
#26078 = CARTESIAN_POINT ( 'NONE',  ( -0.2300000000000000100, 0.5182417262804744906, 0.3749999999999995559 ) ) ;
#26079 = ORIENTED_EDGE ( 'NONE', *, *, #29825, .T. ) ;
#26080 = DATE_AND_TIME ( #1004, #32590 ) ;
#26081 = FACE_OUTER_BOUND ( 'NONE', #16767, .T. ) ;
#26082 = VERTEX_POINT ( 'NONE', #14840 ) ;
#26083 = ADVANCED_FACE ( 'NONE', ( #33341 ), #21014, .F. ) ;
#26084 = CARTESIAN_POINT ( 'NONE',  ( 0.4162055814956918121, -1.586242312561611634, 0.6469014666648855716 ) ) ;
#26086 = CARTESIAN_POINT ( 'NONE',  ( 0.1963398750588821740, -0.6872747950079822754, 0.3329267309873611413 ) ) ;
#26085 = CARTESIAN_POINT ( 'NONE',  ( 0.06493569881847564840, -0.8211346530322489734, 0.08200188512405065522 ) ) ;
#26087 = CARTESIAN_POINT ( 'NONE',  ( 0.1854014988492357074, -1.730386108846895921, -0.3576835534809157946 ) ) ;
#26088 = ORIENTED_EDGE ( 'NONE', *, *, #6175, .T. ) ;
#26089 = EDGE_CURVE ( 'NONE', #3822, #8849, #8948, .T. ) ;
#26090 = ORIENTED_EDGE ( 'NONE', *, *, #5739, .F. ) ;
#26091 = AXIS2_PLACEMENT_3D ( 'NONE', #30090, #20638, #32757 ) ;
#26092 = CARTESIAN_POINT ( 'NONE',  ( 0.3976745947184191499, -1.253140510797894125, 0.5816770576092088474 ) ) ;
#26093 = EDGE_CURVE ( 'NONE', #24586, #13712, #6021, .T. ) ;
#26094 = CARTESIAN_POINT ( 'NONE',  ( 0.1752860773241999015, -0.7509627177522383290, 0.5639964784769007089 ) ) ;
#26095 = ORIENTED_EDGE ( 'NONE', *, *, #18438, .F. ) ;
#26096 = DIRECTION ( 'NONE',  ( 2.686534417925922091E-31, -0.5877852522924700285, 0.8090169943749496717 ) ) ;
#26097 = CARTESIAN_POINT ( 'NONE',  ( 0.06540210900077661482, -2.107936428766288728, -0.2870436526301870517 ) ) ;
#26098 =( BOUNDED_SURFACE ( )  B_SPLINE_SURFACE ( 3, 2, ( 
 ( #11059, #11249, #11463 ),
 ( #23618, #36134, #23818 ),
 ( #27093, #39627, #24028 ),
 ( #33454, #5260, #29376 ) ),
 .UNSPECIFIED., .F., .F., .F. ) 
 B_SPLINE_SURFACE_WITH_KNOTS ( ( 4, 4 ),
 ( 3, 3 ),
 ( 1.279358563532895232E-17, 0.0008871692367534844822 ),
 ( 0.000000000000000000, 1.000000000000000000 ),
 .UNSPECIFIED. ) 
 GEOMETRIC_REPRESENTATION_ITEM ( )  RATIONAL_B_SPLINE_SURFACE ( (
 ( 1.000000000000000000, 0.9159177456829746822, 1.000000000000000000),
 ( 1.000000000000000000, 0.9105746466534058170, 1.000000000000000000),
 ( 1.000000000000000000, 0.9036974575934779708, 1.000000000000000000),
 ( 1.000000000000000000, 0.8959137433814483575, 1.000000000000000000) ) ) 
 REPRESENTATION_ITEM ( '' )  SURFACE ( )  );
#26099 = APPROVAL_PERSON_ORGANIZATION ( #17101, #28650, #32729 ) ;
#26100 = CARTESIAN_POINT ( 'NONE',  ( 0.4079901106498464158, -1.633071172328754983, -0.7462941026102626330 ) ) ;
#26101 = VERTEX_POINT ( 'NONE', #25325 ) ;
#26102 = CARTESIAN_POINT ( 'NONE',  ( 0.3329586478011472561, -1.131820071144838069, 0.5182417262812423209 ) ) ;
#26103 = CARTESIAN_POINT ( 'NONE',  ( 0.3222894045021684195, -1.758215778056678724, 0.5682417262808792113 ) ) ;
#26104 = CARTESIAN_POINT ( 'NONE',  ( -0.01548846960707517956, -0.4638115001431016848, -0.2459753896937850459 ) ) ;
#26105 = CIRCLE ( 'NONE', #40526, 0.01499999999999994914 ) ;
#26106 = CARTESIAN_POINT ( 'NONE',  ( 0.2842326993136328195, -1.549395603922531617, -0.7208999815284821144 ) ) ;
#26107 = CARTESIAN_POINT ( 'NONE',  ( 0.4016461280392738531, -1.742774929250199945, -0.4866300481184575033 ) ) ;
#26108 = EDGE_CURVE ( 'NONE', #12314, #13200, #19737, .T. ) ;
#26109 = CARTESIAN_POINT ( 'NONE',  ( -0.2746410161513779258, -2.809880844172510272, -0.2480969101616946337 ) ) ;
#26110 = EDGE_CURVE ( 'NONE', #1874, #23886, #28000, .T. ) ;
#26111 = CARTESIAN_POINT ( 'NONE',  ( 0.08197583149358347865, -1.314149287951269951, 0.5636821078433256194 ) ) ;
#26112 = PERSON_AND_ORGANIZATION ( #28500, #32463 ) ;
#26113 = ADVANCED_FACE ( 'NONE', ( #6379 ), #10940, .T. ) ;
#26114 = CARTESIAN_POINT ( 'NONE',  ( 0.6615513487989460595, -1.426771801028701825, -0.6132045830072060388 ) ) ;
#26115 = EDGE_CURVE ( 'NONE', #1749, #23808, #24915, .T. ) ;
#26116 = CARTESIAN_POINT ( 'NONE',  ( 0.05634402396114371325, 0.2613837787620694186, 0.3773006586902090675 ) ) ;
#26117 = CARTESIAN_POINT ( 'NONE',  ( 0.4162711365034791888, -1.591899382515264305, -0.6171341197600156425 ) ) ;
#26118 = DIRECTION ( 'NONE',  ( -7.771561172376107616E-16, 7.170354002788761615E-17, -1.000000000000000000 ) ) ;
#26119 = ORIENTED_EDGE ( 'NONE', *, *, #20039, .T. ) ;
#26120 = CARTESIAN_POINT ( 'NONE',  ( 0.2949815950263163233, -1.721662039081772733, 0.6893651101351793153 ) ) ;
#26121 = CARTESIAN_POINT ( 'NONE',  ( 0.6057880463341017707, -1.521544944963801882, -0.4306026127826089178 ) ) ;
#26122 = CARTESIAN_POINT ( 'NONE',  ( 0.5222653935518027923, -1.637842191745487730, -0.6100709635252473673 ) ) ;
#26123 = CARTESIAN_POINT ( 'NONE',  ( 0.2059267202968889376, -1.283046696160772271, -0.2869364497861741636 ) ) ;
#26124 = ORIENTED_EDGE ( 'NONE', *, *, #37167, .F. ) ;
#26125 = EDGE_LOOP ( 'NONE', ( #2168, #9443, #36067, #13945 ) ) ;
#26126 = CARTESIAN_POINT ( 'NONE',  ( 0.4972671625857253974, -1.080199071502573771, 0.5707417262808780478 ) ) ;
#26127 = VERTEX_POINT ( 'NONE', #37442 ) ;
#26128 = DIRECTION ( 'NONE',  ( 0.4999551463232373427, -0.8660512985181134660, 0.000000000000000000 ) ) ;
#26129 = CARTESIAN_POINT ( 'NONE',  ( 0.01548846960712814240, 0.3688619771571980954, 0.3775276577326248106 ) ) ;
#26130 = CARTESIAN_POINT ( 'NONE',  ( 0.3312706671835699557, -1.040500793050076256, 0.7771620973990449599 ) ) ;
#26132 = ORIENTED_EDGE ( 'NONE', *, *, #30625, .T. ) ;
#26131 = DIRECTION ( 'NONE',  ( 0.000000000000000000, -0.5877852522924820189, -0.8090169943749409009 ) ) ;
#26133 = CARTESIAN_POINT ( 'NONE',  ( 0.3578995607061009054, -0.9255625346965836719, 0.6844156867609741957 ) ) ;
#26134 = CARTESIAN_POINT ( 'NONE',  ( 0.3614155096298604097, -1.733227469354456263, -0.5467282445978081107 ) ) ;
#26135 = ORIENTED_EDGE ( 'NONE', *, *, #21482, .T. ) ;
#26136 = DIRECTION ( 'NONE',  ( 0.9823715787225890672, 0.000000000000000000, 0.1869387100578369376 ) ) ;
#26137 = ORIENTED_EDGE ( 'NONE', *, *, #34843, .T. ) ;
#26138 = CARTESIAN_POINT ( 'NONE',  ( 0.3279880978169363304, -1.639400604360913949, 0.5872381464462802514 ) ) ;
#26139 = CARTESIAN_POINT ( 'NONE',  ( 0.1124878519000608590, -0.7868389026292395005, -0.07401770572993009167 ) ) ;
#26140 = CARTESIAN_POINT ( 'NONE',  ( 0.05579155178881651383, -1.335540925555324332, 0.3667417262808778111 ) ) ;
#26141 = EDGE_CURVE ( 'NONE', #20593, #13608, #21831, .T. ) ;
#26142 = CARTESIAN_POINT ( 'NONE',  ( -2.051109323440559901E-05, -2.028068521879886177, -0.3128692020079770209 ) ) ;
#26143 = ORIENTED_EDGE ( 'NONE', *, *, #34676, .T. ) ;
#26144 = ADVANCED_FACE ( 'NONE', ( #34969 ), #266, .F. ) ;
#26145 = CARTESIAN_POINT ( 'NONE',  ( 0.5446975496317306709, -1.168323758156589953, 0.5471643355025310740 ) ) ;
#26146 = CARTESIAN_POINT ( 'NONE',  ( 0.1852697703518018379, -0.8388889655799375289, 0.1462684119608197997 ) ) ;
#26147 = CARTESIAN_POINT ( 'NONE',  ( -0.04575334816097668261, -0.4390433668671559486, 0.2110480141057394232 ) ) ;
#26148 = DIRECTION ( 'NONE',  ( 0.000000000000000000, -0.8585432690668223232, 0.5127411190260187102 ) ) ;
#26149 = CARTESIAN_POINT ( 'NONE',  ( 0.4113940825675456159, -1.194246046371860936, 0.6856661914167786476 ) ) ;
#26150 = CARTESIAN_POINT ( 'NONE',  ( 0.2640703320512924335, -0.5784607244460839848, 0.1477649966949237115 ) ) ;
#26151 = CARTESIAN_POINT ( 'NONE',  ( 0.1722267588728232657, -0.8902057077919266481, 0.1457020840065470779 ) ) ;
#26152 = CARTESIAN_POINT ( 'NONE',  ( 0.4136294883733859229, -1.694877849074643450, 0.4282417262808777547 ) ) ;
#26153 = CARTESIAN_POINT ( 'NONE',  ( 0.1999999999999789169, -2.097675824466503247, -0.7286991843995637153 ) ) ;
#26154 = CARTESIAN_POINT ( 'NONE',  ( -0.2746410161513782033, -2.183180860297908144, -0.4937760292030871079 ) ) ;
#26155 = CARTESIAN_POINT ( 'NONE',  ( 0.3206695962710918169, -1.761864437037726328, 0.5005377785206835961 ) ) ;
#26156 = EDGE_CURVE ( 'NONE', #892, #5233, #29026, .T. ) ;
#26157 = CARTESIAN_POINT ( 'NONE',  ( 0.03312451316780189864, -1.135919892802786935, 0.6708301406083743146 ) ) ;
#26158 = DIRECTION ( 'NONE',  ( -0.01265474379914244447, -0.8659329421511298142, 0.4999999971568662160 ) ) ;
#26159 = CARTESIAN_POINT ( 'NONE',  ( -0.01548846960707531660, -0.2306506793134033284, 0.4716198300880330985 ) ) ;
#26160 = DIRECTION ( 'NONE',  ( -1.000000000000000000, -2.341930812374887555E-31, 1.664003471950578127E-31 ) ) ;
#26161 = CARTESIAN_POINT ( 'NONE',  ( 0.4038347882556602153, -1.728811102479167472, -0.5994564538101174733 ) ) ;
#26162 = CARTESIAN_POINT ( 'NONE',  ( 0.2813060849845607780, -1.595222829165602763, 0.9543515313515406051 ) ) ;
#26163 = CARTESIAN_POINT ( 'NONE',  ( 0.6982426364517120287, -1.490497097242356128, 0.4889590780275660520 ) ) ;
#26164 = CARTESIAN_POINT ( 'NONE',  ( 0.4453503739158970465, -1.132163833841517864, 0.4458354100233239969 ) ) ;
#26165 = EDGE_LOOP ( 'NONE', ( #22188, #6368, #10370, #38453 ) ) ;
#26166 = CARTESIAN_POINT ( 'NONE',  ( -0.2399999999999999079, -3.253295730098268113, -0.6063490597057096254 ) ) ;
#26167 = CARTESIAN_POINT ( 'NONE',  ( 0.2241874626926840808, -0.8290071211643307292, 0.6423122159289148536 ) ) ;
#26169 = VERTEX_POINT ( 'NONE', #19357 ) ;
#26168 = CARTESIAN_POINT ( 'NONE',  ( -0.2399999999999999079, -2.845511416290244622, -0.3415338532332813926 ) ) ;
#26171 = ORIENTED_EDGE ( 'NONE', *, *, #23502, .T. ) ;
#26170 = EDGE_LOOP ( 'NONE', ( #25024, #33994, #5062, #21477 ) ) ;
#26172 = CARTESIAN_POINT ( 'NONE',  ( 0.5360939586754306374, -1.669780358010149568, -0.5511600881468147195 ) ) ;
#26173 = VERTEX_POINT ( 'NONE', #34761 ) ;
#26174 = CARTESIAN_POINT ( 'NONE',  ( 0.2059273467974225835, -1.283046334493782137, -0.6485234391946320676 ) ) ;
#26175 = DIRECTION ( 'NONE',  ( 0.000000000000000000, -0.7185945389473212819, 0.6954292836766992059 ) ) ;
#26176 = CARTESIAN_POINT ( 'NONE',  ( 0.6505092258670857053, -1.603730573490116162, -0.4546931408925022899 ) ) ;
#26177 = SECURITY_CLASSIFICATION_LEVEL ( 'unclassified' ) ;
#26178 = ADVANCED_FACE ( 'NONE', ( #59 ), #19146, .T. ) ;
#26179 = DIRECTION ( 'NONE',  ( -1.000000000000000000, -0.000000000000000000, -0.000000000000000000 ) ) ;
#26180 = ORIENTED_EDGE ( 'NONE', *, *, #21883, .T. ) ;
#26181 = CARTESIAN_POINT ( 'NONE',  ( 0.08817979687959355550, -0.8149952009864827041, 0.2376065706799516952 ) ) ;
#26182 = AXIS2_PLACEMENT_3D ( 'NONE', #33248, #11231, #27683 ) ;
#26183 = CARTESIAN_POINT ( 'NONE',  ( -0.08000000000000000167, -2.626773565144302935, -0.1926934094652516249 ) ) ;
#26184 = CARTESIAN_POINT ( 'NONE',  ( 0.1100467502016390098, -0.5492220161660857913, 0.1711048947129659437 ) ) ;
#26185 = CARTESIAN_POINT ( 'NONE',  ( 0.04927849822469471119, -1.184322729783269690, 0.6652490848847384397 ) ) ;
#26186 = CARTESIAN_POINT ( 'NONE',  ( 0.4812560861399013401, -1.590261200983826173, -0.4454942134426254086 ) ) ;
#26187 = CARTESIAN_POINT ( 'NONE',  ( -0.1631212487981059667, 0.5067506594879384041, 0.1120476149576258990 ) ) ;
#26188 = CARTESIAN_POINT ( 'NONE',  ( 0.3837628383327942871, -1.723043414611475921, 0.6192075928247073868 ) ) ;
#26189 = CARTESIAN_POINT ( 'NONE',  ( 0.6653107924583753219, -1.561504850366493669, 0.5590290280834550041 ) ) ;
#26190 = DIRECTION ( 'NONE',  ( -0.3468893892380656707, -0.3199132558031744233, 0.8816593788960987998 ) ) ;
#26191 = LINE ( 'NONE', #10536, #10035 ) ;
#26192 = CARTESIAN_POINT ( 'NONE',  ( 0.01548846960707350555, 0.4638115001430552775, 0.2459753896938760287 ) ) ;
#26193 = CARTESIAN_POINT ( 'NONE',  ( 0.01167820585366893989, -0.7468400741294990430, -0.1063804806529143748 ) ) ;
#26194 = CARTESIAN_POINT ( 'NONE',  ( 0.1801371744477150150, -0.8376302764228334974, 0.6639037816134167880 ) ) ;
#26195 =( NAMED_UNIT ( * ) PLANE_ANGLE_UNIT ( ) SI_UNIT ( $, .RADIAN. ) );
#26196 = CARTESIAN_POINT ( 'NONE',  ( 0.005980720888701209978, -0.8455916207747946611, 0.1457185332388707122 ) ) ;
#26197 = CARTESIAN_POINT ( 'NONE',  ( 0.4469283285619459201, -1.099869350908816878, -0.4033480720695140631 ) ) ;
#26198 = CARTESIAN_POINT ( 'NONE',  ( -0.002175845014896822093, -0.8193767622554530838, 0.2897257274743089139 ) ) ;
#26199 = CARTESIAN_POINT ( 'NONE',  ( 0.4598226378601848463, -1.064312249210862982, 0.6507415875188953258 ) ) ;
#26200 = APPLICATION_PROTOCOL_DEFINITION ( 'international standard', 'automotive_design', 2000, #5310 ) ;
#26201 = ADVANCED_FACE ( 'NONE', ( #12764 ), #3505, .T. ) ;
#26202 = CARTESIAN_POINT ( 'NONE',  ( 0.3856987765544705460, -1.723509814865189504, 0.4239487186058908952 ) ) ;
#26203 = CARTESIAN_POINT ( 'NONE',  ( 0.3048118929600290294, -1.756863971546229752, 0.5686390395660469999 ) ) ;
#26204 = ORIENTED_EDGE ( 'NONE', *, *, #2462, .T. ) ;
#26205 = CARTESIAN_POINT ( 'NONE',  ( 0.3784118722789395206, -1.581834032482531738, -0.7462941026102631881 ) ) ;
#26206 = CARTESIAN_POINT ( 'NONE',  ( 0.002558321733063344521, -0.5432559438152800846, 0.2281836175635736930 ) ) ;
#26207 = CARTESIAN_POINT ( 'NONE',  ( 0.2059273467974225835, -1.283046334493782137, -0.6485234391946320676 ) ) ;
#26208 = ORIENTED_EDGE ( 'NONE', *, *, #2658, .F. ) ;
#26209 = CARTESIAN_POINT ( 'NONE',  ( -0.3000000000000000999, -2.377058624452622393, -0.8919706583825134372 ) ) ;
#26210 = CARTESIAN_POINT ( 'NONE',  ( 0.6085831598237441131, -1.284018499374271371, 0.7837445821806681145 ) ) ;
#26212 = EDGE_LOOP ( 'NONE', ( #37096, #16497, #37153, #32932 ) ) ;
#26211 = VERTEX_POINT ( 'NONE', #22654 ) ;
#26213 = CARTESIAN_POINT ( 'NONE',  ( -0.02000000000000000042, -2.589364949149576933, -0.2950346662398796171 ) ) ;
#26214 = ORIENTED_EDGE ( 'NONE', *, *, #20488, .F. ) ;
#26215 = DIRECTION ( 'NONE',  ( 0.4999551463232372317, -0.8660512985181134660, 0.000000000000000000 ) ) ;
#26216 = PRODUCT_DEFINITION_SHAPE ( 'NONE', 'NONE',  #40653 ) ;
#26217 = CARTESIAN_POINT ( 'NONE',  ( 0.3864136346424311141, -1.704101823309675190, -0.5257935635300878818 ) ) ;
#26218 = CARTESIAN_POINT ( 'NONE',  ( -0.03303708955568261663, 0.5155567402493677065, -0.07470075307484629057 ) ) ;
#26219 = VERTEX_POINT ( 'NONE', #16454 ) ;
#26220 = CARTESIAN_POINT ( 'NONE',  ( 0.7047926081815637511, -1.538931328977949597, 0.5682417262808784342 ) ) ;
#26221 = CARTESIAN_POINT ( 'NONE',  ( 0.08841851961439690932, -0.6860782299043888255, 0.1966944432554147137 ) ) ;
#26222 = CARTESIAN_POINT ( 'NONE',  ( 0.03925517826010388456, -0.6829828959353061446, 0.6939464994351529636 ) ) ;
#26223 = CARTESIAN_POINT ( 'NONE',  ( 0.4701715835452702774, -1.558074627102426613, 0.5800830931470651874 ) ) ;
#26225 = DIRECTION ( 'NONE',  ( -1.000000000000000000, -2.341930812374887555E-31, 1.664003471950578127E-31 ) ) ;
#26224 = CARTESIAN_POINT ( 'NONE',  ( 0.2675635477756006519, -1.687710685839010960, 0.6071195368929496183 ) ) ;
#26226 = CARTESIAN_POINT ( 'NONE',  ( 0.3816210699381898386, -1.147921404532277423, 0.5760534757964502761 ) ) ;
#26227 = ORIENTED_EDGE ( 'NONE', *, *, #30619, .F. ) ;
#26228 = ORIENTED_EDGE ( 'NONE', *, *, #36357, .F. ) ;
#26229 = CARTESIAN_POINT ( 'NONE',  ( 0.2059273467974226113, -1.283046334493782803, -0.3194715457588298557 ) ) ;
#26230 = B_SPLINE_CURVE_WITH_KNOTS ( 'NONE', 3,
 ( #5614, #37292, #24563, #2545, #15082, #40167 ),
 .UNSPECIFIED., .F., .F.,
 ( 4, 2, 4 ),
 ( 0.008137213426454060344, 0.008732926872069602525, 0.009328640317685142971 ),
 .UNSPECIFIED. ) ;
#26231 = CARTESIAN_POINT ( 'NONE',  ( 0.1504062631728284027, -0.5880184383576758655, 0.5123281263564087862 ) ) ;
#26232 = CARTESIAN_POINT ( 'NONE',  ( -0.03647137243075494750, 0.2291011402250028028, -0.4576748478490495486 ) ) ;
#26233 = CARTESIAN_POINT ( 'NONE',  ( -0.03478556507500706746, -0.5086691011511474958, -0.08927554178899406445 ) ) ;
#26234 = DIRECTION ( 'NONE',  ( 1.000000000000000000, 0.000000000000000000, 0.000000000000000000 ) ) ;
#26235 = CARTESIAN_POINT ( 'NONE',  ( 0.1081859945995184841, -1.420406326327936952, 0.5048778302349400393 ) ) ;
#26236 = CARTESIAN_POINT ( 'NONE',  ( 0.3520862261316686226, -0.8866190960188533587, 0.7137788081797863393 ) ) ;
#26237 = DIRECTION ( 'NONE',  ( -0.9654310062341997511, 0.000000000000000000, -0.2606587274610626670 ) ) ;
#26238 = CARTESIAN_POINT ( 'NONE',  ( 0.01394802180609925127, -0.9131856928993046241, 0.5601969492252886207 ) ) ;
#26239 = CARTESIAN_POINT ( 'NONE',  ( 0.03875673594170580410, 0.4622647171927926069, -0.1151965740700868907 ) ) ;
#26240 = CARTESIAN_POINT ( 'NONE',  ( 0.5214666498663128591, -1.638124173219856150, -0.6107250905094568916 ) ) ;
#26241 = ORIENTED_EDGE ( 'NONE', *, *, #35143, .F. ) ;
#26242 = EDGE_CURVE ( 'NONE', #2801, #15916, #25074, .T. ) ;
#26243 = CARTESIAN_POINT ( 'NONE',  ( 0.3642735142549751171, -1.140585997052691702, 0.7302200931181149768 ) ) ;
#26244 = CARTESIAN_POINT ( 'NONE',  ( 0.2687203115727492264, -1.674044157977605529, 0.5754666865148680976 ) ) ;
#26245 = ADVANCED_FACE ( 'NONE', ( #7372 ), #29413, .F. ) ;
#26246 = CARTESIAN_POINT ( 'NONE',  ( -0.03474824846560561203, -0.2421026470131071862, -0.4562934628914087076 ) ) ;
#26247 = EDGE_CURVE ( 'NONE', #7589, #14915, #16659, .T. ) ;
#26248 = ORIENTED_EDGE ( 'NONE', *, *, #17968, .T. ) ;
#26249 = CYLINDRICAL_SURFACE ( 'NONE', #38429, 0.03000000000000029379 ) ;
#26250 = VERTEX_POINT ( 'NONE', #25719 ) ;
#26251 = CARTESIAN_POINT ( 'NONE',  ( 0.1052637591289525415, -0.6454443736156558753, 0.3793980098026691894 ) ) ;
#26252 = EDGE_CURVE ( 'NONE', #35830, #5331, #2749, .T. ) ;
#26253 = CARTESIAN_POINT ( 'NONE',  ( -0.1969433606228592482, 0.5138636982738209458, 0.3032895567580813356 ) ) ;
#26254 = CARTESIAN_POINT ( 'NONE',  ( 0.4062564059369914160, -1.133149177010132291, 0.4850828916047054684 ) ) ;
#26255 = DIMENSIONAL_EXPONENTS ( 1.000000000000000000, 0.000000000000000000, 0.000000000000000000, 0.000000000000000000, 0.000000000000000000, 0.000000000000000000, 0.000000000000000000 ) ;
#26256 = EDGE_CURVE ( 'NONE', #6802, #26020, #28361, .T. ) ;
#26257 = CARTESIAN_POINT ( 'NONE',  ( 0.1579648256015883934, -1.062633224222470973, 0.7378981056644309255 ) ) ;
#26258 = EDGE_LOOP ( 'NONE', ( #784, #23777, #11006, #39315, #25056, #24248, #27177, #13902 ) ) ;
#26259 = CARTESIAN_POINT ( 'NONE',  ( -0.1684323897528365310, 0.5231977509867857812, 0.3108929459560300645 ) ) ;
#26260 = CARTESIAN_POINT ( 'NONE',  ( 0.6583424475134876941, -1.513463612852635087, -0.4125214496082464932 ) ) ;
#26261 = CARTESIAN_POINT ( 'NONE',  ( 0.03474878377840097399, -0.5087732247600297297, -0.08925105102097614929 ) ) ;
#26262 = FACE_OUTER_BOUND ( 'NONE', #14012, .T. ) ;
#26263 = CARTESIAN_POINT ( 'NONE',  ( 0.3907296536724044755, -1.136716705566652497, 0.7120754492584040474 ) ) ;
#26265 = CARTESIAN_POINT ( 'NONE',  ( 0.5717376075374569488, -1.625791445033037963, 0.5487456121630054362 ) ) ;
#26264 = DIRECTION ( 'NONE',  ( -1.000000000000000000, -0.000000000000000000, -0.000000000000000000 ) ) ;
#26266 = CARTESIAN_POINT ( 'NONE',  ( 0.5832016030513088589, -1.507466846285616890, -0.4433012690765181230 ) ) ;
#26267 = VERTEX_POINT ( 'NONE', #19560 ) ;
#26268 = B_SPLINE_CURVE_WITH_KNOTS ( 'NONE', 3,
 ( #475, #31679, #6772, #38050, #18943, #31289, #10076, #32086, #23416, #35180, #31478, #3498, #19350, #3893, #37643, #18731, #15643, #31888, #9462, #34567, #3285, #15840 ),
 .UNSPECIFIED., .F., .F.,
 ( 4, 2, 2, 2, 2, 2, 2, 2, 2, 2, 4 ),
 ( 0.01043159516612753024, 0.01173405610995085883, 0.01303651705377418916, 0.01368774752568585086, 0.01433897799759751256, 0.01564143894142083421, 0.01694389988524415414, 0.01759513035715581236, 0.01824636082906747059, 0.01954882177289079051, 0.02085128271671411043 ),
 .UNSPECIFIED. ) ;
#26269 = CARTESIAN_POINT ( 'NONE',  ( -0.1532354427637373506, 0.4747053032734181999, 0.3600204025348319736 ) ) ;
#26270 = ORIENTED_EDGE ( 'NONE', *, *, #6439, .F. ) ;
#26271 = CARTESIAN_POINT ( 'NONE',  ( 0.04991041250764023662, -0.5686633296565585249, 0.2759322019946101046 ) ) ;
#26272 = ADVANCED_FACE ( 'NONE', ( #32090 ), #4307, .F. ) ;
#26274 = CARTESIAN_POINT ( 'NONE',  ( 0.1112283632243594861, -0.9174557404464535049, 0.07156239907761412222 ) ) ;
#26273 = CARTESIAN_POINT ( 'NONE',  ( 0.08825506839931913927, -0.6229187635552460023, 0.01667319878056269106 ) ) ;
#26275 = CARTESIAN_POINT ( 'NONE',  ( 0.1813268067401742623, -1.770784169840084354, -0.3550387660845038540 ) ) ;
#26276 = APPROVAL ( #39029, 'UNSPECIFIED' ) ;
#26277 = VERTEX_POINT ( 'NONE', #3897 ) ;
#26278 = CARTESIAN_POINT ( 'NONE',  ( 0.3834850620676270583, -1.099718979878179237, -0.5155029497116575543 ) ) ;
#26279 = CARTESIAN_POINT ( 'NONE',  ( 0.1865668073278461958, -0.7779540966166318405, 0.5928093434591832356 ) ) ;
#26280 = ORIENTED_EDGE ( 'NONE', *, *, #31542, .F. ) ;
#26281 = CARTESIAN_POINT ( 'NONE',  ( 0.1874548549128404462, -0.6895869275214173699, 0.05757391423245525330 ) ) ;
#26282 = CARTESIAN_POINT ( 'NONE',  ( 0.05201782277453876474, -0.4527080286589699742, 0.1280848763234518628 ) ) ;
#26283 = CARTESIAN_POINT ( 'NONE',  ( 0.6159314527243455739, -1.574808447129107059, 0.4182417262808776903 ) ) ;
#26284 = CARTESIAN_POINT ( 'NONE',  ( 0.1197622505559556849, -1.298029526664095101, 0.4264817069637966696 ) ) ;
#26285 = CARTESIAN_POINT ( 'NONE',  ( 0.4584446980593357424, -1.679963946744034375, 0.5963570223128070724 ) ) ;
#26286 = DIRECTION ( 'NONE',  ( -1.000000000000000000, -0.000000000000000000, -0.000000000000000000 ) ) ;
#26287 = CARTESIAN_POINT ( 'NONE',  ( 0.5827378505010344378, -1.244973309454295629, 0.8759922176168969399 ) ) ;
#26288 = DIRECTION ( 'NONE',  ( 0.000000000000000000, 0.000000000000000000, -1.000000000000000000 ) ) ;
#26289 = DIRECTION ( 'NONE',  ( 0.000000000000000000, -0.8159412518334724362, -0.5781348229923761739 ) ) ;
#26290 = APPLICATION_PROTOCOL_DEFINITION ( 'international standard', 'automotive_design', 2000, #6889 ) ;
#26291 = LINE ( 'NONE', #35347, #22559 ) ;
#26292 = CARTESIAN_POINT ( 'NONE',  ( 0.04575185649130587145, 0.2311416656438107786, 0.4288096517596615698 ) ) ;
#26293 = CARTESIAN_POINT ( 'NONE',  ( 0.1849752612960278986, -0.7177878707474302233, -0.02435127109689261965 ) ) ;
#26294 = CARTESIAN_POINT ( 'NONE',  ( 0.4753071910876713324, -1.208389221472485398, 0.5182417262812494263 ) ) ;
#26295 = CARTESIAN_POINT ( 'NONE',  ( 0.08808183485559285819, -1.318030620364535777, 0.4536778408853885947 ) ) ;
#26296 = EDGE_CURVE ( 'NONE', #17043, #8681, #15229, .T. ) ;
#26297 = CARTESIAN_POINT ( 'NONE',  ( 0.01618294926847982027, -0.6819691077562005654, 0.5071040197741758515 ) ) ;
#26298 = CARTESIAN_POINT ( 'NONE',  ( 0.5716435301310013317, -1.574655833597282228, -0.5703388428348806771 ) ) ;
#26299 = ADVANCED_FACE ( 'NONE', ( #25942, #38466 ), #36966, .T. ) ;
#26300 = FACE_OUTER_BOUND ( 'NONE', #39352, .T. ) ;
#26301 = CARTESIAN_POINT ( 'NONE',  ( 0.3048434042955683321, -1.756850910410517885, 0.5692538547013633599 ) ) ;
#26302 = CARTESIAN_POINT ( 'NONE',  ( -0.03874953289575294724, -0.3062954455724302139, 0.3649061716334319749 ) ) ;
#26303 = EDGE_CURVE ( 'NONE', #19986, #15269, #34448, .T. ) ;
#26304 = ORIENTED_EDGE ( 'NONE', *, *, #13288, .F. ) ;
#26305 = B_SPLINE_CURVE_WITH_KNOTS ( 'NONE', 3,
 ( #11809, #17775, #21292, #39581, #20894, #14700 ),
 .UNSPECIFIED., .F., .F.,
 ( 4, 2, 4 ),
 ( 0.000000000000000000, 0.0009816776391258473251, 0.001963355278251694650 ),
 .UNSPECIFIED. ) ;
#26306 = EDGE_LOOP ( 'NONE', ( #22224, #15791, #37145, #26957 ) ) ;
#26307 = CARTESIAN_POINT ( 'NONE',  ( 0.4264202721361136650, -1.467519734074643756, -0.5166151207188711680 ) ) ;
#26308 = VERTEX_POINT ( 'NONE', #14625 ) ;
#26309 = DIRECTION ( 'NONE',  ( 0.000000000000000000, 0.000000000000000000, -1.000000000000000000 ) ) ;
#26310 = CARTESIAN_POINT ( 'NONE',  ( 0.4213583293965230681, -1.178187296390520444, 0.7937282009877297817 ) ) ;
#26311 = VECTOR ( 'NONE', #9702, 39.37007874015748143 ) ;
#26313 = EDGE_LOOP ( 'NONE', ( #1553, #36982, #15533, #23634 ) ) ;
#26312 = CARTESIAN_POINT ( 'NONE',  ( -0.02953079040095652960, 0.5250338024619264354, 0.07436286310882474215 ) ) ;
#26314 = CARTESIAN_POINT ( 'NONE',  ( 0.5317104447742054818, -1.152447470094080328, 0.6575248185080280194 ) ) ;
#26315 = CARTESIAN_POINT ( 'NONE',  ( 0.04582889109739261835, 0.4790149006698649625, -0.08746027838083722528 ) ) ;
#26316 = VERTEX_POINT ( 'NONE', #11751 ) ;
#26317 = CARTESIAN_POINT ( 'NONE',  ( 0.4768848212686895849, -1.682051206446435243, -0.4156371400837835517 ) ) ;
#26318 = AXIS2_PLACEMENT_3D ( 'NONE', #5545, #28378, #18106 ) ;
#26319 = CARTESIAN_POINT ( 'NONE',  ( 0.02452063181877493087, -0.5608703732607570602, 0.2678004018634968508 ) ) ;
#26320 = EDGE_CURVE ( 'NONE', #15674, #8526, #20408, .T. ) ;
#26322 = CARTESIAN_POINT ( 'NONE',  ( 0.1118191872339531490, -0.8690880516572517811, -0.01359164210609734025 ) ) ;
#26321 = CARTESIAN_POINT ( 'NONE',  ( 0.5493166376341016566, -1.662147153828273050, -0.4937231952609894003 ) ) ;
#26323 = DIRECTION ( 'NONE',  ( -0.8745653259477854657, -0.4849077135392299565, 1.623341605721814605E-14 ) ) ;
#26324 = ADVANCED_FACE ( 'NONE', ( #1713 ), #30075, .F. ) ;
#26325 = CARTESIAN_POINT ( 'NONE',  ( 0.07404520294109505352, -1.411154561580794331, -0.3648634245470773196 ) ) ;
#26326 = ORIENTED_EDGE ( 'NONE', *, *, #25286, .F. ) ;
#26327 = DIRECTION ( 'NONE',  ( -0.4379975771764339498, -0.8989761522908011893, 0.000000000000000000 ) ) ;
#26328 = DIRECTION ( 'NONE',  ( -1.000000000000000000, -2.280301054154495132E-31, 1.664003471950577689E-31 ) ) ;
#26329 = CARTESIAN_POINT ( 'NONE',  ( 0.04420884470503230745, -1.503720994967077784, -0.6465903430088162374 ) ) ;
#26330 = CARTESIAN_POINT ( 'NONE',  ( 0.3639979711723335121, -1.990389627807109152, -0.5000272939307007780 ) ) ;
#26331 = CARTESIAN_POINT ( 'NONE',  ( 0.1026041305702670992, -0.8285543066798877199, 0.1457185332388695465 ) ) ;
#26332 = CARTESIAN_POINT ( 'NONE',  ( 0.4839231165671814550, -1.681532706550865397, -0.6135084623096023204 ) ) ;
#26333 = CARTESIAN_POINT ( 'NONE',  ( 0.4948540404288629957, -1.185897220935881569, 0.4182417262808778013 ) ) ;
#26334 = CARTESIAN_POINT ( 'NONE',  ( -0.1665334215456128475, 0.5173690063054338095, 0.3289428497172588450 ) ) ;
#26335 = CARTESIAN_POINT ( 'NONE',  ( -0.3000000000000000999, -2.323257895298838971, -0.7902071827178637209 ) ) ;
#26336 = CARTESIAN_POINT ( 'NONE',  ( 0.05561176441985726804, 0.4442366066780392697, 0.1229089882096652264 ) ) ;
#26337 = DIRECTION ( 'NONE',  ( 1.000000000000000000, -0.000000000000000000, -0.000000000000000000 ) ) ;
#26338 = DIRECTION ( 'NONE',  ( 0.4999551463232372317, -0.8660512985181135770, 0.000000000000000000 ) ) ;
#26339 = APPROVAL_DATE_TIME ( #17072, #3655 ) ;
#26340 = AXIS2_PLACEMENT_3D ( 'NONE', #33998, #30907, #30510 ) ;
#26341 = CARTESIAN_POINT ( 'NONE',  ( 0.03728397956324149692, -1.161596368933228263, 0.6766991317226744851 ) ) ;
#26342 = LINE ( 'NONE', #16887, #30391 ) ;
#26343 = DIRECTION ( 'NONE',  ( 0.9823715787225887341, 0.000000000000000000, 0.1869387100578391581 ) ) ;
#26344 = EDGE_CURVE ( 'NONE', #25042, #36473, #33756, .T. ) ;
#26345 = CIRCLE ( 'NONE', #30261, 0.01500000000000001853 ) ;
#26346 = AXIS2_PLACEMENT_3D ( 'NONE', #25031, #188, #15769 ) ;
#26347 = FACE_OUTER_BOUND ( 'NONE', #31763, .T. ) ;
#26348 = CARTESIAN_POINT ( 'NONE',  ( 0.4422952645324528809, -1.107215779629665775, 0.5826897552320002838 ) ) ;
#26349 = TOROIDAL_SURFACE ( 'NONE', #14490, 0.6154198107346402491, 0.7750185148639454624 ) ;
#26350 = EDGE_CURVE ( 'NONE', #8227, #30000, #25131, .T. ) ;
#26351 = CARTESIAN_POINT ( 'NONE',  ( -0.1157108546715127362, -0.4798936717283863174, 0.3382895567580815332 ) ) ;
#26352 = CARTESIAN_POINT ( 'NONE',  ( 0.02231181081520623027, -0.07006449514257565014, -0.5077922075898769760 ) ) ;
#26353 = ORIENTED_EDGE ( 'NONE', *, *, #36610, .F. ) ;
#26354 = CARTESIAN_POINT ( 'NONE',  ( 0.1883677752342057254, -0.5193258297658697176, 0.2202931123293304094 ) ) ;
#26355 = ORIENTED_EDGE ( 'NONE', *, *, #23355, .F. ) ;
#26356 = CARTESIAN_POINT ( 'NONE',  ( 0.2644464953634217963, -1.687293114999279364, 0.5653706809109292353 ) ) ;
#26357 = CARTESIAN_POINT ( 'NONE',  ( 0.6019347141590773997, -1.479867699914170887, 0.6295854643368259396 ) ) ;
#26358 = ORIENTED_EDGE ( 'NONE', *, *, #22153, .T. ) ;
#26360 = EDGE_LOOP ( 'NONE', ( #25700, #33957, #28377, #27302 ) ) ;
#26359 = EDGE_LOOP ( 'NONE', ( #2112, #18900, #240, #1385 ) ) ;
#26361 = CARTESIAN_POINT ( 'NONE',  ( 0.4506545850206880033, -1.130496563826020040, 0.8936068413349319561 ) ) ;
#26362 = ORIENTED_EDGE ( 'NONE', *, *, #24513, .F. ) ;
#26363 = CARTESIAN_POINT ( 'NONE',  ( 0.1020049694779444072, -1.076130111015646040, 0.8785625650948160059 ) ) ;
#26365 = DIRECTION ( 'NONE',  ( 0.8660512985181135770, 0.4999551463232370652, 2.644395542647567230E-15 ) ) ;
#26364 = CARTESIAN_POINT ( 'NONE',  ( 0.05078493045284276225, 0.4330747843660815999, 0.1920285438096122066 ) ) ;
#26366 = FACE_OUTER_BOUND ( 'NONE', #26359, .T. ) ;
#26367 = EDGE_CURVE ( 'NONE', #12802, #25709, #36033, .T. ) ;
#26368 = APPROVAL_ROLE ( '' ) ;
#26369 = TOROIDAL_SURFACE ( 'NONE', #8605, 0.1699999999999999845, 0.01499999999999999944 ) ;
#26370 = CARTESIAN_POINT ( 'NONE',  ( 0.001424326983700852176, -0.9534082139883233165, -0.01138449076159441485 ) ) ;
#26372 = ORIENTED_EDGE ( 'NONE', *, *, #11709, .F. ) ;
#26371 = ORIENTED_EDGE ( 'NONE', *, *, #16515, .F. ) ;
#26373 = ADVANCED_FACE ( 'NONE', ( #23702 ), #23798, .T. ) ;
#26374 = VECTOR ( 'NONE', #17887, 39.37007874015748143 ) ;
#26375 = CARTESIAN_POINT ( 'NONE',  ( 0.1880342618521675668, -0.9075390834704973875, 0.5937181048572924835 ) ) ;
#26376 = APPLICATION_CONTEXT ( 'configuration controlled 3d designs of mechanical parts and assemblies' ) ;
#26377 = CARTESIAN_POINT ( 'NONE',  ( 0.09001107770154211096, -0.5661368280801137853, 0.1669925442062198118 ) ) ;
#26378 = AXIS2_PLACEMENT_3D ( 'NONE', #9344, #31559, #2994 ) ;
#26379 = CARTESIAN_POINT ( 'NONE',  ( 0.1119770736976786057, -0.5747358184814086446, 0.2604905888496574229 ) ) ;
#26380 = CARTESIAN_POINT ( 'NONE',  ( 0.02864720926977884496, -1.052608752363344946, 0.5991139217441558973 ) ) ;
#26381 = DIRECTION ( 'NONE',  ( 5.551115123125663140E-17, 3.263080277421932464E-16, -1.000000000000000000 ) ) ;
#26382 = AXIS2_PLACEMENT_3D ( 'NONE', #4518, #17082, #4717 ) ;
#26383 = DIRECTION ( 'NONE',  ( 0.000000000000000000, 0.000000000000000000, 1.000000000000000000 ) ) ;
#26384 = AXIS2_PLACEMENT_3D ( 'NONE', #4545, #11141, #20617 ) ;
#26385 = CARTESIAN_POINT ( 'NONE',  ( 0.3386861991152600448, -1.749696087812495193, 0.5923449926325128345 ) ) ;
#26386 = DIRECTION ( 'NONE',  ( 0.000000000000000000, 0.000000000000000000, -1.000000000000000000 ) ) ;
#26387 = CARTESIAN_POINT ( 'NONE',  ( 0.06843998531048707534, -1.327705739214654290, 0.5337169134020078864 ) ) ;
#26388 = CARTESIAN_POINT ( 'NONE',  ( -0.08000000000000000167, -2.183180860297908144, -0.4937760292030871079 ) ) ;
#26389 = CARTESIAN_POINT ( 'NONE',  ( -0.07216878364870257800, 0.08000000000000023759, 0.1249999999999993477 ) ) ;
#26390 = CARTESIAN_POINT ( 'NONE',  ( -3.827020590142639815E-06, -0.7722669175349963222, -0.1011549324461909344 ) ) ;
#26391 = CARTESIAN_POINT ( 'NONE',  ( 0.5759042597488219783, -1.466327531223862168, 0.7055958116420547599 ) ) ;
#26392 = DIRECTION ( 'NONE',  ( -1.000000000000000000, -6.779273404243070203E-32, -4.314083075427408311E-32 ) ) ;
#26393 = CARTESIAN_POINT ( 'NONE',  ( 0.6106560647436484190, -1.615133038819531741, -0.5295971823914620291 ) ) ;
#26394 = CARTESIAN_POINT ( 'NONE',  ( 0.1512804210101734992, -1.367800832853933501, 0.8372142429942934783 ) ) ;
#26395 = CARTESIAN_POINT ( 'NONE',  ( 0.3550881284155063544, -0.9867921891001451007, 0.6236314015414725631 ) ) ;
#26396 = CALENDAR_DATE ( 2026, 13, 10 ) ;
#26397 = CARTESIAN_POINT ( 'NONE',  ( 0.4361655066743588827, -1.002659119010890665, 0.8380844301937150354 ) ) ;
#26398 = CONICAL_SURFACE ( 'NONE', #34252, 0.1020173459747799466, 1.047197551196601184 ) ;
#26399 = EDGE_CURVE ( 'NONE', #24957, #15024, #13264, .T. ) ;
#26400 = CARTESIAN_POINT ( 'NONE',  ( 0.6933448563160584666, -1.428940691336694435, 0.5798181663060312241 ) ) ;
#26401 = EDGE_CURVE ( 'NONE', #10402, #11533, #23121, .T. ) ;
#26402 = CARTESIAN_POINT ( 'NONE',  ( 0.3164963388020943236, -1.761765027830636265, 0.5685543529849016453 ) ) ;
#26403 = AXIS2_PLACEMENT_3D ( 'NONE', #31515, #19185, #3325 ) ;
#26404 = VECTOR ( 'NONE', #19233, 39.37007874015748143 ) ;
#26405 = ORIENTED_EDGE ( 'NONE', *, *, #39675, .F. ) ;
#26406 = DIRECTION ( 'NONE',  ( 0.5794373887239191445, -0.8150167559926640992, 5.613916328591080410E-15 ) ) ;
#26407 = CARTESIAN_POINT ( 'NONE',  ( 0.002311413808415803493, -0.5217619077427898544, 0.1735510156824913164 ) ) ;
#26408 = CARTESIAN_POINT ( 'NONE',  ( 0.09336344782360941896, -1.301801031155125576, 0.4543626096959849647 ) ) ;
#26409 = ORIENTED_EDGE ( 'NONE', *, *, #33901, .F. ) ;
#26410 = DIRECTION ( 'NONE',  ( -1.000000000000000000, -0.000000000000000000, -0.000000000000000000 ) ) ;
#26411 = CARTESIAN_POINT ( 'NONE',  ( 0.1946137278002632309, -0.5377497569806550803, 0.3020257395598471839 ) ) ;
#26413 = ORIENTED_EDGE ( 'NONE', *, *, #21287, .F. ) ;
#26412 = ORIENTED_EDGE ( 'NONE', *, *, #16737, .F. ) ;
#26414 = CARTESIAN_POINT ( 'NONE',  ( 0.07285041588532994994, -1.413036571972506428, -0.6863200093549134406 ) ) ;
#26415 = ORIENTED_EDGE ( 'NONE', *, *, #35073, .F. ) ;
#26416 = CARTESIAN_POINT ( 'NONE',  ( 0.05283094505689985010, -0.03968992937477396760, -0.4666439588235277713 ) ) ;
#26417 = CARTESIAN_POINT ( 'NONE',  ( 0.2411830489815006973, -1.239411181507260373, 0.4182417262808780234 ) ) ;
#26418 = CARTESIAN_POINT ( 'NONE',  ( -0.04047076529492513175, 0.4923674059679591375, -0.09402950075400676178 ) ) ;
#26419 = ORIENTED_EDGE ( 'NONE', *, *, #6693, .T. ) ;
#26420 = CARTESIAN_POINT ( 'NONE',  ( 0.2411561144159813930, -0.6701252966988756610, 0.6760123873793543181 ) ) ;
#26421 = CARTESIAN_POINT ( 'NONE',  ( 0.2709626867699331254, -0.9619090970917223427, 0.7179662831592660277 ) ) ;
#26422 = CARTESIAN_POINT ( 'NONE',  ( 0.2280934743446804969, -1.349410172253141083, 1.031711493552184722 ) ) ;
#26423 = CARTESIAN_POINT ( 'NONE',  ( 0.08764114647180407114, -0.5715037028378165962, 0.2642098798473031529 ) ) ;
#26425 = CARTESIAN_POINT ( 'NONE',  ( -0.1119307826792291932, -0.5115903042181114690, 0.1085569730127857874 ) ) ;
#26424 = CARTESIAN_POINT ( 'NONE',  ( 0.2703307786129086066, -1.660141123700932475, 0.7591185859682896275 ) ) ;
#26426 = CARTESIAN_POINT ( 'NONE',  ( 0.2764337282391635675, -1.207704344519198170, 0.5762930846214849856 ) ) ;
#26427 = EDGE_LOOP ( 'NONE', ( #31552, #26685, #37810 ) ) ;
#26428 = ORIENTED_EDGE ( 'NONE', *, *, #10189, .T. ) ;
#26429 = AXIS2_PLACEMENT_3D ( 'NONE', #8598, #15611, #33931 ) ;
#26430 = CARTESIAN_POINT ( 'NONE',  ( -0.08000000000000000167, -1.845925619402022155, -0.3444148183989317880 ) ) ;
#26431 = CARTESIAN_POINT ( 'NONE',  ( 0.1887787592512208679, -0.4599917114490411074, 0.1613286463795750858 ) ) ;
#26432 = DIRECTION ( 'NONE',  ( 0.000000000000000000, 0.000000000000000000, -1.000000000000000000 ) ) ;
#26433 = TOROIDAL_SURFACE ( 'NONE', #1484, 0.06434668806854092205, 0.005000000000000000104 ) ;
#26434 =( BOUNDED_SURFACE ( )  B_SPLINE_SURFACE ( 3, 2, ( 
 ( #8381, #11868, #20948 ),
 ( #9002, #24853, #5276 ),
 ( #17840, #30400, #30608 ),
 ( #9185, #31225, #33470 ),
 ( #34288, #14550, #30804 ),
 ( #21754, #27719, #24051 ),
 ( #12087, #37373, #2231 ),
 ( #36576, #5702, #33905 ),
 ( #6094, #18259, #24237 ),
 ( #14770, #27332, #39862 ),
 ( #18663, #36760, #21365 ),
 ( #8571, #39648, #40046 ),
 ( #21564, #27119, #8788 ),
 ( #2624, #5890, #15160 ),
 ( #21148, #12294, #33678 ),
 ( #18449, #11484, #31003 ) ),
 .UNSPECIFIED., .F., .F., .T. ) 
 B_SPLINE_SURFACE_WITH_KNOTS ( ( 4, 2, 2, 2, 2, 2, 2, 4 ),
 ( 3, 3 ),
 ( -1.680513367352531873E-17, 0.0003827823838732950985, 0.0007655647677466070021, 0.001148347151619918960, 0.001531129535493230701, 0.002296694303239854400, 0.002679476687113166358, 0.003062259070986478315 ),
 ( 0.000000000000000000, 1.000000000000000000 ),
 .UNSPECIFIED. ) 
 GEOMETRIC_REPRESENTATION_ITEM ( )  RATIONAL_B_SPLINE_SURFACE ( (
 ( 1.000000000000000000, 0.3554223140987289309, 1.000000000000000000),
 ( 1.000000000000000000, 0.3396177442905202182, 1.000000000000000000),
 ( 1.000000000000000000, 0.3300690577498115452, 1.000000000000000000),
 ( 1.000000000000000000, 0.3265765077624734891, 1.000000000000000000),
 ( 1.000000000000000000, 0.3329789664787625170, 1.000000000000000000),
 ( 1.000000000000000000, 0.3573122569017027073, 1.000000000000000000),
 ( 1.000000000000000000, 0.3749106637392585761, 1.000000000000000000),
 ( 1.000000000000000000, 0.4151524565129351974, 1.000000000000000000),
 ( 1.000000000000000000, 0.4373904795482970176, 1.000000000000000000),
 ( 1.000000000000000000, 0.5060226476725440126, 1.000000000000000000),
 ( 1.000000000000000000, 0.5527513560841460505, 1.000000000000000000),
 ( 1.000000000000000000, 0.6152787851278052056, 1.000000000000000000),
 ( 1.000000000000000000, 0.6350790670704571372, 1.000000000000000000),
 ( 1.000000000000000000, 0.6725960642926860356, 1.000000000000000000),
 ( 1.000000000000000000, 0.6901810608942313685, 1.000000000000000000),
 ( 1.000000000000000000, 0.7053379087130886571, 1.000000000000000000) ) ) 
 REPRESENTATION_ITEM ( '' )  SURFACE ( )  );
#26435 = AXIS2_PLACEMENT_3D ( 'NONE', #18294, #30833, #2654 ) ;
#26436 = DIRECTION ( 'NONE',  ( -1.000000000000000000, 0.000000000000000000, 0.000000000000000000 ) ) ;
#26437 = AXIS2_PLACEMENT_3D ( 'NONE', #22523, #38335, #31765 ) ;
#26438 = CARTESIAN_POINT ( 'NONE',  ( 0.05999999999999990757, -0.3165425539888620521, -0.4137570037148034507 ) ) ;
#26439 = DIRECTION ( 'NONE',  ( -2.465190328815661892E-32, -1.000000000000000000, -6.656013887802287108E-31 ) ) ;
#26440 = CARTESIAN_POINT ( 'NONE',  ( 0.5718426945711908571, -1.221126421150759755, 0.7198242229513793777 ) ) ;
#26441 = DIRECTION ( 'NONE',  ( -7.771561172376107616E-16, 7.170354002788761615E-17, -1.000000000000000000 ) ) ;
#26442 = CARTESIAN_POINT ( 'NONE',  ( 0.02571248063816646001, -0.9265510417023297141, 0.5911808037001393679 ) ) ;
#26443 = CARTESIAN_POINT ( 'NONE',  ( 2.359223927328458203E-18, -1.562563540555660935E-17, -0.04249999999999995448 ) ) ;
#26444 = CARTESIAN_POINT ( 'NONE',  ( 0.5576601260976730146, -1.622690634273228349, -0.5586186950843531340 ) ) ;
#26445 = CARTESIAN_POINT ( 'NONE',  ( 0.2817055660618989488, -0.9903619377415766589, 0.7098947161768234260 ) ) ;
#26446 = CARTESIAN_POINT ( 'NONE',  ( 0.04154009738085469305, 0.01731731106881273866, 0.4700109389422700290 ) ) ;
#26447 = CARTESIAN_POINT ( 'NONE',  ( -0.04945776359514877929, -0.2513414220725570525, -0.4057848608195684936 ) ) ;
#26448 = ORIENTED_EDGE ( 'NONE', *, *, #12996, .F. ) ;
#26449 = DIRECTION ( 'NONE',  ( 1.000000000000000000, -0.000000000000000000, -0.000000000000000000 ) ) ;
#26450 = CARTESIAN_POINT ( 'NONE',  ( 0.1371918123484773266, -0.7288778413244972887, 0.5065603813249234255 ) ) ;
#26451 = AXIS2_PLACEMENT_3D ( 'NONE', #29269, #35843, #10747 ) ;
#26452 = DIRECTION ( 'NONE',  ( 0.000000000000000000, 0.000000000000000000, -1.000000000000000000 ) ) ;
#26453 = CARTESIAN_POINT ( 'NONE',  ( -0.3000000000000000999, -3.253295730098268113, -0.6063490597057096254 ) ) ;
#26454 = CARTESIAN_POINT ( 'NONE',  ( 0.2005744727561914464, -1.165451418712258214, 0.7493240844877221418 ) ) ;
#26455 = ORIENTED_EDGE ( 'NONE', *, *, #8977, .T. ) ;
#26456 = CARTESIAN_POINT ( 'NONE',  ( -0.1710642717598483409, 0.4986889574318792984, 0.3078512670230422743 ) ) ;
#26457 = AXIS2_PLACEMENT_3D ( 'NONE', #26159, #878, #38677 ) ;
#26458 = AXIS2_PLACEMENT_3D ( 'NONE', #5076, #21352, #14143 ) ;
#26459 = CARTESIAN_POINT ( 'NONE',  ( 0.6420950953327444477, -1.575825456952314685, -0.4289601232232088113 ) ) ;
#26460 = CARTESIAN_POINT ( 'NONE',  ( 0.1861553373212349316, -1.375139781582257914, 0.4202249536440196276 ) ) ;
#26461 = FACE_OUTER_BOUND ( 'NONE', #15529, .T. ) ;
#26462 = AXIS2_PLACEMENT_3D ( 'NONE', #31284, #5330, #27577 ) ;
#26463 = CARTESIAN_POINT ( 'NONE',  ( 0.4170199900086061784, -1.169318256293440106, 0.7032566000091412528 ) ) ;
#26465 = CARTESIAN_POINT ( 'NONE',  ( 0.5669405059600367558, -1.627145089617755058, 0.5182417262812432091 ) ) ;
#26464 = FACE_OUTER_BOUND ( 'NONE', #5329, .T. ) ;
#26466 = DIRECTION ( 'NONE',  ( 0.000000000000000000, 0.000000000000000000, 1.000000000000000000 ) ) ;
#26467 = ORIENTED_EDGE ( 'NONE', *, *, #21057, .T. ) ;
#26468 = DIRECTION ( 'NONE',  ( 0.000000000000000000, -0.8159412518334721032, -0.5781348229923762849 ) ) ;
#26469 = ORIENTED_EDGE ( 'NONE', *, *, #29393, .F. ) ;
#26470 = CARTESIAN_POINT ( 'NONE',  ( 0.09463920074833474805, -0.7590106432348279197, 0.6020095118386700195 ) ) ;
#26471 = CIRCLE ( 'NONE', #37002, 0.1000000000000000194 ) ;
#26473 = CARTESIAN_POINT ( 'NONE',  ( 0.4806321272675940781, -1.111925921944065809, -0.6264081341737259834 ) ) ;
#26472 = CARTESIAN_POINT ( 'NONE',  ( 0.08929178762115032308, -0.5798774593664931531, 0.08564773658936970790 ) ) ;
#26474 = DIRECTION ( 'NONE',  ( -1.000000000000000000, -0.000000000000000000, -0.000000000000000000 ) ) ;
#26475 = VERTEX_POINT ( 'NONE', #30476 ) ;
#26476 = DIRECTION ( 'NONE',  ( 0.4999551463232373427, -0.8660512985181134660, 0.000000000000000000 ) ) ;
#26477 = ADVANCED_FACE ( 'NONE', ( #36648 ), #10611, .T. ) ;
#26478 = CARTESIAN_POINT ( 'NONE',  ( 0.1239748337567665587, -0.5947780400922306754, 0.3080055205751647263 ) ) ;
#26479 = ORIENTED_EDGE ( 'NONE', *, *, #9835, .T. ) ;
#26480 = CARTESIAN_POINT ( 'NONE',  ( 0.3969982963057278047, -1.750077671058422046, -0.4821875037442182599 ) ) ;
#26481 = CARTESIAN_POINT ( 'NONE',  ( 0.04047170147977395549, -0.4536011460193543621, 0.2133323880731011479 ) ) ;
#26482 = CARTESIAN_POINT ( 'NONE',  ( 0.6238534087474900680, -1.575592206279644136, 0.4182417262808776903 ) ) ;
#26483 = CARTESIAN_POINT ( 'NONE',  ( 0.1372954668741161455, -1.287838507416935396, 0.4318400540907381679 ) ) ;
#26484 = AXIS2_PLACEMENT_3D ( 'NONE', #5111, #24268, #17666 ) ;
#26485 = CARTESIAN_POINT ( 'NONE',  ( 0.3926032618788913298, -1.756026311479878421, -0.5284552501752952658 ) ) ;
#26486 = CARTESIAN_POINT ( 'NONE',  ( -0.02000000000000000042, -2.321277022828569958, -0.5785054236952983375 ) ) ;
#26487 = EDGE_CURVE ( 'NONE', #14366, #30357, #15877, .T. ) ;
#26488 = CARTESIAN_POINT ( 'NONE',  ( 0.2888622377148890585, -0.7373900025806978675, 0.6684008680139050806 ) ) ;
#26489 = VECTOR ( 'NONE', #18493, 39.37007874015748854 ) ;
#26490 = TOROIDAL_SURFACE ( 'NONE', #20566, 0.5250000000000000222, 0.01499999999999999944 ) ;
#26491 = FACE_OUTER_BOUND ( 'NONE', #6410, .T. ) ;
#26492 = CARTESIAN_POINT ( 'NONE',  ( 0.02235124290213119647, -0.2417860359143750582, -0.4518977707513310293 ) ) ;
#26493 = PERSON_AND_ORGANIZATION ( #28500, #32463 ) ;
#26494 = AXIS2_PLACEMENT_3D ( 'NONE', #1276, #23279, #1469 ) ;
#26495 = CARTESIAN_POINT ( 'NONE',  ( 0.6482135835996580830, -1.415164486681432798, -0.6155586712855226628 ) ) ;
#26496 = CARTESIAN_POINT ( 'NONE',  ( -0.02000000000000000042, -1.599201040860868339, 0.1842182323853684411 ) ) ;
#26497 = CARTESIAN_POINT ( 'NONE',  ( -0.1212602504878793896, -0.5073146173917532087, 0.3032895567580782270 ) ) ;
#26498 = CARTESIAN_POINT ( 'NONE',  ( 0.4513496650050710657, -1.222212685274413291, 0.4817276195033231567 ) ) ;
#26499 = CIRCLE ( 'NONE', #25174, 0.06434668806854085266 ) ;
#26500 = CARTESIAN_POINT ( 'NONE',  ( 0.07958551560962676130, -1.322831287755754648, 0.4682677590956375036 ) ) ;
#26501 = AXIS2_PLACEMENT_3D ( 'NONE', #11196, #36281, #1956 ) ;
#26502 = EDGE_CURVE ( 'NONE', #24229, #3740, #11856, .T. ) ;
#26503 = APPLIED_DATE_AND_TIME_ASSIGNMENT ( #19378, #12995, ( #25357 ) ) ;
#26504 = CARTESIAN_POINT ( 'NONE',  ( 0.2721752123224986386, -1.596339224327277595, 0.9197038883954219424 ) ) ;
#26505 = CARTESIAN_POINT ( 'NONE',  ( 0.5749393492916552439, -1.540325544240326083, -0.4818059086064602203 ) ) ;
#26506 = CARTESIAN_POINT ( 'NONE',  ( 0.02999778723028644414, -2.087755359801441557, -0.2623954751430960797 ) ) ;
#26507 = CARTESIAN_POINT ( 'NONE',  ( 0.5893686083517821750, -1.590946717650547182, 0.4182417262808776903 ) ) ;
#26508 = CARTESIAN_POINT ( 'NONE',  ( -0.04285534776242247434, -0.3459954891507863728, 0.3537381284079030297 ) ) ;
#26509 = VERTEX_POINT ( 'NONE', #31300 ) ;
#26510 = ORIENTED_EDGE ( 'NONE', *, *, #11494, .T. ) ;
#26511 = PLANE ( 'NONE',  #18468 ) ;
#26512 = CARTESIAN_POINT ( 'NONE',  ( 0.3718671178488404672, -1.764871997527151848, -0.5765770349210319612 ) ) ;
#26513 = VERTEX_POINT ( 'NONE', #18529 ) ;
#26514 = LINE ( 'NONE', #20543, #25015 ) ;
#26515 = CARTESIAN_POINT ( 'NONE',  ( 0.3492852788876838477, -1.696550652582485830, -0.4668076899784869283 ) ) ;
#26516 = AXIS2_PLACEMENT_3D ( 'NONE', #39159, #26410, #29295 ) ;
#26517 = CARTESIAN_POINT ( 'NONE',  ( 0.5433381647791950542, -1.365663563338381570, 0.6765757352007879533 ) ) ;
#26519 = ORIENTED_EDGE ( 'NONE', *, *, #31877, .T. ) ;
#26518 = CARTESIAN_POINT ( 'NONE',  ( -0.1969433606228599420, 0.5138636982738206127, 0.1528658435937004789 ) ) ;
#26520 = CARTESIAN_POINT ( 'NONE',  ( 0.4452807512755668218, -1.047893410216382382, 0.6910429845488149647 ) ) ;
#26521 = FACE_OUTER_BOUND ( 'NONE', #7407, .T. ) ;
#26522 = ORIENTED_EDGE ( 'NONE', *, *, #18042, .F. ) ;
#26523 = CARTESIAN_POINT ( 'NONE',  ( 0.5881066016147241671, -1.489496199501605611, -0.5990371943001994159 ) ) ;
#26524 = AXIS2_PLACEMENT_3D ( 'NONE', #22172, #15757, #31598 ) ;
#26525 = CARTESIAN_POINT ( 'NONE',  ( 0.2564594514974720130, -1.414529048416510504, 0.9122281602349449070 ) ) ;
#26527 = DIRECTION ( 'NONE',  ( 0.8660512985181126888, 0.4999551463232385085, 0.000000000000000000 ) ) ;
#26526 = CARTESIAN_POINT ( 'NONE',  ( 0.6602609276941329153, -1.536889406902937072, 0.4273433096175258128 ) ) ;
#26528 = CARTESIAN_POINT ( 'NONE',  ( 0.05573493074139709846, -1.335442843293342063, 0.4177417262808780229 ) ) ;
#26529 = FACE_OUTER_BOUND ( 'NONE', #27879, .T. ) ;
#26530 = ORIENTED_EDGE ( 'NONE', *, *, #25559, .F. ) ;
#26531 = DIMENSIONAL_EXPONENTS ( 1.000000000000000000, 0.000000000000000000, 0.000000000000000000, 0.000000000000000000, 0.000000000000000000, 0.000000000000000000, 0.000000000000000000 ) ;
#26532 = EDGE_CURVE ( 'NONE', #20383, #34142, #11939, .T. ) ;
#26533 = DIRECTION ( 'NONE',  ( -1.000000000000000000, 0.000000000000000000, 0.000000000000000000 ) ) ;
#26534 = TOROIDAL_SURFACE ( 'NONE', #25897, 0.09088067974298029428, 0.01499999999999999944 ) ;
#26535 = CARTESIAN_POINT ( 'NONE',  ( 0.003464874609604914023, -1.839213656041257527, -0.6448626447465779510 ) ) ;
#26536 = EDGE_CURVE ( 'NONE', #22389, #11737, #6178, .T. ) ;
#26537 = CYLINDRICAL_SURFACE ( 'NONE', #7553, 0.5543128707267515054 ) ;
#26538 = AXIS2_PLACEMENT_3D ( 'NONE', #29007, #870, #31907 ) ;
#26539 = CARTESIAN_POINT ( 'NONE',  ( 0.3644424172741055346, -1.232111622910960325, 0.6721086862942787787 ) ) ;
#26540 = DIRECTION ( 'NONE',  ( 0.000000000000000000, -0.8438867430782092116, -0.5365213554527465956 ) ) ;
#26541 = EDGE_CURVE ( 'NONE', #32882, #36405, #40176, .T. ) ;
#26542 = CYLINDRICAL_SURFACE ( 'NONE', #12783, 2.001674066779353556 ) ;
#26543 = EDGE_CURVE ( 'NONE', #11891, #12319, #29056, .T. ) ;
#26544 = DIRECTION ( 'NONE',  ( 0.8660512985181134660, 0.4999551463232371207, 0.000000000000000000 ) ) ;
#26545 = DIRECTION ( 'NONE',  ( -1.000000000000000000, 8.195543980992782950E-15, 4.097771990496391475E-15 ) ) ;
#26546 = DIRECTION ( 'NONE',  ( 0.000000000000000000, 0.000000000000000000, -1.000000000000000000 ) ) ;
#26547 = DIRECTION ( 'NONE',  ( 0.000000000000000000, 0.000000000000000000, -1.000000000000000000 ) ) ;
#26548 = DIRECTION ( 'NONE',  ( -0.4999551463232372317, 0.8660512985181135770, -0.000000000000000000 ) ) ;
#26549 =( NAMED_UNIT ( * ) PLANE_ANGLE_UNIT ( ) SI_UNIT ( $, .RADIAN. ) );
#26550 = CIRCLE ( 'NONE', #8792, 0.2200000000000000011 ) ;
#26551 = CARTESIAN_POINT ( 'NONE',  ( 0.3831835866196274254, -1.151467227178074593, 0.4237037165649273907 ) ) ;
#26552 = DIRECTION ( 'NONE',  ( 0.000000000000000000, 0.000000000000000000, -1.000000000000000000 ) ) ;
#26553 = CARTESIAN_POINT ( 'NONE',  ( 0.7071069014570956490, -1.521634513519168452, 0.5617257377400114438 ) ) ;
#26554 = AXIS2_PLACEMENT_3D ( 'NONE', #38990, #10823, #26671 ) ;
#26555 = CIRCLE ( 'NONE', #39661, 0.08249999999977548903 ) ;
#26556 = EDGE_CURVE ( 'NONE', #29236, #22989, #15289, .T. ) ;
#26557 = PRODUCT_DEFINITION_SHAPE ( 'NONE', 'NONE',  #40659 ) ;
#26558 = CARTESIAN_POINT ( 'NONE',  ( -0.2399999999999999079, -3.739689364820627748, -0.3461216533844236887 ) ) ;
#26559 = CARTESIAN_POINT ( 'NONE',  ( 0.5985082606850495868, -1.473464502187743941, 0.6023744451300401259 ) ) ;
#26560 = CARTESIAN_POINT ( 'NONE',  ( 0.3098710801442948748, -1.725017193307739838, 0.7846558205662965690 ) ) ;
#26561 = DIRECTION ( 'NONE',  ( -0.4999551463232372317, 0.8660512985181135770, -0.000000000000000000 ) ) ;
#26562 = AXIS2_PLACEMENT_3D ( 'NONE', #30578, #7986, #21331 ) ;
#26563 = VERTEX_POINT ( 'NONE', #22055 ) ;
#26564 = ORIENTED_EDGE ( 'NONE', *, *, #3352, .T. ) ;
#26565 = CIRCLE ( 'NONE', #37062, 0.1000000000000000194 ) ;
#26566 = CARTESIAN_POINT ( 'NONE',  ( 0.1731170367617594075, -0.5199985899392068900, 0.1286442151290814462 ) ) ;
#26567 = ORIENTED_EDGE ( 'NONE', *, *, #19758, .F. ) ;
#26568 = CARTESIAN_POINT ( 'NONE',  ( -0.0004431470427073231017, -0.9367128829938298207, 0.1457185332388704069 ) ) ;
#26569 = CARTESIAN_POINT ( 'NONE',  ( 0.6017145574000101194, -1.483072097257081445, 0.5679475895592410728 ) ) ;
#26571 = ORIENTED_EDGE ( 'NONE', *, *, #33878, .F. ) ;
#26570 = CARTESIAN_POINT ( 'NONE',  ( -0.0002086810045813790077, -0.7085389528372163515, -0.01266920697570707473 ) ) ;
#26572 = ORIENTED_EDGE ( 'NONE', *, *, #450, .F. ) ;
#26573 = DIRECTION ( 'NONE',  ( 0.000000000000000000, 0.000000000000000000, 1.000000000000000000 ) ) ;
#26574 = ORIENTED_EDGE ( 'NONE', *, *, #15702, .T. ) ;
#26575 = CARTESIAN_POINT ( 'NONE',  ( -0.01345624470603132110, -0.5489092317405479537, 0.2541791200293259112 ) ) ;
#26577 = DIRECTION ( 'NONE',  ( 0.000000000000000000, 0.000000000000000000, -1.000000000000000000 ) ) ;
#26576 = FACE_OUTER_BOUND ( 'NONE', #32686, .T. ) ;
#26578 = CARTESIAN_POINT ( 'NONE',  ( 0.6186566136881834765, -1.609114265322737269, -0.4705007761744832706 ) ) ;
#26579 = APPROVAL_DATE_TIME ( #26787, #40187 ) ;
#26580 = AXIS2_PLACEMENT_3D ( 'NONE', #31124, #6002, #34403 ) ;
#26581 = CARTESIAN_POINT ( 'NONE',  ( -0.2746410161513770931, -2.853330612949663170, -0.6088139570729240724 ) ) ;
#26583 = ORIENTED_EDGE ( 'NONE', *, *, #4622, .F. ) ;
#26582 = ORIENTED_EDGE ( 'NONE', *, *, #31392, .T. ) ;
#26584 = CIRCLE ( 'NONE', #24621, 0.07999999999999996003 ) ;
#26585 = CARTESIAN_POINT ( 'NONE',  ( 0.09998776873723287661, -0.8261931218866173099, 0.3381795186695624733 ) ) ;
#26586 = CARTESIAN_POINT ( 'NONE',  ( 0.04211891365776822965, -0.9906088561216523924, 0.6817232344076664674 ) ) ;
#26587 = CIRCLE ( 'NONE', #14766, 0.01500000000000002547 ) ;
#26588 = ADVANCED_FACE ( 'NONE', ( #18748 ), #33972, .F. ) ;
#26589 = CARTESIAN_POINT ( 'NONE',  ( 0.1472076274870235679, -0.7270890653341587351, 0.5403574314070681561 ) ) ;
#26590 = CIRCLE ( 'NONE', #24626, 0.1400000000000007627 ) ;
#26591 = CARTESIAN_POINT ( 'NONE',  ( 0.1246370012518288467, -0.6330505824401759796, 0.3923014813962043545 ) ) ;
#26592 = CARTESIAN_POINT ( 'NONE',  ( 0.1790539915098864343, -0.5050269068883876944, 0.2306937646411194032 ) ) ;
#26593 = CARTESIAN_POINT ( 'NONE',  ( 0.6069176374591634948, -1.480164522464830990, 0.5706138896049881559 ) ) ;
#26594 = CARTESIAN_POINT ( 'NONE',  ( 0.6393295224005999255, -1.564323831884513849, 0.4219358453006255560 ) ) ;
#26595 = EDGE_CURVE ( 'NONE', #9524, #16210, #38886, .T. ) ;
#26596 = CARTESIAN_POINT ( 'NONE',  ( 2.685932296560563025E-16, -0.01499999999999986587, 0.1699999999999999845 ) ) ;
#26597 = CARTESIAN_POINT ( 'NONE',  ( 0.3123258297132953665, -1.533408232077866362, -0.7003322928082994503 ) ) ;
#26598 = EDGE_CURVE ( 'NONE', #13401, #13556, #6894, .T. ) ;
#26599 = AXIS2_PLACEMENT_3D ( 'NONE', #40172, #17371, #8502 ) ;
#26600 = CARTESIAN_POINT ( 'NONE',  ( 0.3740960844805631957, -1.108072201694596526, 0.5182417262812423209 ) ) ;
#26601 = CARTESIAN_POINT ( 'NONE',  ( 0.07497864282572899719, -1.322056043867073427, 0.4862695133534066794 ) ) ;
#26602 = CARTESIAN_POINT ( 'NONE',  ( 0.4000000000004778067, -2.061712828828752730, -0.2709148305154810421 ) ) ;
#26603 = AXIS2_PLACEMENT_3D ( 'NONE', #16237, #10047, #6538 ) ;
#26604 = CARTESIAN_POINT ( 'NONE',  ( -8.502430919704473552E-05, -0.7684146918674319426, -0.08995813089792253914 ) ) ;
#26605 = FACE_OUTER_BOUND ( 'NONE', #24202, .T. ) ;
#26606 = EDGE_CURVE ( 'NONE', #10778, #23598, #40271, .T. ) ;
#26607 = CARTESIAN_POINT ( 'NONE',  ( 0.007263304146752605668, -0.7838023699412952627, 0.02006003217016949156 ) ) ;
#26608 = CARTESIAN_POINT ( 'NONE',  ( 0.6100534684184480971, -1.615500477088944065, -0.5228428417932495798 ) ) ;
#26609 = CARTESIAN_POINT ( 'NONE',  ( 0.01933088760290150449, -0.9443470376599968352, 0.6102586483404766060 ) ) ;
#26610 = CARTESIAN_POINT ( 'NONE',  ( 0.4929039159923706559, -1.082692164550193237, 0.5711674032880966756 ) ) ;
#26611 = DATE_AND_TIME ( #4166, #1042 ) ;
#26612 = CARTESIAN_POINT ( 'NONE',  ( 0.6473156011871936677, -1.349322671506162141, 0.8501878200258047302 ) ) ;
#26613 = ADVANCED_FACE ( 'NONE', ( #35785 ), #485, .F. ) ;
#26614 = ADVANCED_FACE ( 'NONE', ( #32095 ), #6783, .T. ) ;
#26615 = AXIS2_PLACEMENT_3D ( 'NONE', #30765, #18625, #9350 ) ;
#26616 = ADVANCED_FACE ( 'NONE', ( #38856 ), #19201, .T. ) ;
#26617 = AXIS2_PLACEMENT_3D ( 'NONE', #29930, #36276, #21677 ) ;
#26618 = DIRECTION ( 'NONE',  ( 0.000000000000000000, 0.000000000000000000, 1.000000000000000000 ) ) ;
#26619 = CARTESIAN_POINT ( 'NONE',  ( 0.3084290614922874374, -1.760927762095492843, 0.5681371985488602450 ) ) ;
#26620 = AXIS2_PLACEMENT_3D ( 'NONE', #24796, #37316, #31365 ) ;
#26621 = AXIS2_PLACEMENT_3D ( 'NONE', #3890, #35377, #13361 ) ;
#26622 = EDGE_CURVE ( 'NONE', #13057, #20865, #23823, .T. ) ;
#26623 = ORIENTED_EDGE ( 'NONE', *, *, #22893, .T. ) ;
#26624 = CARTESIAN_POINT ( 'NONE',  ( 0.03113248654051816583, 0.5209315849442416324, 0.3202538583802939098 ) ) ;
#26625 = PRODUCT_DEFINITION_FORMATION_WITH_SPECIFIED_SOURCE ( 'ANY', '', #3852, .NOT_KNOWN. ) ;
#26626 = CARTESIAN_POINT ( 'NONE',  ( 0.09787890177536405500, -1.020308744753638974, 0.8413265823706557178 ) ) ;
#26627 = CARTESIAN_POINT ( 'NONE',  ( 0.1496044234471295975, -1.269186625694784132, 0.4303707757303895098 ) ) ;
#26629 = VERTEX_POINT ( 'NONE', #28810 ) ;
#26628 = DIRECTION ( 'NONE',  ( -1.000000000000000000, 0.000000000000000000, 0.000000000000000000 ) ) ;
#26630 = DIRECTION ( 'NONE',  ( 1.000000000000000000, 2.341930812374887555E-31, -1.664003471950578127E-31 ) ) ;
#26631 = CIRCLE ( 'NONE', #1020, 0.08830708661417320526 ) ;
#26632 = CARTESIAN_POINT ( 'NONE',  ( 0.6761021464639213052, -1.407442781842621171, 0.4761751337611269674 ) ) ;
#26634 = ORIENTED_EDGE ( 'NONE', *, *, #4995, .F. ) ;
#26633 = ORIENTED_EDGE ( 'NONE', *, *, #26909, .F. ) ;
#26635 = CARTESIAN_POINT ( 'NONE',  ( 0.06788540646851175253, -1.426487579412121898, -0.6578865797971491514 ) ) ;
#26636 = EDGE_LOOP ( 'NONE', ( #22100, #8842, #23023, #22630, #20301 ) ) ;
#26637 = ORIENTED_EDGE ( 'NONE', *, *, #29792, .T. ) ;
#26638 = CARTESIAN_POINT ( 'NONE',  ( -0.3000000000000000999, -3.811657270145150989, -0.1642545796697100491 ) ) ;
#26639 = CARTESIAN_POINT ( 'NONE',  ( 0.4400409819278914836, -1.228797560110408416, 0.5880944087261866793 ) ) ;
#26640 = CARTESIAN_POINT ( 'NONE',  ( -0.04139678531769541009, 0.4525211694413263097, -0.1291682248591896620 ) ) ;
#26641 = ORIENTED_EDGE ( 'NONE', *, *, #3126, .F. ) ;
#26642 = CARTESIAN_POINT ( 'NONE',  ( 0.08368236660537471672, -1.307117728175614335, 0.5699627548592203219 ) ) ;
#26643 = CARTESIAN_POINT ( 'NONE',  ( 0.09173077349526245761, -0.6925701938402700764, 0.2560274467086400274 ) ) ;
#26644 = CARTESIAN_POINT ( 'NONE',  ( 0.2705976637934949802, -1.541701018061943484, 0.9966701210605140027 ) ) ;
#26645 = CARTESIAN_POINT ( 'NONE',  ( 0.4714652189410261651, -1.557192263116904618, 0.6121692311124370400 ) ) ;
#26647 = CYLINDRICAL_SURFACE ( 'NONE', #14327, 0.03000000000000003358 ) ;
#26646 = CARTESIAN_POINT ( 'NONE',  ( 0.1138085506330038799, -0.5805959105637907847, -0.07044495644018930469 ) ) ;
#26648 = CARTESIAN_POINT ( 'NONE',  ( 0.09374999999999995837, -0.9316581899787156340, 0.1618212499200845089 ) ) ;
#26649 = VERTEX_POINT ( 'NONE', #672 ) ;
#26650 = VECTOR ( 'NONE', #2738, 39.37007874015748854 ) ;
#26651 = EDGE_CURVE ( 'NONE', #40017, #18976, #29213, .T. ) ;
#26652 = DIRECTION ( 'NONE',  ( 0.000000000000000000, -0.1725921171159288392, 0.9849933812515907494 ) ) ;
#26653 = CARTESIAN_POINT ( 'NONE',  ( 0.1434650259794786331, -0.5695106312979485441, 0.4826513458886010910 ) ) ;
#26654 = AXIS2_PLACEMENT_3D ( 'NONE', #3459, #19103, #12934 ) ;
#26655 = ADVANCED_FACE ( 'NONE', ( #10087 ), #22659, .F. ) ;
#26656 = LINE ( 'NONE', #32790, #37781 ) ;
#26657 = SECURITY_CLASSIFICATION ( '', '', #25794 ) ;
#26658 = CARTESIAN_POINT ( 'NONE',  ( -0.05268850283020218989, -0.4442517014320102597, -0.1491954418488743439 ) ) ;
#26659 = DIRECTION ( 'NONE',  ( -0.4999551463232377313, 0.8660512985181132439, 0.000000000000000000 ) ) ;
#26660 = CARTESIAN_POINT ( 'NONE',  ( 0.3778447279644155388, -0.9516834458091659732, 0.7020028943473471950 ) ) ;
#26661 = PLANE ( 'NONE',  #21440 ) ;
#26662 = CARTESIAN_POINT ( 'NONE',  ( 0.1457829054851000339, -1.333675122505752375, -0.3151394128761840774 ) ) ;
#26663 = CARTESIAN_POINT ( 'NONE',  ( 0.4317743168343897153, -1.612353136874114634, -0.6636800572944283605 ) ) ;
#26664 = ORIENTED_EDGE ( 'NONE', *, *, #2205, .T. ) ;
#26665 = CARTESIAN_POINT ( 'NONE',  ( 0.1359911470193229943, -1.231045907863504763, -0.5155029497116575543 ) ) ;
#26666 = CARTESIAN_POINT ( 'NONE',  ( 0.3984114568195520345, -1.599003643269838904, -0.5155029497116575543 ) ) ;
#26667 = CARTESIAN_POINT ( 'NONE',  ( -0.04574984450155145793, -0.2311445325521683802, -0.4288136795716587235 ) ) ;
#26668 = VERTEX_POINT ( 'NONE', #26150 ) ;
#26669 = DIRECTION ( 'NONE',  ( -8.881784197001246407E-16, 2.361472542561082612E-16, -1.000000000000000000 ) ) ;
#26670 = CARTESIAN_POINT ( 'NONE',  ( -0.05634304521267782806, 0.01028123094838855403, -0.4588823192046729837 ) ) ;
#26671 = DIRECTION ( 'NONE',  ( 5.551115123125797493E-17, -5.306893166658304503E-16, -1.000000000000000000 ) ) ;
#26672 = AXIS2_PLACEMENT_3D ( 'NONE', #2183, #23596, #11223 ) ;
#26673 = AXIS2_PLACEMENT_3D ( 'NONE', #21074, #33599, #17974 ) ;
#26674 = CARTESIAN_POINT ( 'NONE',  ( 0.2330814885300186434, -1.234478371153929555, 0.7248379463662146804 ) ) ;
#26675 = EDGE_LOOP ( 'NONE', ( #18441, #23601 ) ) ;
#26676 = CARTESIAN_POINT ( 'NONE',  ( -0.03664605387828210464, 0.3149102792626774505, 0.3635688186731549920 ) ) ;
#26677 = CARTESIAN_POINT ( 'NONE',  ( 0.05999999999999990757, 0.000000000000000000, 0.000000000000000000 ) ) ;
#26678 = APPLIED_APPROVAL_ASSIGNMENT ( #27757, ( #11907 ) ) ;
#26679 = CARTESIAN_POINT ( 'NONE',  ( 0.3992403239432529283, -1.683235622436187073, -0.6263438071736542323 ) ) ;
#26680 = DIRECTION ( 'NONE',  ( 1.000000000000000000, 0.000000000000000000, 1.138269997360110167E-15 ) ) ;
#26681 = CARTESIAN_POINT ( 'NONE',  ( 0.4332292389763821028, -1.186803953203684703, 0.6662783122723310303 ) ) ;
#26683 = CARTESIAN_POINT ( 'NONE',  ( 0.5789220659479127340, -1.645056496184873929, -0.5155029497116575543 ) ) ;
#26682 = LINE ( 'NONE', #27068, #22667 ) ;
#26684 = CARTESIAN_POINT ( 'NONE',  ( 0.1916709472725509622, -0.9174159909098704713, 0.2459055916410233245 ) ) ;
#26685 = ORIENTED_EDGE ( 'NONE', *, *, #36722, .F. ) ;
#26686 = CIRCLE ( 'NONE', #6306, 0.01500000000000004455 ) ;
#26687 = CARTESIAN_POINT ( 'NONE',  ( 0.5893629127802496592, -1.590949893388290404, 0.4182417262808776903 ) ) ;
#26688 = EDGE_LOOP ( 'NONE', ( #11890, #36210, #2728 ) ) ;
#26689 =( BOUNDED_SURFACE ( )  B_SPLINE_SURFACE ( 3, 2, ( 
 ( #4747, #30477, #14847 ),
 ( #39936, #17320, #20621 ),
 ( #33758, #11345, #2089 ),
 ( #11752, #2306, #26797 ),
 ( #29876, #8045, #33157 ),
 ( #20829, #1715, #23703 ),
 ( #10958, #24311, #2506 ),
 ( #23519, #36834, #8651 ),
 ( #14626, #8453, #4962 ),
 ( #15046, #21222, #14417 ),
 ( #36034, #27196, #33350 ),
 ( #5572, #39730, #14232 ) ),
 .UNSPECIFIED., .F., .F., .T. ) 
 B_SPLINE_SURFACE_WITH_KNOTS ( ( 4, 2, 2, 2, 2, 4 ),
 ( 3, 3 ),
 ( 0.000000000000000000, 0.0002157422512141129838, 0.0004314845024282259675, 0.0008629690048564519350, 0.001294453507284677903, 0.001725938009712903870 ),
 ( 0.000000000000000000, 1.000000000000000000 ),
 .UNSPECIFIED. ) 
 GEOMETRIC_REPRESENTATION_ITEM ( )  RATIONAL_B_SPLINE_SURFACE ( (
 ( 1.000000000000000000, 0.8660688067375535981, 1.000000000000000000),
 ( 1.000000000000000000, 0.8654212037204194186, 1.000000000000000000),
 ( 1.000000000000000000, 0.8620557401133326358, 1.000000000000000000),
 ( 1.000000000000000000, 0.8506860164930378776, 1.000000000000000000),
 ( 1.000000000000000000, 0.8429438875099044548, 1.000000000000000000),
 ( 1.000000000000000000, 0.8190090774808674867, 1.000000000000000000),
 ( 1.000000000000000000, 0.8018511170037568858, 1.000000000000000000),
 ( 1.000000000000000000, 0.7696825608641452154, 1.000000000000000000),
 ( 1.000000000000000000, 0.7540990922196469937, 1.000000000000000000),
 ( 1.000000000000000000, 0.7234792338946504087, 1.000000000000000000),
 ( 1.000000000000000000, 0.7084058450330773526, 1.000000000000000000),
 ( 1.000000000000000000, 0.6936380329425325675, 1.000000000000000000) ) ) 
 REPRESENTATION_ITEM ( '' )  SURFACE ( )  );
#26690 = CARTESIAN_POINT ( 'NONE',  ( 0.1845258802888041783, -0.7337134285967986669, 0.05501147976861575639 ) ) ;
#26691 = CARTESIAN_POINT ( 'NONE',  ( 0.3649957450613842136, -1.468351375757600996, 0.8486509050985698854 ) ) ;
#26693 = CARTESIAN_POINT ( 'NONE',  ( 0.08989780363036058153, -0.5646359461869331353, 0.1460065308160271857 ) ) ;
#26692 = CARTESIAN_POINT ( 'NONE',  ( 0.06762866613896016676, -0.6210165958772466688, 0.01354926383832238783 ) ) ;
#26694 = CARTESIAN_POINT ( 'NONE',  ( 0.1806790351422245811, -1.790997932741038801, -0.3531985826763806569 ) ) ;
#26695 = ORIENTED_EDGE ( 'NONE', *, *, #14506, .T. ) ;
#26696 = VERTEX_POINT ( 'NONE', #38665 ) ;
#26697 = CARTESIAN_POINT ( 'NONE',  ( -0.3000000000000000999, -2.423474325126674156, -0.5576739111151495232 ) ) ;
#26698 = CARTESIAN_POINT ( 'NONE',  ( 0.5739388401085829816, -1.499262904232843807, 0.5736237701463445804 ) ) ;
#26699 = EDGE_LOOP ( 'NONE', ( #34188, #18267, #22948, #1642 ) ) ;
#26700 = DIRECTION ( 'NONE',  ( 0.000000000000000000, 0.000000000000000000, -1.000000000000000000 ) ) ;
#26701 = CARTESIAN_POINT ( 'NONE',  ( 0.04946426091936331065, -0.4635716124040255570, 0.1136627969334474547 ) ) ;
#26702 = CARTESIAN_POINT ( 'NONE',  ( 0.6060475248853955943, -1.581096070219540239, 0.4182417262808776903 ) ) ;
#26703 = CARTESIAN_POINT ( 'NONE',  ( 0.1896833470237338504, -1.257561668833873103, 0.4318233238025492304 ) ) ;
#26704 = CARTESIAN_POINT ( 'NONE',  ( -0.1655961216393967705, 0.4810575411953303959, 0.1221435944151030156 ) ) ;
#26705 = LINE ( 'NONE', #7548, #37821 ) ;
#26706 = AXIS2_PLACEMENT_3D ( 'NONE', #35981, #7366, #17258 ) ;
#26707 = CARTESIAN_POINT ( 'NONE',  ( 0.7168528728721502707, -1.464418552067108470, 0.6746166867755808427 ) ) ;
#26708 = CARTESIAN_POINT ( 'NONE',  ( 0.3625960434667531151, -1.762758894398492204, -0.5926935080085831142 ) ) ;
#26709 = FACE_OUTER_BOUND ( 'NONE', #34968, .T. ) ;
#26710 = ORGANIZATION ( 'NAUO-ORG4', 'UNSPECIFIED', 'UNSPECIFIED' ) ;
#26711 = CARTESIAN_POINT ( 'NONE',  ( 0.6069444678199540366, -1.586721832627447037, -0.5605626994862983326 ) ) ;
#26712 = CARTESIAN_POINT ( 'NONE',  ( 0.000000000000000000, -0.1022126893003200560, -0.2231384537392532841 ) ) ;
#26713 = CARTESIAN_POINT ( 'NONE',  ( 0.000000000000000000, -0.05999999999999990757, 0.000000000000000000 ) ) ;
#26714 = DIRECTION ( 'NONE',  ( -9.042510699458645841E-13, 1.566396143878659165E-12, -1.000000000000000000 ) ) ;
#26715 = VECTOR ( 'NONE', #9068, 39.37007874015748854 ) ;
#26716 = CARTESIAN_POINT ( 'NONE',  ( 0.08609895781566062611, -1.325383763084707400, 0.4606884510573937552 ) ) ;
#26717 = CARTESIAN_POINT ( 'NONE',  ( 0.1802350563441833808, -0.5022327775090948965, 0.1477559389858786043 ) ) ;
#26718 = CARTESIAN_POINT ( 'NONE',  ( 0.5769685703849426472, -1.564106961903302784, -0.4421163036608469765 ) ) ;
#26719 = CARTESIAN_POINT ( 'NONE',  ( -1.545739608871925730E-14, -2.094379624154600883, -0.2600525927961437334 ) ) ;
#26720 = CARTESIAN_POINT ( 'NONE',  ( 0.6011193747858225578, -1.595581932925099977, 0.4276689662439276396 ) ) ;
#26721 = CARTESIAN_POINT ( 'NONE',  ( -0.03174036153404242999, -0.3664551212196091035, 0.3753291932915900353 ) ) ;
#26722 = B_SPLINE_CURVE_WITH_KNOTS ( 'NONE', 3,
 ( #12525, #34330, #36799, #18301, #5532, #6141, #33943, #24277, #9224, #9436, #2472, #34126 ),
 .UNSPECIFIED., .F., .F.,
 ( 4, 2, 2, 2, 2, 4 ),
 ( 0.004565700224486055406, 0.005703496875624043498, 0.006272395201193034509, 0.006841293526762026386, 0.007979090177900018815, 0.009116886829038009510 ),
 .UNSPECIFIED. ) ;
#26723 = VERTEX_POINT ( 'NONE', #1265 ) ;
#26724 = ORIENTED_EDGE ( 'NONE', *, *, #7152, .T. ) ;
#26725 = CARTESIAN_POINT ( 'NONE',  ( 0.3211756810167746834, -1.183199798883805887, 0.5707417262808780478 ) ) ;
#26726 = ORIENTED_EDGE ( 'NONE', *, *, #32055, .T. ) ;
#26727 = DIRECTION ( 'NONE',  ( 0.000000000000000000, 0.000000000000000000, 1.000000000000000000 ) ) ;
#26728 = CARTESIAN_POINT ( 'NONE',  ( 0.03303737228521891334, 0.2303602220530218125, -0.4672390599430968350 ) ) ;
#26729 = CARTESIAN_POINT ( 'NONE',  ( 0.5552614681345688918, -1.388647501241920157, 0.5981693664984994996 ) ) ;
#26731 = VERTEX_POINT ( 'NONE', #13968 ) ;
#26730 = CARTESIAN_POINT ( 'NONE',  ( 0.2625876981780432828, -0.6796766824346859304, 0.2386862984125060760 ) ) ;
#26732 = CARTESIAN_POINT ( 'NONE',  ( 0.4004013247085298488, -1.001184149470538909, 0.6774742858917212063 ) ) ;
#26733 = VECTOR ( 'NONE', #19212, 39.37007874015748143 ) ;
#26734 = CYLINDRICAL_SURFACE ( 'NONE', #9260, 0.1000000000000000056 ) ;
#26735 = ORIENTED_EDGE ( 'NONE', *, *, #8697, .T. ) ;
#26736 = CARTESIAN_POINT ( 'NONE',  ( 0.3272356563838212384, -1.639253224411857390, 0.5768921858655433610 ) ) ;
#26738 = CARTESIAN_POINT ( 'NONE',  ( 0.1765207216392534473, -0.5289821624952937285, -0.02115802863982717275 ) ) ;
#26737 = CARTESIAN_POINT ( 'NONE',  ( 0.6663393932594230407, -1.528864674313891614, 0.4320056365155769407 ) ) ;
#26739 = CARTESIAN_POINT ( 'NONE',  ( 0.4971324743577882899, -1.079965756743124006, 0.4177417262808780229 ) ) ;
#26740 = LOCAL_TIME ( 0, 53, 7.000000000000000000, #14009 ) ;
#26741 = CARTESIAN_POINT ( 'NONE',  ( 0.1690117501680792333, -1.307634958409015669, -0.3044763796399118094 ) ) ;
#26742 = ORIENTED_EDGE ( 'NONE', *, *, #33898, .T. ) ;
#26743 = CARTESIAN_POINT ( 'NONE',  ( -0.2399999999999999079, -3.941790907013290823, -0.4709369376873030477 ) ) ;
#26744 = CARTESIAN_POINT ( 'NONE',  ( 0.07228386787129255364, -1.414757321928298950, -0.6600343213859931613 ) ) ;
#26745 = CARTESIAN_POINT ( 'NONE',  ( 0.03158843595483477179, 0.4482533282648965556, 0.2030547983902457332 ) ) ;
#26746 = CARTESIAN_POINT ( 'NONE',  ( 0.1484580525513722604, -0.9426921462834582099, 0.6469761069243887830 ) ) ;
#26747 = CARTESIAN_POINT ( 'NONE',  ( 0.1909286924077255032, -1.257064795538239022, -0.3194753470178354759 ) ) ;
#26748 = APPLIED_PERSON_AND_ORGANIZATION_ASSIGNMENT ( #23738, #19287, ( #29284 ) ) ;
#26749 = CARTESIAN_POINT ( 'NONE',  ( 0.5140855864883536741, -1.668539606441037826, -0.5966333239037243663 ) ) ;
#26750 = B_SPLINE_CURVE_WITH_KNOTS ( 'NONE', 3,
 ( #13097, #603, #25656, #7303 ),
 .UNSPECIFIED., .F., .F.,
 ( 4, 4 ),
 ( 0.01492582395562414704, 0.01617680779535383279 ),
 .UNSPECIFIED. ) ;
#26751 = CARTESIAN_POINT ( 'NONE',  ( 0.1284469837844391393, -0.9382340779789365426, 0.3427534698529470791 ) ) ;
#26752 = CARTESIAN_POINT ( 'NONE',  ( -0.01548846960707524721, 0.09061086148576029398, -0.5171215251571035232 ) ) ;
#26753 = DIRECTION ( 'NONE',  ( 0.000000000000000000, -0.5877852522924855716, 0.8090169943749384585 ) ) ;
#26754 = CARTESIAN_POINT ( 'NONE',  ( 0.6531523644885445234, -1.470371462098315263, 0.4182417262808779124 ) ) ;
#26755 = FACE_OUTER_BOUND ( 'NONE', #10325, .T. ) ;
#26756 = APPROVAL_STATUS ( 'not_yet_approved' ) ;
#26757 = AXIS2_PLACEMENT_3D ( 'NONE', #33984, #5789, #885 ) ;
#26758 = CARTESIAN_POINT ( 'NONE',  ( 0.4120248911441328765, -1.141963342659028102, 0.4320455384514549357 ) ) ;
#26759 = DIRECTION ( 'NONE',  ( -1.000000000000000000, -6.779273404243070203E-32, -4.314083075427408311E-32 ) ) ;
#26760 = CARTESIAN_POINT ( 'NONE',  ( -0.3000000000000000999, -1.906460133321048911, -0.3231213194042101278 ) ) ;
#26761 = EDGE_CURVE ( 'NONE', #7506, #7962, #7332, .T. ) ;
#26762 = ORIENTED_EDGE ( 'NONE', *, *, #950, .T. ) ;
#26763 = CARTESIAN_POINT ( 'NONE',  ( 0.01208707464876302047, -0.4498900264573193475, 0.04206197065121651535 ) ) ;
#26764 = CARTESIAN_POINT ( 'NONE',  ( 0.3681929541678355400, -1.759371874277346537, -0.5873187883762895911 ) ) ;
#26765 = LINE ( 'NONE', #32908, #15972 ) ;
#26766 = CYLINDRICAL_SURFACE ( 'NONE', #9859, 0.2200000000000000289 ) ;
#26767 = ORIENTED_EDGE ( 'NONE', *, *, #23412, .T. ) ;
#26768 = EDGE_CURVE ( 'NONE', #20753, #22989, #14795, .T. ) ;
#26769 = ORIENTED_EDGE ( 'NONE', *, *, #10795, .F. ) ;
#26770 = CARTESIAN_POINT ( 'NONE',  ( 0.1767184732304685202, -0.4886261860184148431, 0.1375861377844761757 ) ) ;
#26771 = ORIENTED_EDGE ( 'NONE', *, *, #30275, .T. ) ;
#26772 = EDGE_CURVE ( 'NONE', #22699, #30555, #22167, .T. ) ;
#26774 = VERTEX_POINT ( 'NONE', #36600 ) ;
#26773 = CARTESIAN_POINT ( 'NONE',  ( 0.1345576988209646330, -0.5547214491096114086, 0.1783673147042096618 ) ) ;
#26775 = ADVANCED_FACE ( 'NONE', ( #7796 ), #7990, .T. ) ;
#26777 = ORIENTED_EDGE ( 'NONE', *, *, #128, .T. ) ;
#26776 = CARTESIAN_POINT ( 'NONE',  ( -0.0004183621434831840237, -0.7293707673872504849, -0.008477467720215554545 ) ) ;
#26778 = EDGE_CURVE ( 'NONE', #27000, #18456, #9999, .T. ) ;
#26779 = B_SPLINE_CURVE_WITH_KNOTS ( 'NONE', 3,
 ( #40556, #20280, #6798, #22462, #37672, #34781 ),
 .UNSPECIFIED., .F., .F.,
 ( 4, 2, 4 ),
 ( 0.000000000000000000, 0.5000000000000000000, 1.000000000000000000 ),
 .UNSPECIFIED. ) ;
#26780 = ORIENTED_EDGE ( 'NONE', *, *, #25102, .F. ) ;
#26781 = CARTESIAN_POINT ( 'NONE',  ( -0.1603938765018537715, 0.4636889572247753222, 0.1178658435936994903 ) ) ;
#26782 = ORIENTED_EDGE ( 'NONE', *, *, #20227, .T. ) ;
#26783 = CARTESIAN_POINT ( 'NONE',  ( -0.009205357870253665087, -0.5919609180146404581, 0.3621894606988042553 ) ) ;
#26785 = CARTESIAN_POINT ( 'NONE',  ( 0.1428314273233315668, -1.273136066146236312, 0.6057341954371575632 ) ) ;
#26784 = CYLINDRICAL_SURFACE ( 'NONE', #30541, 0.1000000000000000194 ) ;
#26786 = CARTESIAN_POINT ( 'NONE',  ( 0.6438069108991687495, -1.607599694021685899, -0.4632284051550286108 ) ) ;
#26787 = DATE_AND_TIME ( #23300, #22816 ) ;
#26788 = LINE ( 'NONE', #20820, #28367 ) ;
#26790 = ORIENTED_EDGE ( 'NONE', *, *, #15186, .F. ) ;
#26789 = ORIENTED_EDGE ( 'NONE', *, *, #24482, .T. ) ;
#26791 = CARTESIAN_POINT ( 'NONE',  ( 0.2352121309571624796, -0.9559301127563956113, 0.6564793400487810571 ) ) ;
#26792 = CARTESIAN_POINT ( 'NONE',  ( 0.06985341656399968180, -0.5484169138694637846, 0.2034521178982568179 ) ) ;
#26793 = CARTESIAN_POINT ( 'NONE',  ( 0.5525824764865431282, -1.511072664810155786, 0.5658631727751453067 ) ) ;
#26794 = CARTESIAN_POINT ( 'NONE',  ( 0.02382395405342765254, -1.023441010626642944, 0.5576374536115574765 ) ) ;
#26795 = EDGE_CURVE ( 'NONE', #2874, #35762, #11293, .T. ) ;
#26796 = CARTESIAN_POINT ( 'NONE',  ( 0.6544078563150221850, -1.544269123161552626, 0.4241055859090109292 ) ) ;
#26797 = CARTESIAN_POINT ( 'NONE',  ( 0.3883097432465577592, -1.693085907158164538, -0.4088198505623931722 ) ) ;
#26798 = CARTESIAN_POINT ( 'NONE',  ( 0.6841302653033145553, -1.411212316466117223, 0.6057417262805112612 ) ) ;
#26799 = B_SPLINE_CURVE_WITH_KNOTS ( 'NONE', 3,
 ( #33142, #8856, #8637, #21210, #5148, #27401 ),
 .UNSPECIFIED., .F., .F.,
 ( 4, 2, 4 ),
 ( 0.000000000000000000, 0.2508149426252075376, 0.5016298852504150751 ),
 .UNSPECIFIED. ) ;
#26800 = CARTESIAN_POINT ( 'NONE',  ( 0.1876053338355621880, -0.6785855078148245179, 0.1477569985384105666 ) ) ;
#26801 = FACE_OUTER_BOUND ( 'NONE', #33178, .T. ) ;
#26802 = DIRECTION ( 'NONE',  ( -1.000000000000000000, -0.000000000000000000, -0.000000000000000000 ) ) ;
#26803 = CARTESIAN_POINT ( 'NONE',  ( 6.726208831336936099E-05, -0.6219379412995073020, -0.09511945894820450498 ) ) ;
#26804 = CARTESIAN_POINT ( 'NONE',  ( 0.3443170205183039845, -1.640114790049758353, -0.3775635453920966333 ) ) ;
#26805 = SHAPE_REPRESENTATION_RELATIONSHIP ( 'NONE' , 'NONE' ,  #21742, #7338 ) ;
#26806 = CARTESIAN_POINT ( 'NONE',  ( 0.6275005400096769215, -1.601790509832649922, -0.5777336405445359091 ) ) ;
#26807 = CARTESIAN_POINT ( 'NONE',  ( 0.01037466073212112323, -0.7737952308255096057, 0.4846566707863347867 ) ) ;
#26808 = CARTESIAN_POINT ( 'NONE',  ( 0.2471460726071840197, -0.9121693139129607442, 0.4829066783201274027 ) ) ;
#26809 = PERSON_AND_ORGANIZATION ( #28500, #32463 ) ;
#26810 = CARTESIAN_POINT ( 'NONE',  ( 0.4812359531826634340, -1.078470577594583979, 0.8616913018466071383 ) ) ;
#26811 = CARTESIAN_POINT ( 'NONE',  ( 0.3672875303838389338, -1.616970901354834789, -0.6123576500872190964 ) ) ;
#26812 = CARTESIAN_POINT ( 'NONE',  ( 0.3187434959594735995, -1.760361270025436742, 0.5680051819931960511 ) ) ;
#26813 = ADVANCED_FACE ( 'NONE', ( #29822 ), #11706, .F. ) ;
#26814 = ORIENTED_EDGE ( 'NONE', *, *, #25857, .F. ) ;
#26815 = DIRECTION ( 'NONE',  ( 0.8660512985181134660, 0.4999551463232372872, 0.000000000000000000 ) ) ;
#26816 = CARTESIAN_POINT ( 'NONE',  ( 0.1487004007006368367, -1.233131608729471695, 0.9291103107006072337 ) ) ;
#26817 = EDGE_CURVE ( 'NONE', #15882, #33666, #20364, .T. ) ;
#26818 = CARTESIAN_POINT ( 'NONE',  ( 0.2144290776330740889, -1.231722763067022219, 0.4813240406935799798 ) ) ;
#26820 = EDGE_LOOP ( 'NONE', ( #32310, #14776, #22317, #17458 ) ) ;
#26819 = CARTESIAN_POINT ( 'NONE',  ( 0.4577135909791524848, -1.717961013370186141, 0.5182417262812423209 ) ) ;
#26821 = CARTESIAN_POINT ( 'NONE',  ( 0.1141309172362124369, 0.06118878220587050526, -0.05231945263244261457 ) ) ;
#26822 = EDGE_CURVE ( 'NONE', #35653, #14911, #33100, .T. ) ;
#26823 = TOROIDAL_SURFACE ( 'NONE', #11719, 0.08249999999977548903, 0.01000000000000000021 ) ;
#26824 = CARTESIAN_POINT ( 'NONE',  ( 0.5633629393321837320, -1.208205391268785567, 0.7270432621192387534 ) ) ;
#26826 = EDGE_LOOP ( 'NONE', ( #6613, #35759 ) ) ;
#26825 = EDGE_LOOP ( 'NONE', ( #21819, #32784, #31064 ) ) ;
#26827 = CARTESIAN_POINT ( 'NONE',  ( 0.01266905423176017606, -1.700475420996584885, -0.6376096380771161254 ) ) ;
#26828 = ORIENTED_EDGE ( 'NONE', *, *, #18200, .F. ) ;
#26829 = CARTESIAN_POINT ( 'NONE',  ( 0.6457670174492194937, -1.456209924560479152, -0.4058631681734992669 ) ) ;
#26830 = DIRECTION ( 'NONE',  ( 0.000000000000000000, 0.000000000000000000, 1.000000000000000000 ) ) ;
#26831 = APPROVAL_STATUS ( 'not_yet_approved' ) ;
#26832 = CARTESIAN_POINT ( 'NONE',  ( -0.05491348488830481017, 0.4316112672892382651, -0.1667783590291073981 ) ) ;
#26833 = ORIENTED_EDGE ( 'NONE', *, *, #2712, .T. ) ;
#26834 = CARTESIAN_POINT ( 'NONE',  ( -19685.04193433331602, 285.7890798983738136, -1.951739244310253252 ) ) ;
#26835 = CARTESIAN_POINT ( 'NONE',  ( 0.2042160338947917320, -0.8611997158126063479, 0.6444930625586713369 ) ) ;
#26836 = CARTESIAN_POINT ( 'NONE',  ( 0.2902408836998817687, -1.617250972615089433, 0.9506298565161998004 ) ) ;
#26837 = CARTESIAN_POINT ( 'NONE',  ( 0.4886971128151171295, -1.518144040485195800, 0.7197715497223399206 ) ) ;
#26839 = DIRECTION ( 'NONE',  ( 1.000000000000000000, -1.681422630952717046E-11, 5.294072836416690161E-12 ) ) ;
#26838 = CARTESIAN_POINT ( 'NONE',  ( 0.2692931055722388445, -1.652497923304702132, 0.7773017355661825389 ) ) ;
#26840 = EDGE_CURVE ( 'NONE', #36726, #19301, #34372, .T. ) ;
#26841 = CARTESIAN_POINT ( 'NONE',  ( 0.2325857081196134601, -1.005531832322530184, 0.5832656420552320142 ) ) ;
#26842 = EDGE_LOOP ( 'NONE', ( #15435, #34740, #32124, #12001 ) ) ;
#26843 = EDGE_LOOP ( 'NONE', ( #13284, #457, #12931, #15290 ) ) ;
#26844 = CARTESIAN_POINT ( 'NONE',  ( 0.04582713223189449625, -0.4790191777205495827, -0.08746099429787949908 ) ) ;
#26845 = EDGE_CURVE ( 'NONE', #2801, #39344, #8403, .T. ) ;
#26846 = CARTESIAN_POINT ( 'NONE',  ( 0.2356700409021097453, -0.6918407148733107803, 0.4984434980982429542 ) ) ;
#26847 = CARTESIAN_POINT ( 'NONE',  ( -0.03301200226531658677, 0.2303790867044800128, -0.4673050311136111024 ) ) ;
#26848 = LINE ( 'NONE', #16970, #25866 ) ;
#26849 = CARTESIAN_POINT ( 'NONE',  ( 0.07457743601771446573, -1.318870387072609507, 0.4957195692065117787 ) ) ;
#26850 = CARTESIAN_POINT ( 'NONE',  ( 0.3944272916047369404, -1.765189661685290901, -0.7095092544234420373 ) ) ;
#26851 = DIRECTION ( 'NONE',  ( -0.4999551463232373427, 0.8660512985181134660, -0.000000000000000000 ) ) ;
#26852 = CARTESIAN_POINT ( 'NONE',  ( 0.4529286794724542986, -1.051290237540063455, 0.7432202178062045084 ) ) ;
#26853 = DIRECTION ( 'NONE',  ( 0.000000000000000000, 0.000000000000000000, -1.000000000000000000 ) ) ;
#26854 = CARTESIAN_POINT ( 'NONE',  ( 0.02998309779899579336, -2.054017904330772470, -0.2742168981856276666 ) ) ;
#26855 = CARTESIAN_POINT ( 'NONE',  ( -0.2399999999999999079, -2.183180860297908144, -0.4312760292030870524 ) ) ;
#26856 = ORIENTED_EDGE ( 'NONE', *, *, #31928, .T. ) ;
#26857 = CARTESIAN_POINT ( 'NONE',  ( -0.1157923916715205420, -0.5295015842444287246, 0.3749999999999992784 ) ) ;
#26858 = CYLINDRICAL_SURFACE ( 'NONE', #18586, 0.6115209409081865388 ) ;
#26859 = DIRECTION ( 'NONE',  ( 0.000000000000000000, 0.000000000000000000, 1.000000000000000000 ) ) ;
#26860 = ORIENTED_EDGE ( 'NONE', *, *, #39057, .T. ) ;
#26861 = DIRECTION ( 'NONE',  ( -0.000000000000000000, -0.000000000000000000, 1.000000000000000000 ) ) ;
#26862 = EDGE_CURVE ( 'NONE', #25919, #25464, #29494, .T. ) ;
#26863 = B_SPLINE_CURVE_WITH_KNOTS ( 'NONE', 3,
 ( #1870, #17675, #24280, #14196 ),
 .UNSPECIFIED., .F., .F.,
 ( 4, 4 ),
 ( 0.000000000000000000, 0.0008899773499878894933 ),
 .UNSPECIFIED. ) ;
#26864 = CARTESIAN_POINT ( 'NONE',  ( 0.3925301276612754298, -1.756377271995033684, -0.4843757382520948451 ) ) ;
#26865 = CARTESIAN_POINT ( 'NONE',  ( 0.2557456068137679006, -1.277973818264130479, 0.6877359101403667241 ) ) ;
#26866 = ORIENTED_EDGE ( 'NONE', *, *, #31034, .T. ) ;
#26867 = CARTESIAN_POINT ( 'NONE',  ( 0.02953079040095700838, 0.2329676531120518090, 0.4763574306556300764 ) ) ;
#26868 = DIRECTION ( 'NONE',  ( 0.000000000000000000, -0.5877852522924748024, -0.8090169943749461190 ) ) ;
#26869 = DIRECTION ( 'NONE',  ( -1.000000000000000000, -2.280301054154495132E-31, 1.664003471950577689E-31 ) ) ;
#26870 = CARTESIAN_POINT ( 'NONE',  ( -0.02000000000000000042, -2.183180860297908144, -0.4937760292030871079 ) ) ;
#26871 = CARTESIAN_POINT ( 'NONE',  ( 0.4681644054017271572, -1.238292871408442686, 0.5986446648243279878 ) ) ;
#26873 = DIRECTION ( 'NONE',  ( 0.000000000000000000, 0.000000000000000000, 1.000000000000000000 ) ) ;
#26872 = FACE_OUTER_BOUND ( 'NONE', #30848, .T. ) ;
#26874 = CARTESIAN_POINT ( 'NONE',  ( -0.05082303569918705799, -0.2375724430107435947, -0.4097459652473651182 ) ) ;
#26875 = ORIENTED_EDGE ( 'NONE', *, *, #28339, .F. ) ;
#26876 = CARTESIAN_POINT ( 'NONE',  ( 0.3538719729184752749, -1.624715450675502160, 0.4182417262808775238 ) ) ;
#26877 = ORIENTED_EDGE ( 'NONE', *, *, #3444, .T. ) ;
#26878 = CARTESIAN_POINT ( 'NONE',  ( 0.1915883296772408761, -0.5477411782657776174, 0.1479976049341028554 ) ) ;
#26879 = CARTESIAN_POINT ( 'NONE',  ( 0.06043570224876768787, -0.5391841548082976221, 0.1632230437248760602 ) ) ;
#26881 = PLANE ( 'NONE',  #26182 ) ;
#26880 = CARTESIAN_POINT ( 'NONE',  ( 0.08926425616020196296, -0.5615075463834332536, 0.07548189203980994189 ) ) ;
#26882 = CARTESIAN_POINT ( 'NONE',  ( 0.1176807611043763635, -1.298951677446983588, 0.5132863183563353138 ) ) ;
#26883 = EDGE_CURVE ( 'NONE', #12740, #28384, #9815, .T. ) ;
#26884 = ORIENTED_EDGE ( 'NONE', *, *, #12737, .F. ) ;
#26885 = ORIENTED_EDGE ( 'NONE', *, *, #18050, .F. ) ;
#26886 = EDGE_CURVE ( 'NONE', #5500, #32636, #36845, .T. ) ;
#26887 = DIRECTION ( 'NONE',  ( 1.000000000000000000, 0.000000000000000000, 0.000000000000000000 ) ) ;
#26888 = CARTESIAN_POINT ( 'NONE',  ( 0.1203440671115274391, -0.5719449301461521085, 0.2477259942629035927 ) ) ;
#26889 = VERTEX_POINT ( 'NONE', #12321 ) ;
#26890 = DIRECTION ( 'NONE',  ( 0.000000000000000000, 0.000000000000000000, 1.000000000000000000 ) ) ;
#26891 = CARTESIAN_POINT ( 'NONE',  ( 0.02881408050861556172, -0.4517606495562037083, 0.2100211630561500953 ) ) ;
#26892 = ADVANCED_FACE ( 'NONE', ( #34112 ), #21, .F. ) ;
#26893 = FACE_OUTER_BOUND ( 'NONE', #38945, .T. ) ;
#26894 = PRODUCT_DEFINITION_SHAPE ( 'NONE', 'NONE',  #2626 ) ;
#26895 = CARTESIAN_POINT ( 'NONE',  ( 0.2004112705531303495, -1.239815393329114723, 0.4579970032064163976 ) ) ;
#26896 = CARTESIAN_POINT ( 'NONE',  ( 0.002290818369124609372, -0.5198888459286679087, 0.1457185332388686583 ) ) ;
#26897 = DIRECTION ( 'NONE',  ( 0.000000000000000000, 0.9510565162951443163, 0.3090169943749759840 ) ) ;
#26898 = CARTESIAN_POINT ( 'NONE',  ( 0.7185393139234729221, -1.479621239843056157, 0.4933132820244564565 ) ) ;
#26899 = CARTESIAN_POINT ( 'NONE',  ( 0.03113248654051816583, -0.3458405862425447119, -0.2052451372150005393 ) ) ;
#26900 = DIRECTION ( 'NONE',  ( 1.000000000000000000, 0.000000000000000000, 0.000000000000000000 ) ) ;
#26901 = CARTESIAN_POINT ( 'NONE',  ( 0.5896330274811124594, -1.594592002126501429, -0.5907196032396619945 ) ) ;
#26902 = CARTESIAN_POINT ( 'NONE',  ( 0.05201782277453504549, 0.2617104306118889223, 0.3909705171288710424 ) ) ;
#26903 = CARTESIAN_POINT ( 'NONE',  ( -0.2399999999999999079, -3.156018320128275878, -0.4841849112664152743 ) ) ;
#26904 = FACE_BOUND ( 'NONE', #14520, .T. ) ;
#26905 = CARTESIAN_POINT ( 'NONE',  ( 0.1186969743450562581, -1.297359616540578076, 0.4321288993546299473 ) ) ;
#26906 = CARTESIAN_POINT ( 'NONE',  ( 0.3122857990831161556, -1.766572940467653785, 0.5980579735034173838 ) ) ;
#26907 = CARTESIAN_POINT ( 'NONE',  ( 0.5857434439472278820, -1.570035424762864285, -0.5212337988449284865 ) ) ;
#26908 = CARTESIAN_POINT ( 'NONE',  ( -0.02000000000000000042, -2.266124458208340187, -0.5531721439363799231 ) ) ;
#26909 = EDGE_CURVE ( 'NONE', #9760, #4182, #21644, .T. ) ;
#26910 = CARTESIAN_POINT ( 'NONE',  ( -0.02000000000000000042, -2.297142231534299306, -0.5217974784625020179 ) ) ;
#26911 = DIRECTION ( 'NONE',  ( -0.4999551463232372317, 0.8660512985181134660, -0.000000000000000000 ) ) ;
#26912 = ORIENTED_EDGE ( 'NONE', *, *, #661, .F. ) ;
#26913 = CARTESIAN_POINT ( 'NONE',  ( 0.1499999999999996614, -0.09319974324248556097, 0.5318964258758792640 ) ) ;
#26914 =( BOUNDED_SURFACE ( )  B_SPLINE_SURFACE ( 3, 2, ( 
 ( #33370, #14249, #26811 ),
 ( #5174, #7853, #17726 ),
 ( #8276, #8063, #23933 ),
 ( #36463, #39150, #33174 ),
 ( #1918, #17548, #4559 ),
 ( #30276, #14435, #17932 ),
 ( #29894, #4764, #29678 ),
 ( #36052, #39948, #1736 ) ),
 .UNSPECIFIED., .F., .F., .T. ) 
 B_SPLINE_SURFACE_WITH_KNOTS ( ( 4, 2, 2, 4 ),
 ( 3, 3 ),
 ( 0.003138011302842199680, 0.004009802660711201706, 0.004445698339645702719, 0.004881594018580203732 ),
 ( 0.000000000000000000, 1.000000000000000000 ),
 .UNSPECIFIED. ) 
 GEOMETRIC_REPRESENTATION_ITEM ( )  RATIONAL_B_SPLINE_SURFACE ( (
 ( 1.000000000000000000, 0.5504785946861689983, 1.000000000000000000),
 ( 1.000000000000000000, 0.5522673118645705648, 1.000000000000000000),
 ( 1.000000000000000000, 0.5426696336924615727, 1.000000000000000000),
 ( 1.000000000000000000, 0.5149554968636153029, 1.000000000000000000),
 ( 1.000000000000000000, 0.5037106103022731540, 1.000000000000000000),
 ( 1.000000000000000000, 0.4776838670538872678, 1.000000000000000000),
 ( 1.000000000000000000, 0.4627352203515152085, 1.000000000000000000),
 ( 1.000000000000000000, 0.4461867090254074131, 1.000000000000000000) ) ) 
 REPRESENTATION_ITEM ( '' )  SURFACE ( )  );
#26915 = CARTESIAN_POINT ( 'NONE',  ( 0.2318589737339854795, -1.232498520698479982, 0.5197417262808780025 ) ) ;
#26916 = CARTESIAN_POINT ( 'NONE',  ( 0.08989780363036058153, -0.5646359461869331353, 0.1460065308160271857 ) ) ;
#26917 = CARTESIAN_POINT ( 'NONE',  ( -0.05083665881509066842, 0.2375940621857685897, -0.4096919151850460517 ) ) ;
#26918 = CARTESIAN_POINT ( 'NONE',  ( 0.4892141979174440825, -1.277531844236459158, 0.7175028335045045003 ) ) ;
#26920 = ORIENTED_EDGE ( 'NONE', *, *, #19843, .T. ) ;
#26919 = CARTESIAN_POINT ( 'NONE',  ( -0.1612862774928046916, 0.5009394326984771828, 0.1071084547150100430 ) ) ;
#26921 = CARTESIAN_POINT ( 'NONE',  ( 0.4714567382560805875, -1.076664716445512093, 0.6912835816774075548 ) ) ;
#26922 = DIRECTION ( 'NONE',  ( 0.8660512985181133550, 0.4999551463232372317, 0.000000000000000000 ) ) ;
#26923 = ORIENTED_EDGE ( 'NONE', *, *, #22800, .F. ) ;
#26924 = CARTESIAN_POINT ( 'NONE',  ( 0.1999999999999789724, -2.183180860297921466, -0.4937760292030871079 ) ) ;
#26925 = CARTESIAN_POINT ( 'NONE',  ( 0.3271419406413549891, -1.639226515742882917, 0.5756636260908921665 ) ) ;
#26927 = CARTESIAN_POINT ( 'NONE',  ( 0.1871805636416381813, -0.5848937521155493924, 0.01295504015953219575 ) ) ;
#26926 = CARTESIAN_POINT ( 'NONE',  ( 0.6773337002013100072, -1.513729376107809221, 0.4441964172979790404 ) ) ;
#26928 = CARTESIAN_POINT ( 'NONE',  ( 0.4970273525888077026, -1.079783658718535877, 0.3157417262808778213 ) ) ;
#26929 = DIRECTION ( 'NONE',  ( 1.000000000000000000, 1.446659165673942287E-15, -8.266623803851098360E-16 ) ) ;
#26930 = EDGE_LOOP ( 'NONE', ( #37023, #17889, #12821, #34134 ) ) ;
#26931 = ORIENTED_EDGE ( 'NONE', *, *, #28089, .F. ) ;
#26932 = CARTESIAN_POINT ( 'NONE',  ( 0.01034223579727351801, -1.726934810087732641, -0.6381276386021752511 ) ) ;
#26933 = DIRECTION ( 'NONE',  ( 0.4999551463232373427, -0.8660512985181134660, 0.000000000000000000 ) ) ;
#26934 = CARTESIAN_POINT ( 'NONE',  ( 0.07907905168990768396, -0.8327024128097890721, 0.1457185332388749033 ) ) ;
#26935 = DIRECTION ( 'NONE',  ( 0.000000000000000000, 0.000000000000000000, -1.000000000000000000 ) ) ;
#26936 = ADVANCED_FACE ( 'NONE', ( #21783 ), #11898, .F. ) ;
#26937 = CARTESIAN_POINT ( 'NONE',  ( 0.04582897286455926006, 0.06484386734940718322, -0.4825967645925798299 ) ) ;
#26938 = B_SPLINE_CURVE_WITH_KNOTS ( 'NONE', 3,
 ( #4785, #26642, #17360, #17568, #30305, #20256, #1942, #29916, #14667, #39172, #23956, #39363, #5198, #24163, #33392, #1758, #39550, #14270, #20871, #7872 ),
 .UNSPECIFIED., .F., .F.,
 ( 4, 2, 2, 2, 2, 2, 2, 2, 2, 4 ),
 ( 0.000000000000000000, 0.0006013140366011756862, 0.001202628073202351372, 0.001803942109803526950, 0.002104599128104107150, 0.002405256146404686698, 0.003006570183005846664, 0.003607884219607006195, 0.004209198256208165727, 0.004810512292809325692 ),
 .UNSPECIFIED. ) ;
#26939 = CARTESIAN_POINT ( 'NONE',  ( 0.1650048525095897667, -0.9588139417348214844, 0.4627461750576811750 ) ) ;
#26940 = CARTESIAN_POINT ( 'NONE',  ( 0.6672603290686145439, -1.495344574087576150, 0.4226843776606147851 ) ) ;
#26941 = CARTESIAN_POINT ( 'NONE',  ( 0.03309060444528770517, 0.2303206394829958592, -0.4671006372792953498 ) ) ;
#26942 = CARTESIAN_POINT ( 'NONE',  ( -0.1399999999999997358, 0.000000000000000000, 0.000000000000000000 ) ) ;
#26943 = CARTESIAN_POINT ( 'NONE',  ( -0.2399999999999999079, -3.941790907013290823, -0.4709369376873030477 ) ) ;
#26944 = PERSON_AND_ORGANIZATION_ROLE ( 'classification_officer' ) ;
#26945 = CARTESIAN_POINT ( 'NONE',  ( 0.04703387973542435402, -1.223263004737442428, 0.6745384190568795013 ) ) ;
#26946 = CARTESIAN_POINT ( 'NONE',  ( 0.4959366141775247150, -1.219826185980712241, 0.6057417262809806635 ) ) ;
#26947 = CYLINDRICAL_SURFACE ( 'NONE', #18585, 0.01000000000000005398 ) ;
#26948 = CARTESIAN_POINT ( 'NONE',  ( 2.556504791813307099E-05, -0.4639112435509614718, 0.01040637860906285135 ) ) ;
#26949 = CARTESIAN_POINT ( 'NONE',  ( 2.915087563824520450E-32, -4.527947890665461248E-17, -0.2149999999999999967 ) ) ;
#26950 = CARTESIAN_POINT ( 'NONE',  ( 0.001543112456845291544, -0.4709528296724027063, 0.2942976250601397337 ) ) ;
#26951 = AXIS2_PLACEMENT_3D ( 'NONE', #7401, #3310, #29235 ) ;
#26952 = CARTESIAN_POINT ( 'NONE',  ( 0.03868649100028153515, 0.03360400204099701221, -0.4753701585314239475 ) ) ;
#26953 = ORIENTED_EDGE ( 'NONE', *, *, #11779, .F. ) ;
#26954 = VERTEX_POINT ( 'NONE', #21999 ) ;
#26955 = CIRCLE ( 'NONE', #7968, 0.2200000000000000566 ) ;
#26956 = DIRECTION ( 'NONE',  ( 1.000000000000000000, -2.532387540469236772E-12, -8.550494110633229256E-14 ) ) ;
#26957 = ORIENTED_EDGE ( 'NONE', *, *, #12927, .F. ) ;
#26958 = CARTESIAN_POINT ( 'NONE',  ( 0.4114050106974946330, -1.724440955265992947, -0.5872665585884049300 ) ) ;
#26959 = CARTESIAN_POINT ( 'NONE',  ( -0.1053653701217514282, -0.4790241930300290774, 0.1089215720160774531 ) ) ;
#26961 = ORIENTED_EDGE ( 'NONE', *, *, #29775, .F. ) ;
#26960 = CARTESIAN_POINT ( 'NONE',  ( 0.0001947388906042439084, -0.6652226476256291043, -0.02097404292247649973 ) ) ;
#26962 = ORIENTED_EDGE ( 'NONE', *, *, #10652, .F. ) ;
#26963 = CARTESIAN_POINT ( 'NONE',  ( 0.1272900688827675320, -0.5203071491166968432, 0.3917611924818291680 ) ) ;
#26964 = ORIENTED_EDGE ( 'NONE', *, *, #20087, .F. ) ;
#26965 = CARTESIAN_POINT ( 'NONE',  ( 0.2710593583788064032, -1.672243337529662810, 0.6600209757948071188 ) ) ;
#26967 = CARTESIAN_POINT ( 'NONE',  ( 0.1683750554522408238, -1.244696949452464452, 0.6168817076097603547 ) ) ;
#26966 = CARTESIAN_POINT ( 'NONE',  ( -0.02235124290213020420, -0.5044963136724034403, -0.09030809412322339524 ) ) ;
#26968 = CYLINDRICAL_SURFACE ( 'NONE', #368, 0.03749999999977545601 ) ;
#26969 = APPROVAL_ROLE ( '' ) ;
#26970 = CARTESIAN_POINT ( 'NONE',  ( 0.2034277765170372787, -1.278716433895728422, -0.7137157339815681789 ) ) ;
#26972 = ORIENTED_EDGE ( 'NONE', *, *, #35143, .T. ) ;
#26971 = VERTEX_POINT ( 'NONE', #34523 ) ;
#26973 = CARTESIAN_POINT ( 'NONE',  ( 0.01155593465058764660, -0.8452630998613906987, -0.06009144441515529289 ) ) ;
#26974 = CARTESIAN_POINT ( 'NONE',  ( 0.05026878653071940178, -1.025413872748235145, 0.7120682109587219699 ) ) ;
#26975 = CARTESIAN_POINT ( 'NONE',  ( 0.09061274716232860238, -0.5518344063121839449, 0.2019960243542438250 ) ) ;
#26976 = CARTESIAN_POINT ( 'NONE',  ( 0.1874086131461644433, -0.6929147893325138252, 0.03706785969987234919 ) ) ;
#26977 = CARTESIAN_POINT ( 'NONE',  ( 0.4742224691869081354, -1.671175273632494074, 0.5656171320065535024 ) ) ;
#26978 = CARTESIAN_POINT ( 'NONE',  ( 0.06485795133942112711, -1.341245217906781528, 0.5684376680647764690 ) ) ;
#26979 = AXIS2_PLACEMENT_3D ( 'NONE', #22936, #4573, #35267 ) ;
#26980 = CARTESIAN_POINT ( 'NONE',  ( -0.1710642718812832863, 0.4986889572247755198, 0.3032895567580813356 ) ) ;
#26981 = CARTESIAN_POINT ( 'NONE',  ( 0.4567198261210261845, -1.219045092035883293, 0.5856983068965102568 ) ) ;
#26982 = EDGE_CURVE ( 'NONE', #34243, #12973, #32305, .T. ) ;
#26983 = EDGE_CURVE ( 'NONE', #4836, #36854, #24461, .T. ) ;
#26984 = CARTESIAN_POINT ( 'NONE',  ( 0.000000000000000000, -0.03575622569115821658, -0.2978615321325044363 ) ) ;
#26985 = EDGE_CURVE ( 'NONE', #31373, #24117, #37804, .T. ) ;
#26986 = DIRECTION ( 'NONE',  ( 0.2828184691484095792, -0.9591734532964046878, 6.102565427610453878E-13 ) ) ;
#26987 = CONICAL_SURFACE ( 'NONE', #16473, 0.1346589359789736318, 1.047197551196598742 ) ;
#26988 = FACE_OUTER_BOUND ( 'NONE', #17893, .T. ) ;
#26989 = CARTESIAN_POINT ( 'NONE',  ( 0.01131419357477797018, -0.9464773851093645218, 0.1333178999391497199 ) ) ;
#26990 = CARTESIAN_POINT ( 'NONE',  ( 0.3499942944112305887, -1.632920710989241408, -0.3738306617559248868 ) ) ;
#26991 = LENGTH_MEASURE_WITH_UNIT ( LENGTH_MEASURE( 0.02539999999999999897 ), #34167 );
#26993 = EDGE_CURVE ( 'NONE', #25669, #32917, #37209, .T. ) ;
#26992 = VECTOR ( 'NONE', #30819, 39.37007874015748854 ) ;
#26994 = CARTESIAN_POINT ( 'NONE',  ( 0.6099423129193194404, -1.615565191381619137, -0.5028438385245220799 ) ) ;
#26995 = EDGE_CURVE ( 'NONE', #5485, #13785, #11294, .T. ) ;
#26996 = CARTESIAN_POINT ( 'NONE',  ( 0.004299088327612451445, -0.5973376383060815531, 0.3026940496400818970 ) ) ;
#26997 = CARTESIAN_POINT ( 'NONE',  ( 0.1863616350354748430, -0.8703638341540448353, 0.1952903930469164218 ) ) ;
#26998 = PERSON_AND_ORGANIZATION ( #28500, #32463 ) ;
#26999 = CARTESIAN_POINT ( 'NONE',  ( 0.3900547927747317067, -0.9231895138380423749, 0.8021268779562266138 ) ) ;
#27000 = VERTEX_POINT ( 'NONE', #21171 ) ;
#27001 = CARTESIAN_POINT ( 'NONE',  ( -0.3000000000000000999, -2.183180860297908144, -0.4937760292030871079 ) ) ;
#27002 = CARTESIAN_POINT ( 'NONE',  ( 0.01896931156525321488, 0.07379981600434322442, -0.5147676832640546429 ) ) ;
#27003 = ADVANCED_FACE ( 'NONE', ( #5730 ), #18258, .T. ) ;
#27004 = EDGE_LOOP ( 'NONE', ( #29131, #14818, #11942, #30145, #35974, #23367, #26016, #25524, #26762, #4842, #8066, #12233, #12303 ) ) ;
#27005 = DIRECTION ( 'NONE',  ( 0.8660512985181135770, 0.4999551463232370652, -9.916483284928376127E-15 ) ) ;
#27006 = APPLIED_PERSON_AND_ORGANIZATION_ASSIGNMENT ( #30325, #35530, ( #10846 ) ) ;
#27007 = CARTESIAN_POINT ( 'NONE',  ( 0.02616834738919181572, -0.7253350560476993225, 0.5960850904724321886 ) ) ;
#27008 = VECTOR ( 'NONE', #24664, 39.37007874015748854 ) ;
#27009 = CARTESIAN_POINT ( 'NONE',  ( 0.3771340144105596592, -1.765187147855314498, -0.4446665289696524748 ) ) ;
#27011 = ORIENTED_EDGE ( 'NONE', *, *, #32300, .T. ) ;
#27010 = CARTESIAN_POINT ( 'NONE',  ( 0.3934443868333699634, -1.753172285594142066, -0.5285261949624394662 ) ) ;
#27012 = CARTESIAN_POINT ( 'NONE',  ( 0.06356324272688286536, -1.339002332173930832, 0.5682722211006857593 ) ) ;
#27013 = CARTESIAN_POINT ( 'NONE',  ( 0.5468032192656866464, -1.183383020191767443, 0.7376474321803302425 ) ) ;
#27015 = ORIENTED_EDGE ( 'NONE', *, *, #24487, .T. ) ;
#27014 = ORIENTED_EDGE ( 'NONE', *, *, #21404, .F. ) ;
#27016 = CARTESIAN_POINT ( 'NONE',  ( 0.1177554796393661674, -1.375324152023213564, -0.7018171977754862345 ) ) ;
#27017 = CIRCLE ( 'NONE', #101, 0.06000000000000045575 ) ;
#27018 = ORIENTED_EDGE ( 'NONE', *, *, #15483, .F. ) ;
#27019 = VECTOR ( 'NONE', #23936, 39.37007874015748143 ) ;
#27020 = CARTESIAN_POINT ( 'NONE',  ( 3.466477128667603047, -1.051097370103299733, 0.4182417262808778013 ) ) ;
#27021 = DATE_AND_TIME ( #14453, #31314 ) ;
#27022 = CIRCLE ( 'NONE', #18498, 0.03000000000000029379 ) ;
#27023 = CARTESIAN_POINT ( 'NONE',  ( -0.05464101615137762630, -2.032088213807425880, -0.4352898549974345555 ) ) ;
#27024 = ORIENTED_EDGE ( 'NONE', *, *, #12176, .F. ) ;
#27025 = LINE ( 'NONE', #8299, #33706 ) ;
#27026 = CARTESIAN_POINT ( 'NONE',  ( 0.1763646209231259920, -0.8431947878026431198, 0.5885539986222864117 ) ) ;
#27027 = CARTESIAN_POINT ( 'NONE',  ( 0.2556018531037459462, -1.498891464106183014, 1.002349236551413281 ) ) ;
#27028 = CARTESIAN_POINT ( 'NONE',  ( 0.1828482083265061120, -0.8368919259864775473, 0.6643785663031293032 ) ) ;
#27030 = DIRECTION ( 'NONE',  ( -1.416619696839557091E-11, -0.5877852522924708056, 0.8090169943749491166 ) ) ;
#27029 = CARTESIAN_POINT ( 'NONE',  ( 0.1142161186253681515, -0.5282243346103802084, -0.03585910532386479832 ) ) ;
#27031 = CARTESIAN_POINT ( 'NONE',  ( 0.01562499999999997224, -0.9454337353465638305, 0.1626451679851157184 ) ) ;
#27032 = ORIENTED_EDGE ( 'NONE', *, *, #35885, .F. ) ;
#27033 = ORIENTED_EDGE ( 'NONE', *, *, #28027, .T. ) ;
#27034 = CARTESIAN_POINT ( 'NONE',  ( 0.03309060444528726802, -0.5154120966056443542, -0.07470591001490078931 ) ) ;
#27035 = CARTESIAN_POINT ( 'NONE',  ( 0.5937943159907096424, -1.263846424195741891, 0.8742795452994258643 ) ) ;
#27036 = FACE_OUTER_BOUND ( 'NONE', #31827, .T. ) ;
#27037 = EDGE_CURVE ( 'NONE', #40008, #528, #38615, .T. ) ;
#27038 = CARTESIAN_POINT ( 'NONE',  ( 0.3699999999999786793, -2.080216821995567233, -0.4859795201926049302 ) ) ;
#27039 = CARTESIAN_POINT ( 'NONE',  ( -0.04945776359515825088, -0.4418538386403662033, -0.1805520672786481706 ) ) ;
#27040 = EDGE_CURVE ( 'NONE', #31364, #23204, #13287, .T. ) ;
#27041 = AXIS2_PLACEMENT_3D ( 'NONE', #33532, #11338, #36223 ) ;
#27042 = DIRECTION ( 'NONE',  ( 2.280301054154496446E-31, -1.000000000000000000, 4.555315873022819131E-16 ) ) ;
#27043 = CARTESIAN_POINT ( 'NONE',  ( 0.1790649681787556680, -1.895405488977804254, -0.6873613951464528915 ) ) ;
#27044 = EDGE_CURVE ( 'NONE', #11702, #16451, #10854, .T. ) ;
#27045 = CARTESIAN_POINT ( 'NONE',  ( 0.02953079040095673430, -0.2329676531120430660, 0.4763574306556350169 ) ) ;
#27046 = CARTESIAN_POINT ( 'NONE',  ( 0.5155751834530871713, -1.137973747986757544, 0.7479765829993398896 ) ) ;
#27047 = AXIS2_PLACEMENT_3D ( 'NONE', #29349, #1977, #1191 ) ;
#27048 = CARTESIAN_POINT ( 'NONE',  ( -1.019575837292303166, -0.04310840302197994911, 0.09999999999999879818 ) ) ;
#27049 = AXIS2_PLACEMENT_3D ( 'NONE', #15581, #34690, #37369 ) ;
#27050 = CARTESIAN_POINT ( 'NONE',  ( 0.02872242845529806091, 0.5252126300208209697, -0.08844866507292881153 ) ) ;
#27051 = CARTESIAN_POINT ( 'NONE',  ( -0.2399999999999999079, -2.477126460671948749, -0.4732852368073287574 ) ) ;
#27052 = EDGE_LOOP ( 'NONE', ( #19980, #36380, #30167, #954, #33329, #33072, #6694, #36414 ) ) ;
#27053 = DIRECTION ( 'NONE',  ( -1.000000000000000000, -7.857794173099924470E-32, -8.628166150854818811E-32 ) ) ;
#27054 = CARTESIAN_POINT ( 'NONE',  ( -0.05083674528492013178, -0.04859289555129394506, -0.4711018118971389557 ) ) ;
#27055 = CARTESIAN_POINT ( 'NONE',  ( 0.6068013899440870551, -1.480012627510800760, 0.5642015433052736118 ) ) ;
#27056 = ADVANCED_FACE ( 'NONE', ( #3454 ), #7322, .F. ) ;
#27057 = ORIENTED_EDGE ( 'NONE', *, *, #8109, .F. ) ;
#27058 = CYLINDRICAL_SURFACE ( 'NONE', #13479, 0.05000000000000000971 ) ;
#27059 = DIRECTION ( 'NONE',  ( -0.4999551463232372317, 0.8660512985181135770, -0.000000000000000000 ) ) ;
#27060 = CARTESIAN_POINT ( 'NONE',  ( 0.1130491610541830005, -1.062706497792865523, 0.7372862091105505389 ) ) ;
#27061 = ORIENTED_EDGE ( 'NONE', *, *, #21244, .F. ) ;
#27062 = CARTESIAN_POINT ( 'NONE',  ( -0.02869712619511932336, 0.3396447909410118537, 0.3648221446286663006 ) ) ;
#27063 = CARTESIAN_POINT ( 'NONE',  ( 0.04760578872587347549, 0.04300259564631410403, 0.4803138972567881360 ) ) ;
#27064 = CARTESIAN_POINT ( 'NONE',  ( 0.03170874437002394602, -0.4816890803163380586, -0.09938493968693067060 ) ) ;
#27065 = DIRECTION ( 'NONE',  ( -1.188678714063530652E-15, 1.000000000000000000, 0.000000000000000000 ) ) ;
#27066 = CARTESIAN_POINT ( 'NONE',  ( 0.4688806894441774897, -1.239828276217276759, 0.5901340395503891223 ) ) ;
#27067 = VECTOR ( 'NONE', #20779, 39.37007874015748143 ) ;
#27068 = CARTESIAN_POINT ( 'NONE',  ( 0.05999999999999990757, -0.1354409211049039941, -0.1857769145426272639 ) ) ;
#27069 = CARTESIAN_POINT ( 'NONE',  ( 0.4030327056921976792, -1.680968334469209680, -0.4031266960524464982 ) ) ;
#27070 = ORIENTED_EDGE ( 'NONE', *, *, #14278, .F. ) ;
#27071 = ORIENTED_EDGE ( 'NONE', *, *, #12000, .T. ) ;
#27072 = CYLINDRICAL_SURFACE ( 'NONE', #32957, 0.1999999999999994837 ) ;
#27073 = ORIENTED_EDGE ( 'NONE', *, *, #30129, .T. ) ;
#27074 = AXIS2_PLACEMENT_3D ( 'NONE', #14365, #21718, #26929 ) ;
#27075 = LINE ( 'NONE', #20500, #37104 ) ;
#27076 = CIRCLE ( 'NONE', #18527, 0.5399999999999999245 ) ;
#27077 = CARTESIAN_POINT ( 'NONE',  ( 0.2634339134604823940, -1.167471577589091369, 0.8605345870829919086 ) ) ;
#27079 = DIRECTION ( 'NONE',  ( 2.465190328815661892E-32, 1.000000000000000000, 6.656013887802287108E-31 ) ) ;
#27078 = CARTESIAN_POINT ( 'NONE',  ( 0.6926523052361154287, -1.550981559465477666, 0.5932697689988618572 ) ) ;
#27080 = CARTESIAN_POINT ( 'NONE',  ( 0.5006733635628357604, -1.193711096620792889, 0.4198196556967657145 ) ) ;
#27081 = EDGE_LOOP ( 'NONE', ( #14388, #20145, #21699 ) ) ;
#27082 = AXIS2_PLACEMENT_3D ( 'NONE', #20044, #23136, #35662 ) ;
#27083 = DIRECTION ( 'NONE',  ( -0.4999999999999972244, 0.02174101728960634375, 0.8657524635640466704 ) ) ;
#27084 = CARTESIAN_POINT ( 'NONE',  ( 0.1684271861732587194, -0.7249060024178762829, 0.5310654164351663598 ) ) ;
#27085 = ORIENTED_EDGE ( 'NONE', *, *, #11163, .F. ) ;
#27086 = DIRECTION ( 'NONE',  ( -1.000000000000000000, -2.280301054154495132E-31, 1.664003471950577689E-31 ) ) ;
#27087 = CARTESIAN_POINT ( 'NONE',  ( 0.05201840200954328114, -0.4415345355162912377, 0.1624690192511292486 ) ) ;
#27088 = EDGE_CURVE ( 'NONE', #14602, #15639, #36923, .T. ) ;
#27089 = CARTESIAN_POINT ( 'NONE',  ( 0.6295207449309501158, -1.563610153985103945, 0.4182417262808776903 ) ) ;
#27090 = CARTESIAN_POINT ( 'NONE',  ( 0.1413813297004133662, -1.285503893349357663, 0.4210986513813943510 ) ) ;
#27091 = ADVANCED_FACE ( 'NONE', ( #621 ), #15257, .T. ) ;
#27092 = CARTESIAN_POINT ( 'NONE',  ( 0.3945466357887226772, -1.754957878890512024, -0.4915690588065673161 ) ) ;
#27093 = CARTESIAN_POINT ( 'NONE',  ( 0.3857519400669835452, -1.760804991660537722, -0.4635226585062726667 ) ) ;
#27094 = B_SPLINE_CURVE_WITH_KNOTS ( 'NONE', 3,
 ( #21464, #11584, #36667, #15065 ),
 .UNSPECIFIED., .F., .F.,
 ( 4, 4 ),
 ( 0.8392141848601618603, 0.9812523608469967407 ),
 .UNSPECIFIED. ) ;
#27095 = CARTESIAN_POINT ( 'NONE',  ( 0.2622253439111549289, -0.6837502657356347990, 0.6133988000875116864 ) ) ;
#27096 = CARTESIAN_POINT ( 'NONE',  ( -0.05464101615137773038, -2.585754275622221154, -0.2040099479399058446 ) ) ;
#27097 = CARTESIAN_POINT ( 'NONE',  ( -0.1655857493438386840, 0.4810233835288760806, 0.3340284351899800441 ) ) ;
#27098 = B_SPLINE_CURVE_WITH_KNOTS ( 'NONE', 3,
 ( #833, #26123, #35359, #3687, #38634, #7346, #28373 ),
 .UNSPECIFIED., .F., .F.,
 ( 4, 3, 4 ),
 ( -6.000000000402129679E-08, 0.000000000000000000, 0.0003133564821238285308 ),
 .UNSPECIFIED. ) ;
#27099 = TOROIDAL_SURFACE ( 'NONE', #29729, 0.5250000000000000222, 0.01499999999999999944 ) ;
#27100 = CARTESIAN_POINT ( 'NONE',  ( 0.6042279486826958035, -1.591103445072521438, -0.5492199064561998911 ) ) ;
#27101 = CARTESIAN_POINT ( 'NONE',  ( 0.02992969784436203332, -1.949504067775972294, -0.6897318246428794097 ) ) ;
#27102 = CARTESIAN_POINT ( 'NONE',  ( 0.6565669552028456923, -1.566507581639152935, 0.6100543721193861790 ) ) ;
#27103 = CARTESIAN_POINT ( 'NONE',  ( 0.3720469278356866027, -1.757009016027275550, -0.4316954512420498880 ) ) ;
#27104 = CARTESIAN_POINT ( 'NONE',  ( -0.02953079040095700838, 0.2329676531120452587, -0.4763574306556336291 ) ) ;
#27105 = CIRCLE ( 'NONE', #22508, 0.03000000000000001971 ) ;
#27106 = EDGE_CURVE ( 'NONE', #8287, #16786, #183, .T. ) ;
#27107 = CARTESIAN_POINT ( 'NONE',  ( 0.002083146443013488870, -0.4777046557262296100, 0.1283381445693447254 ) ) ;
#27108 = CARTESIAN_POINT ( 'NONE',  ( 0.5717479371661525755, -1.545029730964961434, -0.5259570771718768967 ) ) ;
#27109 = ADVANCED_FACE ( 'NONE', ( #25677 ), #35137, .F. ) ;
#27110 = AXIS2_PLACEMENT_3D ( 'NONE', #25367, #31932, #18977 ) ;
#27111 = CYLINDRICAL_SURFACE ( 'NONE', #23247, 2.001674066779348227 ) ;
#27112 = DIRECTION ( 'NONE',  ( -0.4999551463232347892, 0.8660512985181149093, 0.000000000000000000 ) ) ;
#27113 = EDGE_CURVE ( 'NONE', #17309, #35061, #31639, .T. ) ;
#27115 = ORIENTED_EDGE ( 'NONE', *, *, #11494, .F. ) ;
#27114 = PRODUCT ( 'Lower cage plate', 'Lower cage plate', '', ( #33499 ) ) ;
#27116 = DIRECTION ( 'NONE',  ( 1.000000000000000000, 0.000000000000000000, 0.000000000000000000 ) ) ;
#27117 = CIRCLE ( 'NONE', #25836, 0.08000000000000002942 ) ;
#27118 = ORIENTED_EDGE ( 'NONE', *, *, #38128, .F. ) ;
#27119 = CARTESIAN_POINT ( 'NONE',  ( 0.3386245021663031318, -1.171855970582244222, 0.5796378340604717572 ) ) ;
#27120 = CARTESIAN_POINT ( 'NONE',  ( 0.1915761776375039804, -1.276944146096590016, 0.5182417262812423209 ) ) ;
#27121 = CARTESIAN_POINT ( 'NONE',  ( -0.03654364704248847656, 0.2290829176602892370, -0.4574690890339254135 ) ) ;
#27122 = CARTESIAN_POINT ( 'NONE',  ( 0.5048881121617861956, -1.301036302150182289, 0.6753596003262275493 ) ) ;
#27124 = ORIENTED_EDGE ( 'NONE', *, *, #14559, .F. ) ;
#27123 = CARTESIAN_POINT ( 'NONE',  ( -0.1593650814506384072, 0.4947962564849512357, 0.1029884207726596002 ) ) ;
#27125 = CARTESIAN_POINT ( 'NONE',  ( 0.3382833150183324755, -0.9396054708716727877, 0.6333258291577809063 ) ) ;
#27126 = ORIENTED_EDGE ( 'NONE', *, *, #30843, .T. ) ;
#27127 = CARTESIAN_POINT ( 'NONE',  ( 0.02299189108461704989, -1.617841354202916859, -0.3728701932220275794 ) ) ;
#27128 = VERTEX_POINT ( 'NONE', #7126 ) ;
#27129 = CARTESIAN_POINT ( 'NONE',  ( 0.3330041777007136661, -1.680901281163226457, -0.6241177864389138019 ) ) ;
#27130 = VERTEX_POINT ( 'NONE', #31849 ) ;
#27131 = CARTESIAN_POINT ( 'NONE',  ( 0.3573112754633941401, -1.622562401408601085, 0.5912586822741335846 ) ) ;
#27133 = CARTESIAN_POINT ( 'NONE',  ( 0.1139707206188099453, -0.5585964955268626353, -0.05809159769505588267 ) ) ;
#27132 = CARTESIAN_POINT ( 'NONE',  ( 0.7000186069066542949, -1.492953544047383563, 0.4955563437734074594 ) ) ;
#27134 = CYLINDRICAL_SURFACE ( 'NONE', #24734, 0.03000000000000022787 ) ;
#27135 = VECTOR ( 'NONE', #15193, 39.37007874015748143 ) ;
#27136 = B_SPLINE_CURVE_WITH_KNOTS ( 'NONE', 3,
 ( #16971, #13861, #29515, #7703 ),
 .UNSPECIFIED., .F., .F.,
 ( 4, 4 ),
 ( 0.02020468389890235292, 0.1625918618111195091 ),
 .UNSPECIFIED. ) ;
#27137 = ORIENTED_EDGE ( 'NONE', *, *, #37717, .T. ) ;
#27138 = VERTEX_POINT ( 'NONE', #3664 ) ;
#27139 = CARTESIAN_POINT ( 'NONE',  ( 0.1828088565713123503, -1.273079348061378235, 0.4182417262808778013 ) ) ;
#27140 = CARTESIAN_POINT ( 'NONE',  ( -0.05464101615137786222, -2.122347498858831116, -0.8313396097929491857 ) ) ;
#27141 = AXIS2_PLACEMENT_3D ( 'NONE', #35742, #23005, #38813 ) ;
#27142 = CIRCLE ( 'NONE', #29092, 0.01499999999999999424 ) ;
#27143 = CARTESIAN_POINT ( 'NONE',  ( 0.1316173717439282076, -0.9114899509784721854, 0.5960367549459311132 ) ) ;
#27144 = CARTESIAN_POINT ( 'NONE',  ( 0.1424771846812046827, -1.296107695835423401, -0.3417999629372251436 ) ) ;
#27145 = CIRCLE ( 'NONE', #21147, 0.06000000000000038636 ) ;
#27146 = EDGE_CURVE ( 'NONE', #5206, #18566, #28762, .T. ) ;
#27147 = LINE ( 'NONE', #11296, #14129 ) ;
#27148 = ADVANCED_FACE ( 'NONE', ( #19694 ), #2523, .T. ) ;
#27149 = DIRECTION ( 'NONE',  ( -0.4870160029269081092, 0.8733930460526335704, 0.000000000000000000 ) ) ;
#27150 = CARTESIAN_POINT ( 'NONE',  ( 0.5708401535611469235, -1.615683077095924736, 0.5197417262808792238 ) ) ;
#27151 = CARTESIAN_POINT ( 'NONE',  ( 0.05283710938261031165, 0.4315340639268053224, 0.1819215676045953523 ) ) ;
#27152 = LINE ( 'NONE', #23871, #12194 ) ;
#27153 = FACE_OUTER_BOUND ( 'NONE', #30420, .T. ) ;
#27154 = APPROVAL_DATE_TIME ( #4918, #15957 ) ;
#27155 = CARTESIAN_POINT ( 'NONE',  ( 0.4333926128620538831, -1.140607306138202270, 0.4331035760720922112 ) ) ;
#27156 = CARTESIAN_POINT ( 'NONE',  ( 0.4638926575998975621, -1.238161088593346282, 0.6057417262809813296 ) ) ;
#27157 = APPLICATION_CONTEXT ( 'configuration controlled 3d designs of mechanical parts and assemblies' ) ;
#27158 = FACE_OUTER_BOUND ( 'NONE', #20438, .T. ) ;
#27159 =( BOUNDED_SURFACE ( )  B_SPLINE_SURFACE ( 3, 2, ( 
 ( #13832, #3781, #26018 ),
 ( #7056, #32159, #3968 ),
 ( #17133, #38535, #14045 ),
 ( #38327, #6851, #19431 ),
 ( #939, #35862, #10365 ),
 ( #16335, #22927, #28874 ),
 ( #32567, #7242, #19818 ),
 ( #16940, #29684, #22728 ),
 ( #4383, #7676, #32352 ),
 ( #13236, #25806, #26407 ),
 ( #38937, #16744, #29292 ),
 ( #10159, #7456, #4173 ),
 ( #13639, #26206, #10552 ),
 ( #23127, #35655, #9947 ),
 ( #20034, #10769, #20241 ),
 ( #32761, #4563, #2115 ),
 ( #11368, #14253, #2527 ),
 ( #39954, #33376, #39754 ),
 ( #27218, #36058, #8283 ),
 ( #5594, #17732, #20851 ),
 ( #23541, #11772, #27007 ),
 ( #30706, #4983, #32965 ),
 ( #33562, #30094, #24148 ),
 ( #5179, #14650, #5378 ),
 ( #18152, #39155, #17341 ),
 ( #17552, #20427, #1923 ),
 ( #21039, #36858, #30282 ),
 ( #24332, #36469, #2329 ),
 ( #8068, #33181, #20642 ),
 ( #26626, #11585, #36668 ),
 ( #10981, #21251, #7857 ),
 ( #8673, #30497, #4769 ),
 ( #1742, #23722, #36250 ),
 ( #14440, #29899, #39534 ),
 ( #23937, #26816, #39346 ),
 ( #14869, #8478, #33786 ),
 ( #17941, #27429, #11167 ),
 ( #15266, #86, #37894 ),
 ( #15482, #18774, #9705 ),
 ( #5794, #28036, #12795 ),
 ( #40564, #40146, #30899 ),
 ( #21864, #25358, #22078 ),
 ( #12190, #37072, #25140 ),
 ( #6592, #24750, #2927 ),
 ( #31714, #34180, #9284 ),
 ( #22273, #12383, #34391 ),
 ( #34788, #27617, #2719 ),
 ( #27823, #24938, #40358 ),
 ( #18351, #28423, #6204 ),
 ( #11977, #15672, #24542 ),
 ( #33989, #28219, #37272 ),
 ( #34601, #296, #37466 ),
 ( #9089, #15066, #21655 ),
 ( #31325, #19172, #6403 ),
 ( #5991, #8892, #37681 ),
 ( #21465, #18556, #3132 ),
 ( #31113, #12579, #9499 ),
 ( #18971, #31504, #3313 ),
 ( #15876, #16095, #31923 ),
 ( #3742, #29024, #16295 ),
 ( #34997, #16897, #10326 ),
 ( #38080, #28639, #22683 ),
 ( #22470, #16691, #13185 ),
 ( #29439, #28834, #38496 ),
 ( #7403, #7625, #35217 ),
 ( #1283, #3532, #26356 ),
 ( #1095, #13788, #7017 ),
 ( #9899, #23288, #3923 ),
 ( #29237, #6806, #10111 ),
 ( #13004, #35407, #22887 ) ),
 .UNSPECIFIED., .F., .F., .T. ) 
 B_SPLINE_SURFACE_WITH_KNOTS ( ( 4, 2, 2, 2, 2, 2, 2, 2, 2, 2, 2, 2, 2, 2, 2, 2, 2, 2, 2, 2, 2, 2, 2, 2, 2, 2, 2, 2, 2, 2, 2, 2, 2, 2, 4 ),
 ( 3, 3 ),
 ( 0.006982594028375741814, 0.007169652589743046381, 0.007263181870426699098, 0.007356711151110351815, 0.007730828273844962684, 0.008479062519314182686, 0.009975531010252624425, 0.01147199950119106443, 0.01296846799212950617, 0.01895434195588327139, 0.02045081044682171140, 0.02194727893776015487, 0.02494021591963703488, 0.02793315290151391489, 0.02942962139245235836, 0.03092608988339079837, 0.03391902686526768185, 0.03691196384714456186, 0.03840843233808299839, 0.03990490082902144187, 0.04140136931995988534, 0.04289783781089832881, 0.04364607205636755055, 0.04439430630183677229, 0.04589077479277520882, 0.04663900903824443056, 0.04738724328371364536, 0.04813547752918286710, 0.04888371177465208883, 0.05038018026559053231, 0.05187664875652897578, 0.05337311724746741926, 0.05374723437020202665, 0.05412135149293663405, 0.05486958573840585579 ),
 ( 0.000000000000000000, 1.000000000000000000 ),
 .UNSPECIFIED. ) 
 GEOMETRIC_REPRESENTATION_ITEM ( )  RATIONAL_B_SPLINE_SURFACE ( (
 ( 1.000000000000000000, 0.7687635770067674512, 1.000000000000000000),
 ( 1.000000000000000000, 0.7687635770067674512, 1.000000000000000000),
 ( 1.000000000000000000, 0.7687635770067657859, 1.000000000000000000),
 ( 1.000000000000000000, 0.7687635770067657859, 1.000000000000000000),
 ( 1.000000000000000000, 0.7687635770067644536, 1.000000000000000000),
 ( 1.000000000000000000, 0.7687635770067644536, 1.000000000000000000),
 ( 1.000000000000000000, 0.7687632101434925813, 1.000000000000000000),
 ( 1.000000000000000000, 0.7687598537572957191, 1.000000000000000000),
 ( 1.000000000000000000, 0.7687534107862498134, 1.000000000000000000),
 ( 1.000000000000000000, 0.7687384292891166204, 1.000000000000000000),
 ( 1.000000000000000000, 0.7687365999447838272, 1.000000000000000000),
 ( 1.000000000000000000, 0.7687020167486041666, 1.000000000000000000),
 ( 1.000000000000000000, 0.7686222834918778890, 1.000000000000000000),
 ( 1.000000000000000000, 0.7675492984621066217, 1.000000000000000000),
 ( 1.000000000000000000, 0.7668174832494044635, 1.000000000000000000),
 ( 1.000000000000000000, 0.7652231905048935134, 1.000000000000000000),
 ( 1.000000000000000000, 0.7643808905106918017, 1.000000000000000000),
 ( 1.000000000000000000, 0.7599837323011349177, 1.000000000000000000),
 ( 1.000000000000000000, 0.7555546695031651883, 1.000000000000000000),
 ( 1.000000000000000000, 0.7485199935451233300, 1.000000000000000000),
 ( 1.000000000000000000, 0.7470345500374537817, 1.000000000000000000),
 ( 1.000000000000000000, 0.7439636425267035502, 1.000000000000000000),
 ( 1.000000000000000000, 0.7423870523181574921, 1.000000000000000000),
 ( 1.000000000000000000, 0.7376049540916959080, 1.000000000000000000),
 ( 1.000000000000000000, 0.7343341012102607701, 1.000000000000000000),
 ( 1.000000000000000000, 0.7284347353659686997, 1.000000000000000000),
 ( 1.000000000000000000, 0.7258666192759820612, 1.000000000000000000),
 ( 1.000000000000000000, 0.7233512264919610413, 1.000000000000000000),
 ( 1.000000000000000000, 0.7227328269103746594, 1.000000000000000000),
 ( 1.000000000000000000, 0.7220177958833203791, 1.000000000000000000),
 ( 1.000000000000000000, 0.7219233079132257869, 1.000000000000000000),
 ( 1.000000000000000000, 0.7224401686324471994, 1.000000000000000000),
 ( 1.000000000000000000, 0.7237963925639867568, 1.000000000000000000),
 ( 1.000000000000000000, 0.7277615327345778873, 1.000000000000000000),
 ( 1.000000000000000000, 0.7304068960252722009, 1.000000000000000000),
 ( 1.000000000000000000, 0.7344733377828095433, 1.000000000000000000),
 ( 1.000000000000000000, 0.7358434634388121287, 1.000000000000000000),
 ( 1.000000000000000000, 0.7384753478062177079, 1.000000000000000000),
 ( 1.000000000000000000, 0.7397446418154087766, 1.000000000000000000),
 ( 1.000000000000000000, 0.7420434277178875604, 1.000000000000000000),
 ( 1.000000000000000000, 0.7430738375077751146, 1.000000000000000000),
 ( 1.000000000000000000, 0.7446479001369198381, 1.000000000000000000),
 ( 1.000000000000000000, 0.7451730098702049609, 1.000000000000000000),
 ( 1.000000000000000000, 0.7453954219144471871, 1.000000000000000000),
 ( 1.000000000000000000, 0.7453712964557482890, 1.000000000000000000),
 ( 1.000000000000000000, 0.7450704390704340208, 1.000000000000000000),
 ( 1.000000000000000000, 0.7447959842850340184, 1.000000000000000000),
 ( 1.000000000000000000, 0.7435913020326400114, 1.000000000000000000),
 ( 1.000000000000000000, 0.7422580051630394138, 1.000000000000000000),
 ( 1.000000000000000000, 0.7395387433289906109, 1.000000000000000000),
 ( 1.000000000000000000, 0.7385151462303933823, 1.000000000000000000),
 ( 1.000000000000000000, 0.7363255657919565156, 1.000000000000000000),
 ( 1.000000000000000000, 0.7351593361101353974, 1.000000000000000000),
 ( 1.000000000000000000, 0.7327799655195763595, 1.000000000000000000),
 ( 1.000000000000000000, 0.7315669817046001056, 1.000000000000000000),
 ( 1.000000000000000000, 0.7291668309240953993, 1.000000000000000000),
 ( 1.000000000000000000, 0.7279734049794366335, 1.000000000000000000),
 ( 1.000000000000000000, 0.7245550934509018548, 1.000000000000000000),
 ( 1.000000000000000000, 0.7225262869826848400, 1.000000000000000000),
 ( 1.000000000000000000, 0.7191733065149791271, 1.000000000000000000),
 ( 1.000000000000000000, 0.7178371072958583676, 1.000000000000000000),
 ( 1.000000000000000000, 0.7159520326050418104, 1.000000000000000000),
 ( 1.000000000000000000, 0.7154250687472349934, 1.000000000000000000),
 ( 1.000000000000000000, 0.7152986269598831104, 1.000000000000000000),
 ( 1.000000000000000000, 0.7153184165285554341, 1.000000000000000000),
 ( 1.000000000000000000, 0.7151210821975008125, 1.000000000000000000),
 ( 1.000000000000000000, 0.7151025729118313246, 1.000000000000000000),
 ( 1.000000000000000000, 0.7149568612536305601, 1.000000000000000000),
 ( 1.000000000000000000, 0.7148599564469685363, 1.000000000000000000),
 ( 1.000000000000000000, 0.7147632890095302338, 1.000000000000000000) ) ) 
 REPRESENTATION_ITEM ( '' )  SURFACE ( )  );
#27160 = CARTESIAN_POINT ( 'NONE',  ( 2.612502379249534283E-05, -0.4595599869189778697, 0.01785893867001119018 ) ) ;
#27161 = CARTESIAN_POINT ( 'NONE',  ( 0.3649134372921009062, -1.761483993094715705, -0.5896594712253142578 ) ) ;
#27162 = AXIS2_PLACEMENT_3D ( 'NONE', #29463, #1307, #26383 ) ;
#27163 = CARTESIAN_POINT ( 'NONE',  ( -0.2399999999999999079, -2.511040369707300268, -0.4948468226404901804 ) ) ;
#27164 = CARTESIAN_POINT ( 'NONE',  ( 0.5324045658229008549, -1.654590185004139125, -0.5371941175943450997 ) ) ;
#27165 = EDGE_LOOP ( 'NONE', ( #32569, #14248, #7399, #8487 ) ) ;
#27166 = CIRCLE ( 'NONE', #36994, 0.03000000000000002318 ) ;
#27167 = ORIENTED_EDGE ( 'NONE', *, *, #30268, .F. ) ;
#27168 = AXIS2_PLACEMENT_3D ( 'NONE', #30654, #2475, #17879 ) ;
#27169 = CARTESIAN_POINT ( 'NONE',  ( 0.4166104074968063342, -1.713279937176168888, 0.4265607484113185244 ) ) ;
#27170 = VERTEX_POINT ( 'NONE', #17018 ) ;
#27171 = CARTESIAN_POINT ( 'NONE',  ( 0.4376587549789876519, -1.692075737177143768, -0.4124806547340321705 ) ) ;
#27172 = FACE_OUTER_BOUND ( 'NONE', #30452, .T. ) ;
#27174 = ORIENTED_EDGE ( 'NONE', *, *, #34825, .F. ) ;
#27173 = CARTESIAN_POINT ( 'NONE',  ( 0.0005173413194128835589, -0.6356009618386162519, -0.005393434144287580050 ) ) ;
#27175 = B_SPLINE_CURVE_WITH_KNOTS ( 'NONE', 3,
 ( #34459, #24208, #18412, #8540, #18847, #40628, #36936, #21110, #6060, #27895, #18628, #24817, #27297, #37339, #33638, #5451, #15124, #2192 ),
 .UNSPECIFIED., .F., .F.,
 ( 4, 2, 2, 2, 2, 2, 2, 2, 4 ),
 ( 0.000000000000000000, 0.0007746617437634303492, 0.001549323487526860698, 0.002323985231290290939, 0.003098646975053721397, 0.003873308718817151854, 0.004647970462580581878, 0.005422632206344012336, 0.006197293950107442793 ),
 .UNSPECIFIED. ) ;
#27176 = VECTOR ( 'NONE', #33889, 39.37007874015748143 ) ;
#27177 = ORIENTED_EDGE ( 'NONE', *, *, #39, .T. ) ;
#27178 = FACE_OUTER_BOUND ( 'NONE', #30052, .T. ) ;
#27179 = VERTEX_POINT ( 'NONE', #35733 ) ;
#27180 = CARTESIAN_POINT ( 'NONE',  ( 0.2675213926922588303, -1.675618524670827725, 0.5885039628761479236 ) ) ;
#27182 = CARTESIAN_POINT ( 'NONE',  ( 0.1219191204388515443, -1.265695392162811128, 0.6214586437892982707 ) ) ;
#27181 = CARTESIAN_POINT ( 'NONE',  ( 0.5960624699613672473, -1.598417375062506807, 0.4241902398403092911 ) ) ;
#27183 = CARTESIAN_POINT ( 'NONE',  ( -0.2043922129835741008, -0.5166151207188713901, 0.08499999999999979794 ) ) ;
#27184 = CALENDAR_DATE ( 2026, 13, 10 ) ;
#27185 = CARTESIAN_POINT ( 'NONE',  ( 0.5128645028602584199, -1.648320493942843079, 0.5682417262808785452 ) ) ;
#27187 = ORIENTED_EDGE ( 'NONE', *, *, #37284, .T. ) ;
#27186 = ORIENTED_EDGE ( 'NONE', *, *, #1206, .F. ) ;
#27188 = CARTESIAN_POINT ( 'NONE',  ( 0.01158602179187158757, -0.8240205477835698122, -0.07428298264304349086 ) ) ;
#27189 = CARTESIAN_POINT ( 'NONE',  ( 0.2209956536232957902, -1.227897296991992793, 0.5182417262820130377 ) ) ;
#27190 = CARTESIAN_POINT ( 'NONE',  ( 0.1327909607021672822, -0.7181627890942366976, 0.4916566485045106294 ) ) ;
#27191 = CARTESIAN_POINT ( 'NONE',  ( 0.1873172703549026430, -0.6992301746806637297, 0.03180769156107667722 ) ) ;
#27192 = CARTESIAN_POINT ( 'NONE',  ( 0.4732241761476873032, -1.676040907666597635, 0.5636287125706156420 ) ) ;
#27193 = CARTESIAN_POINT ( 'NONE',  ( 0.05990452446249143470, -1.332664632394616522, 0.5684199413688966196 ) ) ;
#27194 = B_SPLINE_CURVE_WITH_KNOTS ( 'NONE', 3,
 ( #13729, #17228, #5077, #1230, #14144, #38821, #1621, #39245, #39639, #36143, #7955, #29993, #1826, #8167, #20746, #33269, #14541, #11473 ),
 .UNSPECIFIED., .F., .F.,
 ( 4, 2, 2, 2, 2, 2, 2, 2, 4 ),
 ( 0.000000000000000000, 0.0007746617437634300239, 0.001549323487526859614, 0.002323985231290289638, 0.003098646975053719228, 0.003873308718817148819, 0.004647970462580579276, 0.005422632206344009734, 0.006197293950107438457 ),
 .UNSPECIFIED. ) ;
#27195 = AXIS2_PLACEMENT_3D ( 'NONE', #29114, #13278, #10395 ) ;
#27196 = CARTESIAN_POINT ( 'NONE',  ( 0.3857818729960305060, -1.743806986988165386, -0.4496613049301777520 ) ) ;
#27197 = CARTESIAN_POINT ( 'NONE',  ( 0.2160030156770379184, -1.196403219198641565, -0.5155029497116575543 ) ) ;
#27198 = LINE ( 'NONE', #33976, #8234 ) ;
#27199 = CIRCLE ( 'NONE', #39660, 2.001671648589477215 ) ;
#27200 = CARTESIAN_POINT ( 'NONE',  ( 0.1999999999999791112, -2.107936428766273629, -0.2870436526301869407 ) ) ;
#27201 = CARTESIAN_POINT ( 'NONE',  ( 0.6451746001002063302, -1.456551915967818189, 0.4182417262808775238 ) ) ;
#27202 = CIRCLE ( 'NONE', #37052, 0.5302738246768086139 ) ;
#27203 = CARTESIAN_POINT ( 'NONE',  ( 0.4438612498438265774, -1.115686201973224989, 0.5854483341245866335 ) ) ;
#27204 = CARTESIAN_POINT ( 'NONE',  ( 0.3405956938547828883, -1.648484147626967378, -0.3820619200265555904 ) ) ;
#27205 = CARTESIAN_POINT ( 'NONE',  ( 0.6597989824866907771, -1.598367771496736367, -0.5155029497116575543 ) ) ;
#27206 = CARTESIAN_POINT ( 'NONE',  ( 0.1287314663193102893, -1.150224043500909454, 0.9169127589950010204 ) ) ;
#27207 = AXIS2_PLACEMENT_3D ( 'NONE', #13499, #38583, #36102 ) ;
#27208 = CARTESIAN_POINT ( 'NONE',  ( 0.4871018846440973715, -1.079508789421436799, 0.5988988590622403851 ) ) ;
#27209 = CARTESIAN_POINT ( 'NONE',  ( 0.03517919600029659893, -0.9626726882664039531, 0.6501402935033664399 ) ) ;
#27210 = PRODUCT_CONTEXT ( 'NONE', #37659, 'mechanical' ) ;
#27211 = CARTESIAN_POINT ( 'NONE',  ( 0.1893427799090355301, -0.4853919354581605061, 0.2707563002020392240 ) ) ;
#27212 = AXIS2_PLACEMENT_3D ( 'NONE', #28091, #35227, #35415 ) ;
#27213 = CARTESIAN_POINT ( 'NONE',  ( 0.01210505692010060280, 0.06117178301711216626, -0.1249999999999998612 ) ) ;
#27214 = CARTESIAN_POINT ( 'NONE',  ( 0.03672447062657592520, -0.04080285735492294313, -0.4790833464420522492 ) ) ;
#27215 = DIRECTION ( 'NONE',  ( -1.000000000000000000, -0.000000000000000000, -0.000000000000000000 ) ) ;
#27216 = ORIENTED_EDGE ( 'NONE', *, *, #10405, .T. ) ;
#27217 = CARTESIAN_POINT ( 'NONE',  ( 0.000000000000000000, -0.4700000000000001954, 0.000000000000000000 ) ) ;
#27218 = CARTESIAN_POINT ( 'NONE',  ( 0.02214534912214586454, -0.6642453835387356342, 0.4942379723847386552 ) ) ;
#27219 = AXIS2_PLACEMENT_3D ( 'NONE', #19722, #1432, #38642 ) ;
#27220 = CARTESIAN_POINT ( 'NONE',  ( 0.5878316020795693042, -1.491211184378168131, 0.5715274954139647479 ) ) ;
#27221 = CARTESIAN_POINT ( 'NONE',  ( 0.2904739219323096422, -1.661323359162851787, 0.4499284763591545055 ) ) ;
#27223 = ORIENTED_EDGE ( 'NONE', *, *, #19142, .T. ) ;
#27222 = DIRECTION ( 'NONE',  ( 0.01254811300245564816, 0.8659344938869285579, 0.4999999971568664936 ) ) ;
#27224 = CARTESIAN_POINT ( 'NONE',  ( -0.02000000000000000042, -1.910390638264138685, -0.7420407338378623985 ) ) ;
#27225 = CARTESIAN_POINT ( 'NONE',  ( 0.5974340449968663647, -1.261189741147681787, 0.6853727476855657752 ) ) ;
#27227 = EDGE_LOOP ( 'NONE', ( #35860, #32262, #17518, #3928, #15214, #30412, #6043, #21306, #32220 ) ) ;
#27226 = VERTEX_POINT ( 'NONE', #29560 ) ;
#27228 = CARTESIAN_POINT ( 'NONE',  ( 0.1359808222933183708, -1.346136899214501526, -0.7113549742108937757 ) ) ;
#27229 = AXIS2_PLACEMENT_3D ( 'NONE', #13045, #10160, #25597 ) ;
#27230 = ORIENTED_EDGE ( 'NONE', *, *, #23573, .F. ) ;
#27231 = CIRCLE ( 'NONE', #23310, 0.9237847906030155487 ) ;
#27232 = FACE_OUTER_BOUND ( 'NONE', #22932, .T. ) ;
#27233 = APPROVAL_PERSON_ORGANIZATION ( #4511, #3655, #11108 ) ;
#27234 = PRODUCT ( 'Pulley', 'Pulley', '', ( #37497 ) ) ;
#27235 = CYLINDRICAL_SURFACE ( 'NONE', #30498, 0.08000000000000000167 ) ;
#27236 = PERSON_AND_ORGANIZATION_ROLE ( 'classification_officer' ) ;
#27237 = CARTESIAN_POINT ( 'NONE',  ( -0.03647137243075046498, 0.4543612417835873885, -0.2356044583002107895 ) ) ;
#27238 = ORIENTED_EDGE ( 'NONE', *, *, #703, .F. ) ;
#27239 = DIRECTION ( 'NONE',  ( 1.188678714063518227E-15, -1.000000000000000000, -3.263080277421930985E-16 ) ) ;
#27240 = CARTESIAN_POINT ( 'NONE',  ( 0.09432152222331363634, -0.7171591389413056739, 0.2904309725956230603 ) ) ;
#27241 = CIRCLE ( 'NONE', #35133, 0.07999999999999996003 ) ;
#27242 = CARTESIAN_POINT ( 'NONE',  ( 0.3074989459046198470, -1.644816290331682085, 0.9179228641454580950 ) ) ;
#27243 = CARTESIAN_POINT ( 'NONE',  ( 0.4966101132311644406, -1.532727327792678951, 0.6782467145029912325 ) ) ;
#27244 = VECTOR ( 'NONE', #28204, 39.37007874015748143 ) ;
#27246 = CARTESIAN_POINT ( 'NONE',  ( 0.1876053338355621880, -0.6785855078148245179, 0.1477569985384105666 ) ) ;
#27245 = LINE ( 'NONE', #40581, #38136 ) ;
#27247 = CARTESIAN_POINT ( 'NONE',  ( 0.07484086907908865660, -1.207164791911022217, 0.6604330453735346440 ) ) ;
#27248 = VERTEX_POINT ( 'NONE', #17814 ) ;
#27249 = ORIENTED_EDGE ( 'NONE', *, *, #6855, .F. ) ;
#27250 = CARTESIAN_POINT ( 'NONE',  ( 0.3187641638634987618, -1.760284878867080183, 0.5597302103697527897 ) ) ;
#27251 = CARTESIAN_POINT ( 'NONE',  ( 0.5539872852267673231, -1.198627223726707491, 0.8202900059160223023 ) ) ;
#27252 = CARTESIAN_POINT ( 'NONE',  ( -0.02587796518899032269, -1.798561299892753714E-16, -0.5399999999999999245 ) ) ;
#27253 = EDGE_CURVE ( 'NONE', #40377, #34047, #10853, .T. ) ;
#27254 = CARTESIAN_POINT ( 'NONE',  ( -0.2043922129835736845, -0.5166151207188713901, 0.3749999999999999445 ) ) ;
#27255 = APPLIED_PERSON_AND_ORGANIZATION_ASSIGNMENT ( #22460, #16086, ( #39149 ) ) ;
#27256 = CIRCLE ( 'NONE', #32487, 0.1999999999999994837 ) ;
#27257 = CARTESIAN_POINT ( 'NONE',  ( 0.06837834821047945877, -1.326772567953161897, 0.5201612180504711080 ) ) ;
#27258 = AXIS2_PLACEMENT_3D ( 'NONE', #34062, #11657, #12269 ) ;
#27259 = CARTESIAN_POINT ( 'NONE',  ( 0.1621979957779212944, -1.277097269517335931, -0.6997590581617950667 ) ) ;
#27260 = CARTESIAN_POINT ( 'NONE',  ( 0.3283134639458292758, -1.178171897100129151, 0.5638118889048701066 ) ) ;
#27261 = CARTESIAN_POINT ( 'NONE',  ( 0.5555567715531690709, -1.190973094708358992, 0.5709149340790615756 ) ) ;
#27262 = AXIS2_PLACEMENT_3D ( 'NONE', #28310, #24428, #24844 ) ;
#27263 = PERSON_AND_ORGANIZATION ( #28500, #32463 ) ;
#27264 = AXIS2_PLACEMENT_3D ( 'NONE', #10943, #23504, #11548 ) ;
#27265 = LOCAL_TIME ( 0, 53, 7.000000000000000000, #31259 ) ;
#27266 = CARTESIAN_POINT ( 'NONE',  ( 0.1939472947763713484, -2.001291656381384954, -0.6721680726779954984 ) ) ;
#27267 = EDGE_LOOP ( 'NONE', ( #8898, #4009, #35569, #18470 ) ) ;
#27268 = DIRECTION ( 'NONE',  ( 1.000000000000000000, 1.023084414572561287E-11, 1.435532102222559952E-11 ) ) ;
#27269 = DIRECTION ( 'NONE',  ( 0.000000000000000000, -0.8063205929144885431, 0.5914787413272156735 ) ) ;
#27270 = AXIS2_PLACEMENT_3D ( 'NONE', #17865, #30430, #20781 ) ;
#27271 = CARTESIAN_POINT ( 'NONE',  ( -0.01548846960707406760, -0.3688619771572930750, -0.3775276577327001948 ) ) ;
#27272 = VERTEX_POINT ( 'NONE', #39623 ) ;
#27273 = CARTESIAN_POINT ( 'NONE',  ( 0.5318682467102796574, -1.150266585189366531, 0.6291131035211885436 ) ) ;
#27274 = DIRECTION ( 'NONE',  ( 0.8660254037844402619, -0.1903656704316006587, -0.4623428506218351663 ) ) ;
#27275 = CARTESIAN_POINT ( 'NONE',  ( 0.1756863999069679660, -1.240364938524567862, 0.7368202461708308615 ) ) ;
#27276 = ORIENTED_EDGE ( 'NONE', *, *, #25904, .F. ) ;
#27277 = ADVANCED_FACE ( 'NONE', ( #26893 ), #6703, .T. ) ;
#27278 = CARTESIAN_POINT ( 'NONE',  ( -0.1210148435730048905, -0.5061394519556924321, 0.1438724812234762340 ) ) ;
#27279 = CARTESIAN_POINT ( 'NONE',  ( 0.04762035657659133281, -0.04295292190959984491, 0.4802795956081307160 ) ) ;
#27280 = CARTESIAN_POINT ( 'NONE',  ( 0.03171861681799903465, -0.4702483710821712126, -0.2325697148610222365 ) ) ;
#27281 = DIRECTION ( 'NONE',  ( -8.881784197001246407E-16, 2.361472542561082612E-16, -1.000000000000000000 ) ) ;
#27282 = CIRCLE ( 'NONE', #6878, 0.1000000000000000194 ) ;
#27283 = EDGE_CURVE ( 'NONE', #38708, #11216, #20728, .T. ) ;
#27284 = CARTESIAN_POINT ( 'NONE',  ( 0.3957667564970019369, -1.142477732822457126, 0.6888951601802728586 ) ) ;
#27286 = CARTESIAN_POINT ( 'NONE',  ( 0.4751248519516730884, -1.681100737592190031, 0.5628962907142390781 ) ) ;
#27285 = CYLINDRICAL_SURFACE ( 'NONE', #31864, 0.1249999999999999584 ) ;
#27287 = ADVANCED_FACE ( 'NONE', ( #24413 ), #2780, .F. ) ;
#27288 = DIRECTION ( 'NONE',  ( 0.000000000000000000, 0.000000000000000000, -1.000000000000000000 ) ) ;
#27289 = EDGE_LOOP ( 'NONE', ( #28086, #16359, #2596, #4988 ) ) ;
#27290 = VECTOR ( 'NONE', #37918, 39.37007874015748143 ) ;
#27291 = EDGE_CURVE ( 'NONE', #34692, #39668, #12456, .T. ) ;
#27292 = CARTESIAN_POINT ( 'NONE',  ( -1.502516396515344672E-15, -0.3899999999999999578, 0.05000000000000055789 ) ) ;
#27293 = EDGE_LOOP ( 'NONE', ( #10436, #24673, #3817, #36536 ) ) ;
#27294 = CIRCLE ( 'NONE', #22050, 0.02999999999999997113 ) ;
#27295 = CARTESIAN_POINT ( 'NONE',  ( 0.1868687334809603917, -0.4547550531002670371, 0.05501147976861575639 ) ) ;
#27296 = CARTESIAN_POINT ( 'NONE',  ( 0.3705980884814369936, -1.414600388509865914, 0.8578092172935054549 ) ) ;
#27298 = CARTESIAN_POINT ( 'NONE',  ( 0.4370059147932298105, -1.114236431796985949, -0.6414654485229357439 ) ) ;
#27297 = CARTESIAN_POINT ( 'NONE',  ( -0.05083665881508921125, -0.4330284998000982211, 0.1917934360576655506 ) ) ;
#27299 = CARTESIAN_POINT ( 'NONE',  ( 0.4974456442574050619, -1.184401136727558868, 0.4224083929475309640 ) ) ;
#27300 = SECURITY_CLASSIFICATION ( '', '', #24966 ) ;
#27301 = ORIENTED_EDGE ( 'NONE', *, *, #11050, .T. ) ;
#27302 = ORIENTED_EDGE ( 'NONE', *, *, #39220, .T. ) ;
#27303 = CARTESIAN_POINT ( 'NONE',  ( 0.3972786276333574174, -2.032124455670578200, -0.4826101713713118468 ) ) ;
#27304 = CARTESIAN_POINT ( 'NONE',  ( 0.5800985813862742368, -1.490016391247783734, 0.6431135307928460554 ) ) ;
#27305 = AXIS2_PLACEMENT_3D ( 'NONE', #20787, #32892, #14582 ) ;
#27306 = CARTESIAN_POINT ( 'NONE',  ( 0.6699292074404794572, -1.569526485364059143, 0.6071573546319902759 ) ) ;
#27307 = LINE ( 'NONE', #21121, #6209 ) ;
#27308 = ADVANCED_FACE ( 'NONE', ( #11847 ), #25788, .F. ) ;
#27309 = CARTESIAN_POINT ( 'NONE',  ( 0.2923286432308245808, -1.660243258845594649, -0.3694143330441917450 ) ) ;
#27310 = CARTESIAN_POINT ( 'NONE',  ( -0.05464101615137787610, -2.551729310907437043, -0.5086726180052709712 ) ) ;
#27311 = CARTESIAN_POINT ( 'NONE',  ( 0.3933751395322774291, -1.752169251404669392, -0.4834917239368269337 ) ) ;
#27312 = CARTESIAN_POINT ( 'NONE',  ( 0.5616682974235900350, -1.585511599874633193, -0.5166151207188732775 ) ) ;
#27313 = CARTESIAN_POINT ( 'NONE',  ( 0.4717011137366580176, -1.062550488221034151, 0.8575416557712804977 ) ) ;
#27314 = DIRECTION ( 'NONE',  ( -1.355854680848614478E-31, 3.330669073875470114E-16, 1.000000000000000000 ) ) ;
#27315 = CARTESIAN_POINT ( 'NONE',  ( -0.1688017273025826936, 0.4914669153062960483, 0.3250764289764328518 ) ) ;
#27316 = B_SPLINE_CURVE_WITH_KNOTS ( 'NONE', 3,
 ( #24298, #18120, #21007, #40108, #34148, #15032 ),
 .UNSPECIFIED., .F., .F.,
 ( 4, 2, 4 ),
 ( 0.000000000000000000, 0.001177402821458509207, 0.002354805642917018414 ),
 .UNSPECIFIED. ) ;
#27317 = CARTESIAN_POINT ( 'NONE',  ( 0.5763042886240972162, -1.611411870786366940, -0.5437224079586429060 ) ) ;
#27318 = AXIS2_PLACEMENT_3D ( 'NONE', #21728, #21947, #36949 ) ;
#27319 = CARTESIAN_POINT ( 'NONE',  ( 0.01896931156525484205, 0.2428675472501187205, 0.4598342473848836542 ) ) ;
#27320 = CARTESIAN_POINT ( 'NONE',  ( 0.5862859414779472145, -1.607631461875910217, 0.5832712881534547478 ) ) ;
#27321 = DIRECTION ( 'NONE',  ( 0.8660512985181139101, 0.4999551463232366766, 0.000000000000000000 ) ) ;
#27322 = CARTESIAN_POINT ( 'NONE',  ( 2.072478234521481980E-16, 0.2900000000000004796, -0.04250000000000046102 ) ) ;
#27323 = APPLIED_SECURITY_CLASSIFICATION_ASSIGNMENT ( #3006, ( #5625 ) ) ;
#27324 = CARTESIAN_POINT ( 'NONE',  ( 0.001298983775798597754, -0.4632363948272406606, 0.3098607539948510792 ) ) ;
#27325 = CARTESIAN_POINT ( 'NONE',  ( 0.1316017208954911033, -1.248059642665102942, 0.5182417262812423209 ) ) ;
#27326 = CARTESIAN_POINT ( 'NONE',  ( 0.4296077269088024453, -1.643823256665882582, -0.6213498245139347231 ) ) ;
#27327 = DIRECTION ( 'NONE',  ( 5.551115123125845564E-17, 0.000000000000000000, -1.000000000000000000 ) ) ;
#27328 = VECTOR ( 'NONE', #6947, 39.37007874015748143 ) ;
#27329 = VERTEX_POINT ( 'NONE', #27309 ) ;
#27330 = EDGE_CURVE ( 'NONE', #25808, #36294, #34258, .T. ) ;
#27331 = CARTESIAN_POINT ( 'NONE',  ( 0.4697623592636160361, -1.061459377010899541, -0.6056023639864148711 ) ) ;
#27332 = CARTESIAN_POINT ( 'NONE',  ( 0.3571916633338231839, -1.156198450587171189, 0.5973401585408657510 ) ) ;
#27333 = FACE_OUTER_BOUND ( 'NONE', #19717, .T. ) ;
#27334 = CARTESIAN_POINT ( 'NONE',  ( 0.01548846960707524721, 0.000000000000000000, 0.000000000000000000 ) ) ;
#27335 = ADVANCED_FACE ( 'NONE', ( #34472 ), #27099, .T. ) ;
#27336 = CARTESIAN_POINT ( 'NONE',  ( 0.5229710184148730345, -1.333122656980544773, 0.5928855954934411088 ) ) ;
#27338 = VERTEX_POINT ( 'NONE', #3016 ) ;
#27337 = CARTESIAN_POINT ( 'NONE',  ( 0.3699999999999786793, -2.166079853131637645, -0.4467913981637915422 ) ) ;
#27339 = CARTESIAN_POINT ( 'NONE',  ( 0.5130887424854349010, -1.117175276521638505, 0.5842416974757255188 ) ) ;
#27340 = VERTEX_POINT ( 'NONE', #24828 ) ;
#27341 = EDGE_CURVE ( 'NONE', #25716, #10985, #11659, .T. ) ;
#27342 = CARTESIAN_POINT ( 'NONE',  ( 0.1756948879565448929, -1.266804977652423725, -0.3255180435861027011 ) ) ;
#27343 = EDGE_LOOP ( 'NONE', ( #29254, #19497, #14356, #1101 ) ) ;
#27344 = CARTESIAN_POINT ( 'NONE',  ( 0.08222542156927918622, -1.327483614382551913, 0.4683366274853996702 ) ) ;
#27345 = CARTESIAN_POINT ( 'NONE',  ( 0.3593153017356163215, -1.620878803526070389, 0.6356398769032042262 ) ) ;
#27347 = CARTESIAN_POINT ( 'NONE',  ( 0.1880119672192303582, -0.5274192702082527440, 0.09355512109399032050 ) ) ;
#27346 = CARTESIAN_POINT ( 'NONE',  ( 0.7068366539029264928, -1.522610279710209680, 0.5630547890730004390 ) ) ;
#27348 = DIRECTION ( 'NONE',  ( 0.3468893892380643384, -0.7396492646828627393, 0.5767033179097752482 ) ) ;
#27349 = EDGE_LOOP ( 'NONE', ( #25178, #11929, #25401, #17244 ) ) ;
#27350 = CIRCLE ( 'NONE', #10252, 0.03000000000000002318 ) ;
#27351 = CIRCLE ( 'NONE', #25384, 0.03749999999977551152 ) ;
#27352 = CARTESIAN_POINT ( 'NONE',  ( 0.4162193950359272532, -1.008383645579083554, 0.7108382935901826905 ) ) ;
#27353 = ORIENTED_EDGE ( 'NONE', *, *, #11992, .F. ) ;
#27354 = DIRECTION ( 'NONE',  ( 1.000000000000000000, 1.450080480853946466E-15, -8.881784197001242463E-16 ) ) ;
#27355 = CARTESIAN_POINT ( 'NONE',  ( 0.4015936175283410514, -1.155705023113092533, 0.5182417262812423209 ) ) ;
#27356 = ADVANCED_FACE ( 'NONE', ( #36741 ), #37351, .T. ) ;
#27357 = EDGE_CURVE ( 'NONE', #32770, #14928, #8550, .T. ) ;
#27358 = CARTESIAN_POINT ( 'NONE',  ( 0.3072783065116599377, -1.250270042923148583, 0.6870471857482981504 ) ) ;
#27359 = APPROVAL_PERSON_ORGANIZATION ( #2129, #40039, #27629 ) ;
#27360 = DIRECTION ( 'NONE',  ( 2.465190328815661892E-32, 1.000000000000000000, 6.656013887802287108E-31 ) ) ;
#27361 = EDGE_CURVE ( 'NONE', #31508, #16113, #6285, .T. ) ;
#27362 = CARTESIAN_POINT ( 'NONE',  ( 0.3933867764525452726, -1.106167708152965723, 0.6141292311898844947 ) ) ;
#27363 = EDGE_CURVE ( 'NONE', #1766, #38965, #37160, .T. ) ;
#27364 = AXIS2_PLACEMENT_3D ( 'NONE', #25177, #35032, #34824 ) ;
#27365 = CARTESIAN_POINT ( 'NONE',  ( 0.2197066928929958252, -0.9902086090378329208, 0.5562769007654783104 ) ) ;
#27366 = DIRECTION ( 'NONE',  ( 7.771561172376107616E-16, -7.170354002788761615E-17, 1.000000000000000000 ) ) ;
#27367 = CARTESIAN_POINT ( 'NONE',  ( 0.05561176441985765662, 0.2541700551350243309, -0.3845131534397753792 ) ) ;
#27368 = CARTESIAN_POINT ( 'NONE',  ( 0.3924513946351673721, -1.141110873382124913, 0.4807468720547258823 ) ) ;
#27369 = CARTESIAN_POINT ( 'NONE',  ( 0.002346242718065488699, -0.9632443647534850717, 0.3631189922238501344 ) ) ;
#27370 = SECURITY_CLASSIFICATION_LEVEL ( 'unclassified' ) ;
#27371 = CARTESIAN_POINT ( 'NONE',  ( 0.4844264163852358696, -1.123939254815026878, 0.5158946235675032632 ) ) ;
#27372 = CARTESIAN_POINT ( 'NONE',  ( 0.5566683473865443599, -1.184766897212384151, 0.6057417262809812186 ) ) ;
#27373 = CARTESIAN_POINT ( 'NONE',  ( -0.2399999999999999079, -2.945416957892569521, -0.4639726661791638840 ) ) ;
#27374 = VERTEX_POINT ( 'NONE', #21339 ) ;
#27375 = CARTESIAN_POINT ( 'NONE',  ( 0.01194366878076004966, -0.5146706732448569355, -0.04802372811395377861 ) ) ;
#27376 = CARTESIAN_POINT ( 'NONE',  ( -0.2746410161513776482, -3.840189043187996809, -0.1239867222638698224 ) ) ;
#27377 = CARTESIAN_POINT ( 'NONE',  ( 0.0004843130070887482585, -0.4400213179164120803, 0.1732464827935638330 ) ) ;
#27378 = VECTOR ( 'NONE', #24672, 39.37007874015748854 ) ;
#27379 = CARTESIAN_POINT ( 'NONE',  ( 0.3655107245187978471, -1.761138529012605369, -0.5889844493690715721 ) ) ;
#27380 = EDGE_LOOP ( 'NONE', ( #7370, #19991, #2847, #39952 ) ) ;
#27381 = ORIENTED_EDGE ( 'NONE', *, *, #18232, .F. ) ;
#27382 = CARTESIAN_POINT ( 'NONE',  ( -0.1178427669581002812, -0.4906303760369221667, 0.1227918960327450820 ) ) ;
#27383 = ORIENTED_EDGE ( 'NONE', *, *, #2671, .F. ) ;
#27384 = LOCAL_TIME ( 0, 53, 7.000000000000000000, #21008 ) ;
#27385 = CARTESIAN_POINT ( 'NONE',  ( 0.4030327056921978457, -1.680968334469209680, -0.4031266960524464427 ) ) ;
#27386 = EDGE_CURVE ( 'NONE', #1535, #30357, #33876, .T. ) ;
#27388 = ORIENTED_EDGE ( 'NONE', *, *, #36301, .F. ) ;
#27387 = CARTESIAN_POINT ( 'NONE',  ( -0.1157923916714887341, -0.5295015842442657439, 0.1380392329925907435 ) ) ;
#27390 = EDGE_LOOP ( 'NONE', ( #4122, #13709 ) ) ;
#27389 = CARTESIAN_POINT ( 'NONE',  ( -0.001014514837871428703, -0.7910287684333593416, 0.01309347023044784945 ) ) ;
#27391 = EDGE_CURVE ( 'NONE', #30357, #10402, #21194, .T. ) ;
#27392 = VECTOR ( 'NONE', #35939, 39.37007874015748143 ) ;
#27393 = ORIENTED_EDGE ( 'NONE', *, *, #19596, .F. ) ;
#27394 = DIRECTION ( 'NONE',  ( -1.000000000000000000, 0.000000000000000000, -1.138269997360103659E-15 ) ) ;
#27395 = ORIENTED_EDGE ( 'NONE', *, *, #8667, .T. ) ;
#27396 = CARTESIAN_POINT ( 'NONE',  ( 0.2694109831733587646, -1.541367803212651655, 0.8730078803289684775 ) ) ;
#27398 = CARTESIAN_POINT ( 'NONE',  ( 0.2225804103835565539, -1.238343994408460214, 0.5682417262808779901 ) ) ;
#27397 = CARTESIAN_POINT ( 'NONE',  ( 0.2011892967074957184, -1.251141541415955682, -0.3144976166544468099 ) ) ;
#27399 = DIRECTION ( 'NONE',  ( 1.000000000000000000, 0.000000000000000000, 0.000000000000000000 ) ) ;
#27400 = SECURITY_CLASSIFICATION_LEVEL ( 'unclassified' ) ;
#27401 = CARTESIAN_POINT ( 'NONE',  ( 0.7053410326410682885, -1.513865973459305625, 0.5669051209305092653 ) ) ;
#27403 = ORIENTED_EDGE ( 'NONE', *, *, #12014, .F. ) ;
#27402 = ORIENTED_EDGE ( 'NONE', *, *, #21404, .T. ) ;
#27404 = CARTESIAN_POINT ( 'NONE',  ( 0.1424029337235096226, -1.400533250147911746, -0.3552704771134632677 ) ) ;
#27405 = CARTESIAN_POINT ( 'NONE',  ( -0.04047076529493150165, -0.4923674059679353232, 0.09402950075400964836 ) ) ;
#27406 = CARTESIAN_POINT ( 'NONE',  ( 0.3373193197188696923, -1.055824305789904161, 0.7619749169485852125 ) ) ;
#27407 = CARTESIAN_POINT ( 'NONE',  ( 0.1855569663413472736, -0.8197182691652543651, 0.09662382917702272422 ) ) ;
#27408 = CARTESIAN_POINT ( 'NONE',  ( 0.03113248654051816583, 0.1969856463038233696, 0.03459270371430114843 ) ) ;
#27409 = CARTESIAN_POINT ( 'NONE',  ( 0.1997816917901940881, -2.061179784062637133, -0.2712838347678763196 ) ) ;
#27410 = FACE_OUTER_BOUND ( 'NONE', #3445, .T. ) ;
#27411 = CARTESIAN_POINT ( 'NONE',  ( 0.3935425020819560138, -1.717736786839809682, 0.4220810518247123388 ) ) ;
#27412 = VECTOR ( 'NONE', #8325, 39.37007874015748854 ) ;
#27413 = EDGE_CURVE ( 'NONE', #17214, #38375, #4754, .T. ) ;
#27414 = CARTESIAN_POINT ( 'NONE',  ( 0.3854140029834414172, -1.662020764902374381, -0.6188351660075884775 ) ) ;
#27415 = CARTESIAN_POINT ( 'NONE',  ( 0.4904112910084876820, -1.188461936721588508, 0.4282417262808777547 ) ) ;
#27416 = CARTESIAN_POINT ( 'NONE',  ( 0.2284923717121199460, -1.304659949875474068, -0.5155029497116575543 ) ) ;
#27417 = FACE_OUTER_BOUND ( 'NONE', #6452, .T. ) ;
#27418 = CARTESIAN_POINT ( 'NONE',  ( 0.3824171657898973176, -1.655877295464978527, -0.3991060487093113784 ) ) ;
#27419 = FACE_OUTER_BOUND ( 'NONE', #15576, .T. ) ;
#27420 = CARTESIAN_POINT ( 'NONE',  ( 0.2844183530474730937, -1.648412185216814541, 0.8663902821515296893 ) ) ;
#27421 = CARTESIAN_POINT ( 'NONE',  ( 0.01946601547008546679, -0.9333846633216874578, 0.6017762147510251625 ) ) ;
#27422 = DATE_AND_TIME ( #18543, #33894 ) ;
#27423 = CARTESIAN_POINT ( 'NONE',  ( 0.3136609249452982917, -0.7980415872784507592, 0.6920156437578004471 ) ) ;
#27424 = DIRECTION ( 'NONE',  ( 0.4999551463232372317, -0.8660512985181135770, 0.000000000000000000 ) ) ;
#27425 = CARTESIAN_POINT ( 'NONE',  ( 0.04157078424165680519, 0.01703670724029244729, -0.4699541233906586180 ) ) ;
#27426 = CYLINDRICAL_SURFACE ( 'NONE', #33607, 0.1500000000000000500 ) ;
#27427 = VERTEX_POINT ( 'NONE', #23108 ) ;
#27428 = CARTESIAN_POINT ( 'NONE',  ( 0.6479348668002676837, -1.454958465852009830, 0.4182417262808776348 ) ) ;
#27429 = CARTESIAN_POINT ( 'NONE',  ( 0.1712457320379880688, -1.308359377140657198, 0.9395131347236835850 ) ) ;
#27430 = ADVANCED_FACE ( 'NONE', ( #12653 ), #14599, .F. ) ;
#27431 = CARTESIAN_POINT ( 'NONE',  ( 0.5869881002782089130, -1.486012224770534740, 0.6423071506457943558 ) ) ;
#27432 = CARTESIAN_POINT ( 'NONE',  ( 0.3791949009533828741, -1.765055094326592577, -0.4492776787058168630 ) ) ;
#27434 = ORIENTED_EDGE ( 'NONE', *, *, #35060, .T. ) ;
#27433 = CARTESIAN_POINT ( 'NONE',  ( -0.1731185243557757936, 0.5373335498847187086, 0.3749999999999993894 ) ) ;
#27435 = CARTESIAN_POINT ( 'NONE',  ( 0.4936113061342744524, -1.107001320208115036, 0.7496827700887727097 ) ) ;
#27437 = ORIENTED_EDGE ( 'NONE', *, *, #18783, .T. ) ;
#27436 = EDGE_LOOP ( 'NONE', ( #22895, #9679, #35598, #29436 ) ) ;
#27438 = CARTESIAN_POINT ( 'NONE',  ( 0.2310704385326068921, -0.6810227473006470467, 0.4838669985239971161 ) ) ;
#27439 = FACE_OUTER_BOUND ( 'NONE', #8484, .T. ) ;
#27440 = CARTESIAN_POINT ( 'NONE',  ( 0.3187641638634987618, -1.760284878867080183, 0.5597302103697527897 ) ) ;
#27441 = CARTESIAN_POINT ( 'NONE',  ( -0.02872242845530527736, 0.4768947642620179894, -0.2371557650701878461 ) ) ;
#27442 = VERTEX_POINT ( 'NONE', #22158 ) ;
#27443 = CARTESIAN_POINT ( 'NONE',  ( 0.09148389223799407999, -0.7122299647079209928, 0.2589910736622687559 ) ) ;
#27444 = CARTESIAN_POINT ( 'NONE',  ( 0.2059273467974226113, -1.283046334493782359, -0.5931747813493345456 ) ) ;
#27445 = CARTESIAN_POINT ( 'NONE',  ( 0.4980715694105531388, -1.542567323246221145, 0.5836530299116245990 ) ) ;
#27447 = CARTESIAN_POINT ( 'NONE',  ( -0.001314104238682122210, -0.8140392535364435744, 0.03481557541610642154 ) ) ;
#27446 = CARTESIAN_POINT ( 'NONE',  ( 0.3335735135025916787, -1.761544825112107526, 0.4744483505433231829 ) ) ;
#27448 = CARTESIAN_POINT ( 'NONE',  ( 0.01358515540082348184, -1.035362938470157701, 0.5742360950302952682 ) ) ;
#27449 = ORIENTED_EDGE ( 'NONE', *, *, #25904, .T. ) ;
#27450 = VERTEX_POINT ( 'NONE', #34672 ) ;
#27451 = DIRECTION ( 'NONE',  ( 0.000000000000000000, 0.000000000000000000, -1.000000000000000000 ) ) ;
#27452 = CARTESIAN_POINT ( 'NONE',  ( 0.3426364375912121507, -0.9538486569171759077, 0.8392164456209516565 ) ) ;
#27453 = DIRECTION ( 'NONE',  ( 1.000000000000000000, 2.403560570595279103E-31, -1.725633230170969455E-31 ) ) ;
#27454 = FACE_OUTER_BOUND ( 'NONE', #7410, .T. ) ;
#27455 = SHAPE_REPRESENTATION_RELATIONSHIP ( 'NONE' , 'NONE' ,  #25967, #39278 ) ;
#27456 = ADVANCED_FACE ( 'NONE', ( #20223 ), #16611, .T. ) ;
#27457 = CARTESIAN_POINT ( 'NONE',  ( 0.5755305386461456729, -1.223609111988087861, 0.6057417262809032810 ) ) ;
#27458 = DIRECTION ( 'NONE',  ( 0.000000000000000000, 0.000000000000000000, 1.000000000000000000 ) ) ;
#27459 = CARTESIAN_POINT ( 'NONE',  ( 0.3223562399630707787, -1.181388948535295969, 0.4642260976938263894 ) ) ;
#27460 = CARTESIAN_POINT ( 'NONE',  ( 0.2003179398552689949, -0.7109237300142917659, 0.3290305662194804026 ) ) ;
#27461 = B_SPLINE_SURFACE_WITH_KNOTS ( 'NONE', 3, 1, ( 
 ( #35350, #29174 ),
 ( #20134, #20329 ),
 ( #16843, #38221 ),
 ( #22621, #32451 ),
 ( #32060, #23014 ),
 ( #38427, #29574 ) ),
 .UNSPECIFIED., .F., .F., .F.,
 ( 4, 2, 4 ),
 ( 2, 2 ),
 ( 1.913048296048411236E-15, 0.5000000000000000000, 1.228824370872419358 ),
 ( 0.000000000000000000, 1.000000000000000000 ),
 .UNSPECIFIED. ) ;
#27462 = COORDINATED_UNIVERSAL_TIME_OFFSET ( 0, 0, .AHEAD. ) ;
#27463 = CYLINDRICAL_SURFACE ( 'NONE', #35893, 0.1000000000000000056 ) ;
#27464 = CARTESIAN_POINT ( 'NONE',  ( 0.000000000000000000, 0.000000000000000000, 0.000000000000000000 ) ) ;
#27465 = CARTESIAN_POINT ( 'NONE',  ( 0.4434045676814238890, -1.200249727390046095, 0.6565421829911162188 ) ) ;
#27466 = CARTESIAN_POINT ( 'NONE',  ( -0.01548846960707393229, -0.07651041855119014579, 0.5222379212568235562 ) ) ;
#27467 = ORIENTED_EDGE ( 'NONE', *, *, #13749, .F. ) ;
#27468 = CARTESIAN_POINT ( 'NONE',  ( 0.4625870132446883165, -1.136566534039517018, 0.4526360456727940296 ) ) ;
#27469 = CARTESIAN_POINT ( 'NONE',  ( 0.08989780363036058153, -0.5646359461869331353, 0.1460065308160271857 ) ) ;
#27470 = ORIENTED_EDGE ( 'NONE', *, *, #14287, .F. ) ;
#27471 = CARTESIAN_POINT ( 'NONE',  ( -0.02953079040095606123, 0.09152108205202102997, -0.5223162075576446295 ) ) ;
#27472 = CARTESIAN_POINT ( 'NONE',  ( 0.02505718529252235621, -0.8981064542781922455, 0.5277094094783241207 ) ) ;
#27474 = EDGE_LOOP ( 'NONE', ( #21674, #6213, #1189, #16333 ) ) ;
#27473 = ORIENTED_EDGE ( 'NONE', *, *, #9314, .T. ) ;
#27475 = CARTESIAN_POINT ( 'NONE',  ( -0.04155248107635971244, 0.2901916982059713490, 0.3701002694350333799 ) ) ;
#27476 = CARTESIAN_POINT ( 'NONE',  ( 0.05269111014006671451, -0.009103832413163924150, 0.4686064687114369631 ) ) ;
#27477 = CARTESIAN_POINT ( 'NONE',  ( 0.7370562124357561418, -1.515684240363464941, 0.4449423861150900716 ) ) ;
#27478 = CARTESIAN_POINT ( 'NONE',  ( 0.3682365755625819914, -1.750444406184286761, -0.3437022085564034879 ) ) ;
#27479 = CARTESIAN_POINT ( 'NONE',  ( 0.4592765119208255808, -1.225248709697466909, 0.6570367264342110714 ) ) ;
#27481 = DIRECTION ( 'NONE',  ( 0.000000000000000000, 0.000000000000000000, -1.000000000000000000 ) ) ;
#27480 = CARTESIAN_POINT ( 'NONE',  ( 0.04211471441534279242, 0.4486586774158415336, 0.1367340165256794304 ) ) ;
#27482 = DIRECTION ( 'NONE',  ( 0.4999551463232372317, -0.8660512985181134660, 0.000000000000000000 ) ) ;
#27483 = ORIENTED_EDGE ( 'NONE', *, *, #34617, .T. ) ;
#27484 = ORIENTED_EDGE ( 'NONE', *, *, #10734, .T. ) ;
#27485 = CARTESIAN_POINT ( 'NONE',  ( 0.07797173117127408071, -1.322015870089231493, 0.5685938977595220711 ) ) ;
#27486 = ORIENTED_EDGE ( 'NONE', *, *, #3868, .F. ) ;
#27487 = PERSON ( 'NAUO-PER19', 'UNSPECIFIED', 'UNSPECIFIED', ('UNSPECIFIED'), ('UNSPECIFIED'), ('UNSPECIFIED') ) ;
#27488 = CARTESIAN_POINT ( 'NONE',  ( 0.5114126470110641476, -1.614748454822723556, -0.5166151207188711680 ) ) ;
#27489 = CARTESIAN_POINT ( 'NONE',  ( 0.4418185801296429238, -1.573801657680888866, 0.5756389504404278989 ) ) ;
#27491 = DIRECTION ( 'NONE',  ( 0.000000000000000000, -0.5877852522924463807, 0.8090169943749667691 ) ) ;
#27490 = DIRECTION ( 'NONE',  ( 0.000000000000000000, 0.000000000000000000, 1.000000000000000000 ) ) ;
#27492 = ORIENTED_EDGE ( 'NONE', *, *, #662, .T. ) ;
#27493 = CARTESIAN_POINT ( 'NONE',  ( -0.3000000000000000999, -2.477126460671948749, -0.4732852368073287574 ) ) ;
#27494 = CARTESIAN_POINT ( 'NONE',  ( 0.4032509867765149414, -1.739306358580214429, -0.3080928060649947287 ) ) ;
#27495 = CARTESIAN_POINT ( 'NONE',  ( 0.2128900943681608926, -0.8312134757594041856, 0.6484179518193018410 ) ) ;
#27496 = CARTESIAN_POINT ( 'NONE',  ( 0.4849335853385449147, -1.661118561410368732, 0.4921452663170099995 ) ) ;
#27497 = DIRECTION ( 'NONE',  ( -0.5608954083811059643, 0.8278866715058241788, 0.000000000000000000 ) ) ;
#27498 = CARTESIAN_POINT ( 'NONE',  ( -0.01895494625228227870, 0.5124113341948446365, 0.08888305413160398072 ) ) ;
#27499 = CARTESIAN_POINT ( 'NONE',  ( 0.4420022301528205300, -1.686445855772613855, 0.4182417262808775793 ) ) ;
#27500 = DIRECTION ( 'NONE',  ( -0.4999551463232373427, 0.8660512985181134660, -0.000000000000000000 ) ) ;
#27501 = DIRECTION ( 'NONE',  ( -1.416619696839552729E-11, -0.9510565162951545304, -0.3090169943749445092 ) ) ;
#27502 = EDGE_CURVE ( 'NONE', #9331, #11583, #1509, .T. ) ;
#27503 = CARTESIAN_POINT ( 'NONE',  ( 0.1998706582382908103, -0.5568697517490295290, 0.3524876158099713441 ) ) ;
#27504 = EDGE_CURVE ( 'NONE', #35126, #27130, #32334, .T. ) ;
#27505 = CARTESIAN_POINT ( 'NONE',  ( -0.05252049209742480629, 0.2682992380086470230, 0.3847779939372228397 ) ) ;
#27506 = FACE_OUTER_BOUND ( 'NONE', #3170, .T. ) ;
#27507 = EDGE_CURVE ( 'NONE', #5616, #24540, #33658, .T. ) ;
#27508 = CARTESIAN_POINT ( 'NONE',  ( 0.6027970226300880530, -1.572625850366509148, -0.6129179047768924526 ) ) ;
#27509 = CARTESIAN_POINT ( 'NONE',  ( 0.4358762597388673998, -1.693470429196241911, -0.6183159457888328658 ) ) ;
#27510 = CARTESIAN_POINT ( 'NONE',  ( 0.6574645389592653766, -1.565081392064861410, 0.6191400650029853514 ) ) ;
#27511 = ADVANCED_FACE ( 'NONE', ( #7227, #19047, #35633, #6479, #31580 ), #9776, .F. ) ;
#27512 = CARTESIAN_POINT ( 'NONE',  ( 0.6635030265783503634, -1.456878713983702056, 0.4329734231317256543 ) ) ;
#27513 = CARTESIAN_POINT ( 'NONE',  ( 0.1909286924077255587, -1.257064795538239022, -0.3614800891584005194 ) ) ;
#27514 = SHAPE_REPRESENTATION ( 'MAT-032', ( #23314, #27908, #14087, #8153, #4885, #3575, #34435, #7497, #24629, #18026, #13420, #40373, #36406, #12780, #10158 ), #8832 ) ;
#27515 = EDGE_LOOP ( 'NONE', ( #18174, #28374, #7162, #24391, #32573, #9847 ) ) ;
#27516 = CARTESIAN_POINT ( 'NONE',  ( 3.414809992080329023E-17, -0.4262518876079541830, 0.1639910581422319991 ) ) ;
#27517 = CARTESIAN_POINT ( 'NONE',  ( 0.5325131901480560925, -1.521657566433719300, 0.5503197480263272157 ) ) ;
#27518 = CARTESIAN_POINT ( 'NONE',  ( 0.1176733790823393522, -1.298938889880303371, 0.5182417262812425429 ) ) ;
#27519 = DIRECTION ( 'NONE',  ( 1.000000000000000000, 0.000000000000000000, 0.000000000000000000 ) ) ;
#27520 = ORIENTED_EDGE ( 'NONE', *, *, #35305, .T. ) ;
#27521 = CARTESIAN_POINT ( 'NONE',  ( 0.4535876148589958468, -1.088427983879621586, -0.6204185223330352938 ) ) ;
#27522 = ADVANCED_FACE ( 'NONE', ( #15956 ), #377, .T. ) ;
#27523 = FACE_OUTER_BOUND ( 'NONE', #5252, .T. ) ;
#27524 = DIRECTION ( 'NONE',  ( 1.000000000000000000, 1.138269997360101095E-15, -1.138269997360101095E-15 ) ) ;
#27525 = APPLIED_DATE_AND_TIME_ASSIGNMENT ( #39985, #28070, ( #17711 ) ) ;
#27526 = DIRECTION ( 'NONE',  ( 1.000000000000000000, 0.000000000000000000, 7.847503847416053677E-16 ) ) ;
#27527 = CARTESIAN_POINT ( 'NONE',  ( 0.4728208306174679354, -1.251385747785768610, 0.7149255309087257926 ) ) ;
#27529 = VERTEX_POINT ( 'NONE', #36039 ) ;
#27528 = DIRECTION ( 'NONE',  ( 0.8660512985181133550, 0.4999551463232371207, 0.000000000000000000 ) ) ;
#27530 = CARTESIAN_POINT ( 'NONE',  ( 0.3960970180006803121, -1.016137033769514808, 0.6457357589753065508 ) ) ;
#27531 = VERTEX_POINT ( 'NONE', #25436 ) ;
#27532 = APPLICATION_PROTOCOL_DEFINITION ( 'international standard', 'automotive_design', 2000, #7424 ) ;
#27533 = CARTESIAN_POINT ( 'NONE',  ( 0.1544872190154600589, -1.284018304476169714, -0.3339841533942207730 ) ) ;
#27534 = ORIENTED_EDGE ( 'NONE', *, *, #36555, .T. ) ;
#27535 = CARTESIAN_POINT ( 'NONE',  ( -0.02869712619511924009, 0.2420104654861718607, -0.4357576342647250245 ) ) ;
#27536 = ORIENTED_EDGE ( 'NONE', *, *, #10239, .T. ) ;
#27537 = CARTESIAN_POINT ( 'NONE',  ( 0.03562661732870475717, -0.5340764826629550432, 0.1545348805129083680 ) ) ;
#27539 = CARTESIAN_POINT ( 'NONE',  ( 0.1858368116309794815, -0.7426394543890098010, -0.01208864215565694927 ) ) ;
#27538 = CARTESIAN_POINT ( 'NONE',  ( 0.3511079287476752686, -1.164805985122749687, 0.4335040596137051394 ) ) ;
#27540 = DIRECTION ( 'NONE',  ( 0.000000000000000000, -0.7071067811865465735, -0.7071067811865484609 ) ) ;
#27541 = VERTEX_POINT ( 'NONE', #7841 ) ;
#27542 = ORIENTED_EDGE ( 'NONE', *, *, #27788, .T. ) ;
#27543 = CARTESIAN_POINT ( 'NONE',  ( 0.3607641608100094488, -0.9525365098903693095, 0.6616485578905302312 ) ) ;
#27544 = CARTESIAN_POINT ( 'NONE',  ( 0.4652240812381422952, -1.367871865765116990, 0.8203737607537802123 ) ) ;
#27545 = ORIENTED_EDGE ( 'NONE', *, *, #13943, .T. ) ;
#27546 = CARTESIAN_POINT ( 'NONE',  ( 0.1403991652838525728, -1.774344845793157655, -0.3580071914498583752 ) ) ;
#27547 = CARTESIAN_POINT ( 'NONE',  ( 0.05999999999999990757, 0.7171888913565960255, -0.2950238883388468514 ) ) ;
#27548 = CARTESIAN_POINT ( 'NONE',  ( 0.1954707032480469397, -1.039694013094895508, 0.7297344613678689029 ) ) ;
#27549 = CARTESIAN_POINT ( 'NONE',  ( 0.5664866863181922119, -1.581107300538653782, -0.4800253713849400583 ) ) ;
#27550 = CARTESIAN_POINT ( 'NONE',  ( -0.1204800139379124113, -0.5035717010276916650, 0.3194901984145553375 ) ) ;
#27551 = CARTESIAN_POINT ( 'NONE',  ( 0.4368279861777732975, -1.677667223885756398, 0.4182417262808776903 ) ) ;
#27552 = EDGE_CURVE ( 'NONE', #36330, #17659, #25818, .T. ) ;
#27553 = CARTESIAN_POINT ( 'NONE',  ( 0.6522089892707538805, -1.452491178199303956, 0.4224083929475448973 ) ) ;
#27554 = CARTESIAN_POINT ( 'NONE',  ( -0.02000000000000000042, -1.598492537578166672, -0.3371380022280838773 ) ) ;
#27555 = DIRECTION ( 'NONE',  ( 0.8660512985181130219, 0.4999551463232377868, 0.000000000000000000 ) ) ;
#27556 = DIRECTION ( 'NONE',  ( 0.000000000000000000, 3.330669073875470114E-16, 1.000000000000000000 ) ) ;
#27557 = APPLICATION_PROTOCOL_DEFINITION ( 'international standard', 'automotive_design', 2000, #11111 ) ;
#27558 = EDGE_CURVE ( 'NONE', #34759, #17214, #30443, .T. ) ;
#27559 = CARTESIAN_POINT ( 'NONE',  ( 0.4846870251237639371, -1.126101711201861644, 0.5058349955967992306 ) ) ;
#27560 = EDGE_CURVE ( 'NONE', #26649, #24616, #33013, .T. ) ;
#27561 = CARTESIAN_POINT ( 'NONE',  ( 0.3605448558321485697, -1.159604706203796631, 0.5182417262812284431 ) ) ;
#27562 = FACE_OUTER_BOUND ( 'NONE', #37647, .T. ) ;
#27563 = CARTESIAN_POINT ( 'NONE',  ( 0.0001246750752516694331, -0.5758935607867365913, -0.07708628032613852599 ) ) ;
#27564 = FACE_OUTER_BOUND ( 'NONE', #14654, .T. ) ;
#27565 = CARTESIAN_POINT ( 'NONE',  ( 0.2656972267752780725, -1.560961775696012355, -0.7135955925061087113 ) ) ;
#27566 = CARTESIAN_POINT ( 'NONE',  ( 0.7341807115343071954, -1.546815077829952978, 0.5182417262812423209 ) ) ;
#27567 = EDGE_LOOP ( 'NONE', ( #34026, #6409, #25405 ) ) ;
#27568 = EDGE_LOOP ( 'NONE', ( #19433, #23179, #24865, #6976 ) ) ;
#27569 = EDGE_CURVE ( 'NONE', #24060, #14824, #26191, .T. ) ;
#27570 = CARTESIAN_POINT ( 'NONE',  ( -0.1061036098701638175, -0.4827967145417200179, 0.3599999999999999867 ) ) ;
#27571 = ORIENTED_EDGE ( 'NONE', *, *, #22252, .F. ) ;
#27572 = CYLINDRICAL_SURFACE ( 'NONE', #39457, 0.07999999999999996003 ) ;
#27573 = DIRECTION ( 'NONE',  ( 0.000000000000000000, -0.9510565162951505336, 0.3090169943749571657 ) ) ;
#27575 = ORIENTED_EDGE ( 'NONE', *, *, #35525, .F. ) ;
#27574 = CARTESIAN_POINT ( 'NONE',  ( 0.002311469189254836219, -0.5280309338796042029, 0.1382921204161675355 ) ) ;
#27576 = ORIENTED_EDGE ( 'NONE', *, *, #194, .T. ) ;
#27577 = DIRECTION ( 'NONE',  ( -0.8660512985181133550, -0.4999551463232372317, 0.000000000000000000 ) ) ;
#27578 = ORIENTED_EDGE ( 'NONE', *, *, #39112, .F. ) ;
#27579 = CARTESIAN_POINT ( 'NONE',  ( 0.2656334329314738452, -1.675010518447552776, 0.5636784135978708532 ) ) ;
#27581 = CARTESIAN_POINT ( 'NONE',  ( 0.1765456504409605443, -1.243775442361034544, 0.6134035678024805094 ) ) ;
#27580 = CARTESIAN_POINT ( 'NONE',  ( 0.3045945486428198734, -1.056159242937262821, 0.7373969915095198724 ) ) ;
#27582 = CARTESIAN_POINT ( 'NONE',  ( 0.3613652144640472352, -1.159105058189230597, 0.5085157022477851951 ) ) ;
#27583 = APPROVAL_ROLE ( '' ) ;
#27584 = CARTESIAN_POINT ( 'NONE',  ( 0.1909288978607520115, -1.257065151435887040, -0.7137147910394006090 ) ) ;
#27586 = ORIENTED_EDGE ( 'NONE', *, *, #11488, .T. ) ;
#27585 = VERTEX_POINT ( 'NONE', #16923 ) ;
#27587 = CARTESIAN_POINT ( 'NONE',  ( 0.1734973056165642902, -1.209394307038482719, -0.5155029497116575543 ) ) ;
#27588 = CARTESIAN_POINT ( 'NONE',  ( 0.3793181961222715226, -1.724015678557569320, 0.4221277619539407500 ) ) ;
#27589 = CARTESIAN_POINT ( 'NONE',  ( 0.6465835049539362389, -1.539613817736340318, 0.4182417262808776903 ) ) ;
#27590 = CARTESIAN_POINT ( 'NONE',  ( 0.3759499381784230376, -1.134508656596316944, 0.8084154480762882899 ) ) ;
#27591 = CARTESIAN_POINT ( 'NONE',  ( 0.01202655180096142383, -0.9511917420203161999, 0.2808540945044247228 ) ) ;
#27592 = CARTESIAN_POINT ( 'NONE',  ( -2.196333431559634599E-13, -2.094416301789170820, -0.7275128151819897360 ) ) ;
#27593 = CARTESIAN_POINT ( 'NONE',  ( 0.000000000000000000, 0.1997995745459845707, -0.008951536808938304751 ) ) ;
#27594 = CARTESIAN_POINT ( 'NONE',  ( 0.3003069805930505543, -1.615165612650612426, 0.9446834537455470748 ) ) ;
#27595 = DIRECTION ( 'NONE',  ( 0.8660254037844378194, -0.2682606777263741304, 0.4219433715391058826 ) ) ;
#27596 = DIRECTION ( 'NONE',  ( -1.188678714063518227E-15, 1.000000000000000000, 3.263080277421930985E-16 ) ) ;
#27597 = CARTESIAN_POINT ( 'NONE',  ( -0.3000000000000000999, -3.647187793141847045, -0.4766722536777797115 ) ) ;
#27598 = ADVANCED_FACE ( 'NONE', ( #29467 ), #31398, .F. ) ;
#27599 = PLANE ( 'NONE',  #15364 ) ;
#27600 = CARTESIAN_POINT ( 'NONE',  ( -0.0004530311258370896157, -0.9366683044365211597, 0.1504526319320767802 ) ) ;
#27601 = CARTESIAN_POINT ( 'NONE',  ( 0.3518531909964315307, -1.625880855532917169, -0.4272450907526114117 ) ) ;
#27602 = DIRECTION ( 'NONE',  ( -1.387778780781446292E-17, 0.9852735424593122016, 0.1709855155552010841 ) ) ;
#27603 = EDGE_CURVE ( 'NONE', #7855, #13458, #32339, .T. ) ;
#27604 = AXIS2_PLACEMENT_3D ( 'NONE', #24289, #15022, #11925 ) ;
#27605 = CYLINDRICAL_SURFACE ( 'NONE', #24536, 0.07999999999999996003 ) ;
#27606 = CARTESIAN_POINT ( 'NONE',  ( 0.003124719664520401140, -0.5686731593868927792, 0.1286173008190011902 ) ) ;
#27607 = CARTESIAN_POINT ( 'NONE',  ( 0.06466273788562305891, -1.136606943108019463, 0.7597147705880777924 ) ) ;
#27608 = APPROVAL_DATE_TIME ( #5584, #22255 ) ;
#27609 = CARTESIAN_POINT ( 'NONE',  ( 0.3805742881279173817, -0.9147748976205605231, 0.7744170315737640697 ) ) ;
#27610 = AXIS2_PLACEMENT_3D ( 'NONE', #23021, #9654, #15820 ) ;
#27611 = ADVANCED_FACE ( 'NONE', ( #11956 ), #39587, .F. ) ;
#27612 = DIRECTION ( 'NONE',  ( 1.000000000000000000, 1.119941574063613413E-31, -7.771561172376107616E-16 ) ) ;
#27613 = CARTESIAN_POINT ( 'NONE',  ( 0.02238826743733072361, -0.06997574608431053611, -0.5076331681966341769 ) ) ;
#27614 = CARTESIAN_POINT ( 'NONE',  ( 0.3431621118303436191, -1.692997266099296461, -0.4130752873103220035 ) ) ;
#27615 = ORIENTED_EDGE ( 'NONE', *, *, #36924, .F. ) ;
#27616 = CARTESIAN_POINT ( 'NONE',  ( 0.6451746001002063302, -1.456551915967818189, 0.4182417262808775238 ) ) ;
#27617 = CARTESIAN_POINT ( 'NONE',  ( 0.2388294604317064973, -1.536022005946620528, 0.8953658808002388225 ) ) ;
#27618 = ADVANCED_FACE ( 'NONE', ( #4750, #20833, #8457, #36837, #21021, #11149 ), #5576, .T. ) ;
#27619 = CARTESIAN_POINT ( 'NONE',  ( 0.5887768677989536625, -1.490289241820755617, 0.6055812475267198236 ) ) ;
#27621 = ORIENTED_EDGE ( 'NONE', *, *, #15483, .T. ) ;
#27620 = CARTESIAN_POINT ( 'NONE',  ( 0.3600571967235919879, -1.747985310352905719, 0.4400630855740547132 ) ) ;
#27622 = EDGE_CURVE ( 'NONE', #39166, #4242, #19868, .T. ) ;
#27623 = CARTESIAN_POINT ( 'NONE',  ( 0.3225930820597290305, -0.8396780885765841029, 0.6764912411861826458 ) ) ;
#27625 = ORIENTED_EDGE ( 'NONE', *, *, #38305, .F. ) ;
#27624 = ORIENTED_EDGE ( 'NONE', *, *, #35078, .T. ) ;
#27626 = CARTESIAN_POINT ( 'NONE',  ( 0.1690930997617906550, -1.307384335399499831, -0.7282839042959697862 ) ) ;
#27627 = CARTESIAN_POINT ( 'NONE',  ( 0.3633532330403487776, -1.743361738801966210, -0.5306750697200927069 ) ) ;
#27628 = FACE_OUTER_BOUND ( 'NONE', #37729, .T. ) ;
#27629 = APPROVAL_ROLE ( '' ) ;
#27630 = CIRCLE ( 'NONE', #38124, 0.9087847906030128708 ) ;
#27631 = LINE ( 'NONE', #40161, #29006 ) ;
#27632 = EDGE_LOOP ( 'NONE', ( #13244, #14261, #17140 ) ) ;
#27633 = CARTESIAN_POINT ( 'NONE',  ( 0.09278646505816903756, -0.7145150594772067265, 0.2750910907217022361 ) ) ;
#27634 = LINE ( 'NONE', #37091, #26650 ) ;
#27635 = CARTESIAN_POINT ( 'NONE',  ( 0.4972415774783536802, -1.542437756487440303, 0.5698391771344212264 ) ) ;
#27637 = CARTESIAN_POINT ( 'NONE',  ( -0.0001015365960684644825, -0.6986948758057686115, -0.02208683258971757754 ) ) ;
#27636 = CARTESIAN_POINT ( 'NONE',  ( 0.3226000049158921912, -1.763919894439656133, 0.5248175239680957782 ) ) ;
#27638 = CARTESIAN_POINT ( 'NONE',  ( 7.048302186126095272E-05, -0.9486411243827373996, 0.1970497354082177133 ) ) ;
#27639 = ORIENTED_EDGE ( 'NONE', *, *, #8501, .T. ) ;
#27640 = VERTEX_POINT ( 'NONE', #29880 ) ;
#27641 = CIRCLE ( 'NONE', #17782, 0.1620173459747806799 ) ;
#27642 = CARTESIAN_POINT ( 'NONE',  ( -0.2399999999999999079, -2.292669950144801572, -0.8383185228372386222 ) ) ;
#27643 = CARTESIAN_POINT ( 'NONE',  ( 0.6033864073621231228, -1.403448924263456021, 0.8611617019206015966 ) ) ;
#27644 = CARTESIAN_POINT ( 'NONE',  ( 0.4042628496030684637, -1.723800573128688507, -0.6015185938071440086 ) ) ;
#27645 = DIRECTION ( 'NONE',  ( 0.000000000000000000, 0.000000000000000000, 1.000000000000000000 ) ) ;
#27646 = EDGE_CURVE ( 'NONE', #29368, #20774, #16579, .T. ) ;
#27647 = CARTESIAN_POINT ( 'NONE',  ( 0.3744125517984470131, -1.759357067434767607, -0.4355489755031470289 ) ) ;
#27648 = CARTESIAN_POINT ( 'NONE',  ( 0.2614959211572117637, -1.678097089283488330, 0.5385591481521548873 ) ) ;
#27649 = EDGE_CURVE ( 'NONE', #8445, #11170, #36450, .T. ) ;
#27650 = CARTESIAN_POINT ( 'NONE',  ( 0.3593346688482154661, -1.735925422213635549, -0.5010936962835144115 ) ) ;
#27651 = CARTESIAN_POINT ( 'NONE',  ( 0.5530797604979859061, -1.185210387710321944, 0.6074893116751658440 ) ) ;
#27652 = COORDINATED_UNIVERSAL_TIME_OFFSET ( 0, 0, .AHEAD. ) ;
#27653 = CARTESIAN_POINT ( 'NONE',  ( -0.1138236225804938051, -0.5205343845807006709, 0.3387850541077466748 ) ) ;
#27654 = AXIS2_PLACEMENT_3D ( 'NONE', #39356, #14661, #5802 ) ;
#27655 = CARTESIAN_POINT ( 'NONE',  ( 0.3671187914973310096, -2.025419988125670034, -0.6786350348123257881 ) ) ;
#27656 = CARTESIAN_POINT ( 'NONE',  ( 0.4905717239428445953, -1.546361816834758152, 0.5738993346725939082 ) ) ;
#27657 = DIRECTION ( 'NONE',  ( 1.000000000000000000, 2.280301054154495132E-31, -1.664003471950577689E-31 ) ) ;
#27658 = CIRCLE ( 'NONE', #4641, 0.04999999999999998890 ) ;
#27659 = ORIENTED_EDGE ( 'NONE', *, *, #12228, .F. ) ;
#27660 = DIRECTION ( 'NONE',  ( -1.000000000000000000, -2.280301054154495132E-31, 1.664003471950577689E-31 ) ) ;
#27661 = TOROIDAL_SURFACE ( 'NONE', #9919, 0.08249999999977548903, 0.01000000000000000021 ) ;
#27662 = CARTESIAN_POINT ( 'NONE',  ( -0.03478556507499944855, -0.2420934825333271312, 0.4561854036929733902 ) ) ;
#27663 = DIRECTION ( 'NONE',  ( 0.000000000000000000, -0.8090169943749496717, -0.5877852522924700285 ) ) ;
#27664 = ORIENTED_EDGE ( 'NONE', *, *, #12184, .F. ) ;
#27665 = CARTESIAN_POINT ( 'NONE',  ( -0.04139678531769593051, 0.01699044972118296526, -0.4702883835734110174 ) ) ;
#27666 = CARTESIAN_POINT ( 'NONE',  ( 0.04094777560533426064, -0.9548371111386207977, 0.6396399729219502950 ) ) ;
#27668 = ORIENTED_EDGE ( 'NONE', *, *, #16565, .T. ) ;
#27667 = ORIENTED_EDGE ( 'NONE', *, *, #8785, .T. ) ;
#27669 = CARTESIAN_POINT ( 'NONE',  ( 0.3083966533127217580, -1.760901789209341262, 0.5682271305178940857 ) ) ;
#27670 = CARTESIAN_POINT ( 'NONE',  ( -0.01548846960707524721, 0.000000000000000000, 0.000000000000000000 ) ) ;
#27671 = CARTESIAN_POINT ( 'NONE',  ( 0.05561310505366701823, -0.4316274075649161324, -0.1617055803010020720 ) ) ;
#27672 = CARTESIAN_POINT ( 'NONE',  ( 0.1966547502198365549, -1.674282070017420576, -0.3593914745891567675 ) ) ;
#27673 = CARTESIAN_POINT ( 'NONE',  ( 0.01548846960706664298, -0.5198120922912313757, 0.07362328916749247276 ) ) ;
#27675 = CARTESIAN_POINT ( 'NONE',  ( 0.2059273467974226113, -1.283046334493782359, -0.5931747813493345456 ) ) ;
#27674 = CARTESIAN_POINT ( 'NONE',  ( 0.05252049209742985086, 0.4488546425834872844, 0.1362647994370476678 ) ) ;
#27676 = CARTESIAN_POINT ( 'NONE',  ( -0.05283710938261081819, -0.3063690517300527993, -0.3541964274677634195 ) ) ;
#27677 = ORIENTED_EDGE ( 'NONE', *, *, #6970, .F. ) ;
#27678 = CARTESIAN_POINT ( 'NONE',  ( 0.3824648761862433632, -1.161281635269272305, 0.4182417262808778013 ) ) ;
#27679 = ORIENTED_EDGE ( 'NONE', *, *, #40406, .T. ) ;
#27680 = CARTESIAN_POINT ( 'NONE',  ( 0.04582705327698215897, 0.06484491888963163364, 0.4826014279685452157 ) ) ;
#27681 = CARTESIAN_POINT ( 'NONE',  ( 0.3805693354401638029, -1.436365483031340595, 0.8498359687909504689 ) ) ;
#27683 = DIRECTION ( 'NONE',  ( -6.162975822039154730E-33, 0.000000000000000000, -1.000000000000000000 ) ) ;
#27682 = CARTESIAN_POINT ( 'NONE',  ( -0.1167294259372891468, -0.5331983348239500708, 0.1528658435937000626 ) ) ;
#27684 = CARTESIAN_POINT ( 'NONE',  ( 0.3047936848243344432, -1.756875962071034580, 0.5682417262361116883 ) ) ;
#27685 = CARTESIAN_POINT ( 'NONE',  ( 0.1999999999735330158, -2.091146487246815955, -0.6943973668278335953 ) ) ;
#27686 = B_SPLINE_CURVE_WITH_KNOTS ( 'NONE', 3,
 ( #4521, #17086, #33126, #29634, #27169, #17500 ),
 .UNSPECIFIED., .F., .F.,
 ( 4, 2, 4 ),
 ( 0.000000000000000000, 0.0005458736207840705207, 0.001091747241568141041 ),
 .UNSPECIFIED. ) ;
#27687 = ORIENTED_EDGE ( 'NONE', *, *, #38043, .T. ) ;
#27688 = AXIS2_PLACEMENT_3D ( 'NONE', #31123, #3140, #29197 ) ;
#27689 = CARTESIAN_POINT ( 'NONE',  ( 0.4703191885827326946, -1.592420631535068187, -0.5958679092299303814 ) ) ;
#27690 = CARTESIAN_POINT ( 'NONE',  ( 0.1951391704723344500, -1.987894887562734469, -0.2907895905339114018 ) ) ;
#27691 = CIRCLE ( 'NONE', #3356, 0.03749999999977551152 ) ;
#27692 = CARTESIAN_POINT ( 'NONE',  ( 0.1232466757695174497, -0.5723387072628065564, 0.2472162040730083721 ) ) ;
#27693 = CARTESIAN_POINT ( 'NONE',  ( 0.4839100550601997952, -1.674307978549753440, 0.5301044316523388922 ) ) ;
#27694 = DIRECTION ( 'NONE',  ( 1.000000000000000000, 2.280301054154496446E-31, 1.355854680848613603E-31 ) ) ;
#27695 = EDGE_LOOP ( 'NONE', ( #31117, #36674, #3749, #39113 ) ) ;
#27696 = CARTESIAN_POINT ( 'NONE',  ( 0.05999999999999990757, 0.2217800815169825301, -0.07875759618522079619 ) ) ;
#27697 = VECTOR ( 'NONE', #19534, 39.37007874015748143 ) ;
#27698 = CARTESIAN_POINT ( 'NONE',  ( 0.2059273467974224725, -1.283046334493782137, -0.3824824602286829855 ) ) ;
#27699 = AXIS2_PLACEMENT_3D ( 'NONE', #14872, #39957, #36861 ) ;
#27700 = FACE_BOUND ( 'NONE', #38552, .T. ) ;
#27701 = CARTESIAN_POINT ( 'NONE',  ( 0.2347838743403539985, -1.231490626770528563, 0.5148488905547541350 ) ) ;
#27702 = CARTESIAN_POINT ( 'NONE',  ( 0.6789872039812443472, -1.407470790535994221, 0.5375528621076278712 ) ) ;
#27703 = CARTESIAN_POINT ( 'NONE',  ( -0.04047076529492606850, 0.2415772653364889611, 0.4392125161515883502 ) ) ;
#27704 = CARTESIAN_POINT ( 'NONE',  ( 0.01018801482832277540, -1.013890353644918862, 0.5362285315871677671 ) ) ;
#27705 = CARTESIAN_POINT ( 'NONE',  ( 0.6067827457248362588, -1.586506025082006444, -0.4704708140563562679 ) ) ;
#27706 = CARTESIAN_POINT ( 'NONE',  ( 0.4559719632891930385, -1.698713290701216350, -0.5155029497116575543 ) ) ;
#27707 = CARTESIAN_POINT ( 'NONE',  ( -0.3000000000000000999, -2.376910030844113564, -0.7058185084100425666 ) ) ;
#27708 = CARTESIAN_POINT ( 'NONE',  ( 0.3925833169928708566, -1.148390097986053293, 0.4243636716995100588 ) ) ;
#27709 = CARTESIAN_POINT ( 'NONE',  ( 0.1909286924077255310, -1.257064795538239022, -0.3824824602286830411 ) ) ;
#27710 = VERTEX_POINT ( 'NONE', #33355 ) ;
#27711 = CARTESIAN_POINT ( 'NONE',  ( 0.3658297366832103936, -1.745592370396175541, -0.4954708084374070953 ) ) ;
#27712 = CARTESIAN_POINT ( 'NONE',  ( 0.3951778266041646170, -1.698641715122608087, -0.6047022095078790072 ) ) ;
#27713 = CARTESIAN_POINT ( 'NONE',  ( 0.4112193008909713066, -1.591609915476099868, -0.6177460231409267477 ) ) ;
#27714 = CARTESIAN_POINT ( 'NONE',  ( 0.3624061103390691096, -1.968824918581854932, -0.4968426515055719972 ) ) ;
#27715 = ORIENTED_EDGE ( 'NONE', *, *, #4254, .F. ) ;
#27716 = CARTESIAN_POINT ( 'NONE',  ( 0.5172910145744592514, -1.680634944436373512, -0.5803635445752998168 ) ) ;
#27717 = AXIS2_PLACEMENT_3D ( 'NONE', #26581, #19780, #10122 ) ;
#27718 = CIRCLE ( 'NONE', #17203, 0.5302738246768092800 ) ;
#27719 = CARTESIAN_POINT ( 'NONE',  ( 0.3816469784432204304, -1.141973345686314811, 0.6053139149380659667 ) ) ;
#27720 = DIRECTION ( 'NONE',  ( -1.654489825136704222E-31, 0.9510565162951546414, 0.3090169943749438985 ) ) ;
#27721 = CARTESIAN_POINT ( 'NONE',  ( 0.04575106512775098389, 0.2311453587453343173, -0.4288095618640244133 ) ) ;
#27722 = AXIS2_PLACEMENT_3D ( 'NONE', #35101, #6904, #19479 ) ;
#27723 = CARTESIAN_POINT ( 'NONE',  ( 0.5337345016547716536, -1.351630938401003235, 0.5946468524951272761 ) ) ;
#27725 = ORIENTED_EDGE ( 'NONE', *, *, #21997, .T. ) ;
#27724 = FACE_OUTER_BOUND ( 'NONE', #33438, .T. ) ;
#27726 = CARTESIAN_POINT ( 'NONE',  ( 0.3630793090018165636, -0.9924503543686107321, 0.6290125294248597454 ) ) ;
#27727 = ORIENTED_EDGE ( 'NONE', *, *, #15538, .T. ) ;
#27728 = DATE_AND_TIME ( #24861, #18773 ) ;
#27729 = CARTESIAN_POINT ( 'NONE',  ( 0.1612877650847679423, -1.277903580349897039, -0.3312613801211721221 ) ) ;
#27730 = VERTEX_POINT ( 'NONE', #36235 ) ;
#27731 = CARTESIAN_POINT ( 'NONE',  ( 0.009367919695839343336, -0.5831258035308336529, 0.02670069209610665198 ) ) ;
#27732 = CARTESIAN_POINT ( 'NONE',  ( 0.03562661732870521514, -0.5340764826629550432, 0.1457185332388687693 ) ) ;
#27734 = CARTESIAN_POINT ( 'NONE',  ( 0.1762014475043635342, -0.5919070258151631903, -0.06363282137695237817 ) ) ;
#27733 = FACE_OUTER_BOUND ( 'NONE', #19764, .T. ) ;
#27735 = ADVANCED_FACE ( 'NONE', ( #26801 ), #25368, .F. ) ;
#27736 = VERTEX_POINT ( 'NONE', #39734 ) ;
#27737 = ORIENTED_EDGE ( 'NONE', *, *, #15770, .F. ) ;
#27738 = CARTESIAN_POINT ( 'NONE',  ( 0.3375401459729027720, -0.9900294755946262848, 0.5931500777746694375 ) ) ;
#27739 = EDGE_CURVE ( 'NONE', #27741, #27226, #12002, .T. ) ;
#27740 = CARTESIAN_POINT ( 'NONE',  ( 0.5154828406948165354, -1.449888099294595500, 0.7698194787142327300 ) ) ;
#27741 = VERTEX_POINT ( 'NONE', #15049 ) ;
#27742 = CARTESIAN_POINT ( 'NONE',  ( 0.2447871629624292500, -1.421848713596993496, -0.3349537587709216502 ) ) ;
#27743 = DIRECTION ( 'NONE',  ( 1.000000000000000000, 1.213308482346485395E-12, 2.286601241528059267E-12 ) ) ;
#27744 = CARTESIAN_POINT ( 'NONE',  ( 0.04430295985701804273, -1.505275273055644902, -0.3761050495259261606 ) ) ;
#27745 = VECTOR ( 'NONE', #40638, 39.37007874015748143 ) ;
#27746 = CARTESIAN_POINT ( 'NONE',  ( -0.1124400704934123835, -0.5139941482047849508, 0.3450122074418399687 ) ) ;
#27747 = DIRECTION ( 'NONE',  ( 5.551115123125845564E-17, 0.000000000000000000, -1.000000000000000000 ) ) ;
#27748 = VECTOR ( 'NONE', #13419, 39.37007874015748854 ) ;
#27749 = CARTESIAN_POINT ( 'NONE',  ( 0.07556315841227354002, -1.331191507351498160, 0.4849083929475443422 ) ) ;
#27750 =( BOUNDED_SURFACE ( )  B_SPLINE_SURFACE ( 3, 2, ( 
 ( #22899, #31724, #9514 ),
 ( #3540, #12808, #25371 ),
 ( #10120, #10335, #37902 ),
 ( #9714, #34799, #13012 ),
 ( #22697, #19399, #6601 ),
 ( #19183, #35228, #19595 ),
 ( #907, #25983, #38508 ),
 ( #16110, #35416, #7212 ),
 ( #19777, #4137, #12591 ),
 ( #7416, #4347, #19994 ),
 ( #33336, #32529, #7826 ),
 ( #4949, #29452, #26578 ),
 ( #23691, #1105, #36021 ),
 ( #26786, #17514, #38900 ),
 ( #30063, #5145, #17305 ),
 ( #26176, #39312, #20203 ) ),
 .UNSPECIFIED., .F., .F., .T. ) 
 B_SPLINE_SURFACE_WITH_KNOTS ( ( 4, 2, 2, 2, 2, 2, 2, 4 ),
 ( 3, 3 ),
 ( 0.000000000000000000, 0.0008688684136184839351, 0.001303302620427725794, 0.001737736827236967870, 0.002172171034046209946, 0.002606605240855451588, 0.003041039447664693664, 0.003475473654473935740 ),
 ( 0.000000000000000000, 1.000000000000000000 ),
 .UNSPECIFIED. ) 
 GEOMETRIC_REPRESENTATION_ITEM ( )  RATIONAL_B_SPLINE_SURFACE ( (
 ( 1.000000000000000000, 0.7071067811865511255, 1.000000000000000000),
 ( 1.000000000000000000, 0.7497868472460812450, 1.000000000000000000),
 ( 1.000000000000000000, 0.7816256484933949977, 1.000000000000000000),
 ( 1.000000000000000000, 0.8066966545080302975, 1.000000000000000000),
 ( 1.000000000000000000, 0.8110625487245798348, 1.000000000000000000),
 ( 1.000000000000000000, 0.8155049440654144055, 1.000000000000000000),
 ( 1.000000000000000000, 0.8158287745906235289, 1.000000000000000000),
 ( 1.000000000000000000, 0.8158343461500251470, 1.000000000000000000),
 ( 1.000000000000000000, 0.8155513814744629331, 1.000000000000000000),
 ( 1.000000000000000000, 0.8111133430346705309, 1.000000000000000000),
 ( 1.000000000000000000, 0.8067191351272415822, 1.000000000000000000),
 ( 1.000000000000000000, 0.7903519271076608899, 1.000000000000000000),
 ( 1.000000000000000000, 0.7782561128466314315, 1.000000000000000000),
 ( 1.000000000000000000, 0.7472427613862036022, 1.000000000000000000),
 ( 1.000000000000000000, 0.7284546171351224952, 1.000000000000000000),
 ( 1.000000000000000000, 0.7071067811866026398, 1.000000000000000000) ) ) 
 REPRESENTATION_ITEM ( '' )  SURFACE ( )  );
#27751 = AXIS2_PLACEMENT_3D ( 'NONE', #3729, #13169, #18540 ) ;
#27752 = CARTESIAN_POINT ( 'NONE',  ( 0.08546473275284281745, -1.263146999130163373, 0.5182417262812423209 ) ) ;
#27753 = EDGE_CURVE ( 'NONE', #1527, #8287, #11755, .T. ) ;
#27754 = CARTESIAN_POINT ( 'NONE',  ( 0.2847549724830318874, -1.551417661949121118, -0.6853099816877789019 ) ) ;
#27755 = CARTESIAN_POINT ( 'NONE',  ( 0.08097120591835743619, -1.368856899881548683, 0.5761801428003342496 ) ) ;
#27756 = PRODUCT_CONTEXT ( 'NONE', #11111, 'mechanical' ) ;
#27757 = APPROVAL ( #21851, 'UNSPECIFIED' ) ;
#27758 = AXIS2_PLACEMENT_3D ( 'NONE', #24551, #21472, #37080 ) ;
#27759 = CARTESIAN_POINT ( 'NONE',  ( 0.4532329859814145934, -1.135673831482812979, 0.4497956394000192093 ) ) ;
#27760 = CARTESIAN_POINT ( 'NONE',  ( 0.5535089670275162854, -1.186427276555303001, 0.6057417262809813296 ) ) ;
#27761 = DIRECTION ( 'NONE',  ( -1.000000000000000000, -2.280301054154495132E-31, 1.664003471950577689E-31 ) ) ;
#27762 = CARTESIAN_POINT ( 'NONE',  ( -0.002083146443013336215, -0.8967360763018585867, 0.1624439089914547774 ) ) ;
#27763 = DIRECTION ( 'NONE',  ( -1.000000000000000000, -7.857794173099924470E-32, -8.628166150854818811E-32 ) ) ;
#27764 = DIRECTION ( 'NONE',  ( 0.000000000000000000, 0.000000000000000000, -1.000000000000000000 ) ) ;
#27765 = CARTESIAN_POINT ( 'NONE',  ( 0.1876560278723298503, -1.258954043299216119, -0.2885605078359608222 ) ) ;
#27766 = ORIENTED_EDGE ( 'NONE', *, *, #22252, .T. ) ;
#27767 = ORIENTED_EDGE ( 'NONE', *, *, #5390, .T. ) ;
#27768 = CARTESIAN_POINT ( 'NONE',  ( -0.1053653701217057148, -0.4790241930300679352, 0.1089215720160038869 ) ) ;
#27769 = ORIENTED_EDGE ( 'NONE', *, *, #15694, .F. ) ;
#27770 = DIRECTION ( 'NONE',  ( 1.000000000000000000, 1.671477276948179358E-11, 5.600159359328154813E-12 ) ) ;
#27771 = AXIS2_PLACEMENT_3D ( 'NONE', #8260, #24314, #33161 ) ;
#27772 = CARTESIAN_POINT ( 'NONE',  ( -0.1068489084554431895, -0.4866459697500206683, 0.09652185631084100881 ) ) ;
#27774 = ORIENTED_EDGE ( 'NONE', *, *, #7666, .F. ) ;
#27773 = CARTESIAN_POINT ( 'NONE',  ( -0.1212602504878775439, -0.5073146173917505442, 0.3032895567580813356 ) ) ;
#27775 = ADVANCED_FACE ( 'NONE', ( #11567 ), #32947, .F. ) ;
#27776 = EDGE_LOOP ( 'NONE', ( #28993, #515, #24254, #32199 ) ) ;
#27777 = LINE ( 'NONE', #39917, #34324 ) ;
#27778 = EDGE_CURVE ( 'NONE', #4952, #10331, #219, .T. ) ;
#27779 = AXIS2_PLACEMENT_3D ( 'NONE', #30043, #33316, #36001 ) ;
#27780 = ORIENTED_EDGE ( 'NONE', *, *, #23061, .T. ) ;
#27781 = VECTOR ( 'NONE', #33223, 39.37007874015748854 ) ;
#27782 = CARTESIAN_POINT ( 'NONE',  ( 0.003557204563558416955, -0.5929878893131403927, 0.3587067422883609691 ) ) ;
#27784 = CARTESIAN_POINT ( 'NONE',  ( 0.08667892099931116812, -1.311828707399254279, 0.5891665326009013492 ) ) ;
#27783 = CARTESIAN_POINT ( 'NONE',  ( -0.2746410161513779258, -4.056386786973173564, -0.6915988348251679296 ) ) ;
#27785 = DIRECTION ( 'NONE',  ( 0.8660512985181133550, 0.4999551463232372317, 0.000000000000000000 ) ) ;
#27786 = AXIS2_PLACEMENT_3D ( 'NONE', #26924, #39455, #11087 ) ;
#27787 = EDGE_CURVE ( 'NONE', #12918, #21695, #34988, .T. ) ;
#27788 = EDGE_CURVE ( 'NONE', #24651, #37794, #19228, .T. ) ;
#27789 = CARTESIAN_POINT ( 'NONE',  ( -0.1163452666694987092, -0.5320157244525056672, 0.3133290949221909094 ) ) ;
#27791 = ORIENTED_EDGE ( 'NONE', *, *, #6908, .T. ) ;
#27790 = ORIENTED_EDGE ( 'NONE', *, *, #36827, .F. ) ;
#27792 = EDGE_CURVE ( 'NONE', #2643, #4246, #25132, .T. ) ;
#27793 = CARTESIAN_POINT ( 'NONE',  ( 0.01128677947712186484, -0.9461986806730106059, 0.1457185332388702959 ) ) ;
#27794 = CARTESIAN_POINT ( 'NONE',  ( 0.4242133616548364183, -1.734366925052854391, -0.4397180493288433967 ) ) ;
#27795 = CARTESIAN_POINT ( 'NONE',  ( -0.05076541221973769613, -0.4633004642377251958, 0.09914728473419444355 ) ) ;
#27796 = CARTESIAN_POINT ( 'NONE',  ( 0.4923102438893445232, -1.287854413602990133, 0.8084835653369039088 ) ) ;
#27797 = CIRCLE ( 'NONE', #19889, 0.04999999999999998890 ) ;
#27798 = CARTESIAN_POINT ( 'NONE',  ( 0.02999999999851975241, -2.094416301510383605, -0.7275128150656288151 ) ) ;
#27799 = CARTESIAN_POINT ( 'NONE',  ( 0.5403448000457758971, -1.667326427136834432, -0.4959994330086618941 ) ) ;
#27800 = CARTESIAN_POINT ( 'NONE',  ( 0.3241018648587293272, -1.757744033614132118, 0.6567149589598120230 ) ) ;
#27801 = FACE_OUTER_BOUND ( 'NONE', #7058, .T. ) ;
#27802 = CARTESIAN_POINT ( 'NONE',  ( 0.4144363316557380661, -1.243523414473156397, 0.5370935844994736419 ) ) ;
#27803 = CARTESIAN_POINT ( 'NONE',  ( 0.5694934407712974878, -1.613350223101006620, 0.4177417262808785781 ) ) ;
#27804 = CARTESIAN_POINT ( 'NONE',  ( -0.02000000000000000042, -2.082394770077036661, -0.4779740388940064144 ) ) ;
#27805 = EDGE_CURVE ( 'NONE', #17210, #1749, #30382, .T. ) ;
#27806 = LINE ( 'NONE', #15464, #21408 ) ;
#27807 = AXIS2_PLACEMENT_3D ( 'NONE', #13124, #32056, #25687 ) ;
#27808 = B_SPLINE_CURVE_WITH_KNOTS ( 'NONE', 3,
 ( #10866, #13929, #26117, #19914 ),
 .UNSPECIFIED., .F., .F.,
 ( 4, 4 ),
 ( 1.734723475976807094E-18, 0.0003881528371572850154 ),
 .UNSPECIFIED. ) ;
#27809 = DIRECTION ( 'NONE',  ( -0.4999551463232373427, 0.8660512985181134660, -0.000000000000000000 ) ) ;
#27810 = CARTESIAN_POINT ( 'NONE',  ( 0.002089204316143729572, -0.4812299151504488837, 0.2002484561318531031 ) ) ;
#27811 = CARTESIAN_POINT ( 'NONE',  ( 0.03947150132052767296, -1.011495197293007076, 0.7004091584170603069 ) ) ;
#27812 = PERSON_AND_ORGANIZATION_ROLE ( 'design_supplier' ) ;
#27813 = AXIS2_PLACEMENT_3D ( 'NONE', #10867, #23628, #23441 ) ;
#27814 = CARTESIAN_POINT ( 'NONE',  ( 0.7227036224969136669, -1.477504586156484612, 0.6121051687398550989 ) ) ;
#27815 = AXIS2_PLACEMENT_3D ( 'NONE', #23833, #36354, #2017 ) ;
#27816 = CARTESIAN_POINT ( 'NONE',  ( 0.6776375915179856380, -1.553024467591962665, 0.6114064090131621221 ) ) ;
#27817 = CARTESIAN_POINT ( 'NONE',  ( 0.03170874437002789425, -0.05432941731172213906, -0.4888251740112578014 ) ) ;
#27818 = CIRCLE ( 'NONE', #33060, 0.01499999999999995261 ) ;
#27819 = AXIS2_PLACEMENT_3D ( 'NONE', #8920, #2961, #8315 ) ;
#27820 = CARTESIAN_POINT ( 'NONE',  ( -0.2399999999999999079, -2.323257895298838971, -0.7902071827178637209 ) ) ;
#27821 = VERTEX_POINT ( 'NONE', #18752 ) ;
#27822 = CARTESIAN_POINT ( 'NONE',  ( -0.3000000000000000999, -3.291368864184587739, -0.6988176298300774469 ) ) ;
#27823 = CARTESIAN_POINT ( 'NONE',  ( 0.2529494766129096739, -1.556025590441917128, 0.8771849030697340677 ) ) ;
#27824 = CARTESIAN_POINT ( 'NONE',  ( 0.1283662278338046081, -0.5536758349069195173, 0.1788647258318563915 ) ) ;
#27826 = ORIENTED_EDGE ( 'NONE', *, *, #20755, .T. ) ;
#27825 = LINE ( 'NONE', #12192, #5977 ) ;
#27827 = CARTESIAN_POINT ( 'NONE',  ( 0.4660228360541302517, -1.069033551699853479, 0.7465831672886248382 ) ) ;
#27829 = ORIENTED_EDGE ( 'NONE', *, *, #30152, .F. ) ;
#27828 = ORIENTED_EDGE ( 'NONE', *, *, #19314, .F. ) ;
#27830 = CARTESIAN_POINT ( 'NONE',  ( 0.4100237506442933610, -0.9802720315809884122, 0.7587508493699357537 ) ) ;
#27831 = EDGE_CURVE ( 'NONE', #37319, #4571, #6077, .T. ) ;
#27832 = DIRECTION ( 'NONE',  ( 0.000000000000000000, 0.000000000000000000, -1.000000000000000000 ) ) ;
#27833 = CARTESIAN_POINT ( 'NONE',  ( -0.08000000000000000167, -2.196071624283071788, -0.8624000883860228894 ) ) ;
#27834 = COORDINATED_UNIVERSAL_TIME_OFFSET ( 0, 0, .AHEAD. ) ;
#27835 = EDGE_CURVE ( 'NONE', #2400, #16986, #7368, .T. ) ;
#27836 = FACE_OUTER_BOUND ( 'NONE', #6558, .T. ) ;
#27837 = ORIENTED_EDGE ( 'NONE', *, *, #16782, .F. ) ;
#27838 = EDGE_CURVE ( 'NONE', #15019, #26971, #14698, .T. ) ;
#27839 = CARTESIAN_POINT ( 'NONE',  ( 0.08779053797915296886, -0.7269445601652628763, 0.2094401179698018867 ) ) ;
#27840 = AXIS2_PLACEMENT_3D ( 'NONE', #34485, #25853, #4012 ) ;
#27841 = CARTESIAN_POINT ( 'NONE',  ( 0.3106403372944860908, -1.755530900668034189, 0.6572509151387877502 ) ) ;
#27842 = CIRCLE ( 'NONE', #16040, 0.1999999999999999278 ) ;
#27843 = CARTESIAN_POINT ( 'NONE',  ( 0.1312703668873084484, -0.6769293281215125191, 0.4711565125189325354 ) ) ;
#27845 = CARTESIAN_POINT ( 'NONE',  ( 2.048885995248197414E-16, 0.2900000000000004796, -5.122214988120493288E-16 ) ) ;
#27844 = CARTESIAN_POINT ( 'NONE',  ( 0.3290154599841292327, -1.759929421022380369, 0.4808583447391158727 ) ) ;
#27846 = CARTESIAN_POINT ( 'NONE',  ( -0.05561176441985817703, -0.2871508736821589136, 0.3605511861568549414 ) ) ;
#27847 = ORIENTED_EDGE ( 'NONE', *, *, #2997, .T. ) ;
#27848 = CARTESIAN_POINT ( 'NONE',  ( 0.4266995953040617628, -1.696353446692786981, 0.4244815370374785402 ) ) ;
#27849 = CARTESIAN_POINT ( 'NONE',  ( 0.3413008603379567019, -0.8270678360722266698, 0.7412715964732541352 ) ) ;
#27850 = AXIS2_PLACEMENT_3D ( 'NONE', #3813, #22169, #12888 ) ;
#27851 = DIRECTION ( 'NONE',  ( 0.4999551463232372317, -0.8660512985181135770, 0.000000000000000000 ) ) ;
#27852 = ADVANCED_FACE ( 'NONE', ( #68, #9075 ), #9689, .F. ) ;
#27853 = CIRCLE ( 'NONE', #35068, 0.1600000000000007527 ) ;
#27854 = CARTESIAN_POINT ( 'NONE',  ( -0.1873388932668320073, 0.5325605939836577374, 0.3599999999999993205 ) ) ;
#27855 = EDGE_CURVE ( 'NONE', #9762, #39882, #36296, .T. ) ;
#27856 = CARTESIAN_POINT ( 'NONE',  ( 0.4012095065101706770, -1.155916531200418484, 0.4182417262808778013 ) ) ;
#27857 = ADVANCED_FACE ( 'NONE', ( #16075 ), #36338, .F. ) ;
#27858 = CARTESIAN_POINT ( 'NONE',  ( 0.04510596909177587432, -1.502102959356099277, -0.6428203672274495073 ) ) ;
#27859 = LINE ( 'NONE', #5820, #25136 ) ;
#27860 = CARTESIAN_POINT ( 'NONE',  ( 0.5031347454681565079, -1.114267567382387414, 0.6816460158534795033 ) ) ;
#27861 = APPROVAL_STATUS ( 'not_yet_approved' ) ;
#27862 = DIRECTION ( 'NONE',  ( 0.000000000000000000, 3.330669073875470114E-16, 1.000000000000000000 ) ) ;
#27863 = CIRCLE ( 'NONE', #25913, 0.2200000000000000844 ) ;
#27864 = CARTESIAN_POINT ( 'NONE',  ( -0.01548846960707517956, -0.3772621329472692908, 0.3651003739303441131 ) ) ;
#27865 = DIRECTION ( 'NONE',  ( 4.930380657631319405E-32, 0.4913225862583635584, 0.8709776783778060416 ) ) ;
#27866 = CARTESIAN_POINT ( 'NONE',  ( -0.03642997641689543764, -0.08373618209167926763, 0.5050295872266582498 ) ) ;
#27867 = AXIS2_PLACEMENT_3D ( 'NONE', #24799, #14914, #17784 ) ;
#27868 = AXIS2_PLACEMENT_3D ( 'NONE', #22583, #13513, #6505 ) ;
#27869 = ORIENTED_EDGE ( 'NONE', *, *, #35522, .F. ) ;
#27870 = LINE ( 'NONE', #30940, #35157 ) ;
#27871 = APPROVAL_PERSON_ORGANIZATION ( #19910, #14192, #23218 ) ;
#27872 = CARTESIAN_POINT ( 'NONE',  ( 0.1499999999999994671, -0.5346638663566692928, 0.07572681171513533094 ) ) ;
#27873 = CARTESIAN_POINT ( 'NONE',  ( 0.08984346464585953040, -0.5645865489369916723, 0.1381676437203310515 ) ) ;
#27874 = ORIENTED_EDGE ( 'NONE', *, *, #382, .T. ) ;
#27875 = CARTESIAN_POINT ( 'NONE',  ( -0.05137569054208909053, 0.02238181648184895539, -0.4716086671401685804 ) ) ;
#27876 = CONICAL_SURFACE ( 'NONE', #23926, 0.1500000000000009936, 1.047197551196599408 ) ;
#27877 = CARTESIAN_POINT ( 'NONE',  ( 0.1685152595565323486, -1.372181050131067614, 0.6250859892303964882 ) ) ;
#27879 = EDGE_LOOP ( 'NONE', ( #26724, #92, #14736, #4605 ) ) ;
#27878 = ORIENTED_EDGE ( 'NONE', *, *, #2465, .T. ) ;
#27880 = CARTESIAN_POINT ( 'NONE',  ( -0.1126900943766902807, -0.5191528597923980026, 0.1491007326289749135 ) ) ;
#27881 = CARTESIAN_POINT ( 'NONE',  ( 2.072478234521481980E-16, 0.2900000000000004796, -0.04250000000000046102 ) ) ;
#27882 = CARTESIAN_POINT ( 'NONE',  ( 0.7437969124434082868, -1.515212563166708604, 0.5942788597236812187 ) ) ;
#27883 = CARTESIAN_POINT ( 'NONE',  ( 0.1980544885252993881, -2.023080723334441888, -0.3130069968383289991 ) ) ;
#27884 = DIRECTION ( 'NONE',  ( 1.000000000000000000, 2.403560570595279103E-31, -1.725633230170969455E-31 ) ) ;
#27885 = EDGE_CURVE ( 'NONE', #32770, #37196, #12774, .T. ) ;
#27887 = CARTESIAN_POINT ( 'NONE',  ( 0.05999999999999990757, 0.000000000000000000, 0.000000000000000000 ) ) ;
#27886 = CARTESIAN_POINT ( 'NONE',  ( 0.03672309138970048653, 0.4682479968340216847, 0.1092356788912528659 ) ) ;
#27888 = CARTESIAN_POINT ( 'NONE',  ( 0.03170874437002830365, -0.3312776501327927003, -0.3635338427919229121 ) ) ;
#27889 = ORIENTED_EDGE ( 'NONE', *, *, #17058, .T. ) ;
#27890 = EDGE_CURVE ( 'NONE', #24566, #30626, #30878, .T. ) ;
#27891 = CARTESIAN_POINT ( 'NONE',  ( 0.1321480585992808876, -0.6771580847970606332, 0.5036894915659911875 ) ) ;
#27892 = EDGE_LOOP ( 'NONE', ( #30711, #37079 ) ) ;
#27893 = CARTESIAN_POINT ( 'NONE',  ( 0.7043549991621405049, -1.517507936983845562, 0.5724489891249867624 ) ) ;
#27894 = CARTESIAN_POINT ( 'NONE',  ( 0.08644374222443337863, -0.6311465605765145259, 0.4038393922213947551 ) ) ;
#27896 = CARTESIAN_POINT ( 'NONE',  ( 0.5743547643448889684, -1.610790646010106686, 0.4680204833954097476 ) ) ;
#27895 = CARTESIAN_POINT ( 'NONE',  ( -0.05634301242525709824, -0.4332457820339908894, 0.1515812001271522325 ) ) ;
#27897 = CARTESIAN_POINT ( 'NONE',  ( -0.1196601186823846308, -0.4996350631411415333, 0.1296977380670712998 ) ) ;
#27898 = CARTESIAN_POINT ( 'NONE',  ( -0.2399999999999999079, -2.183180860297908144, -0.5562760292030870524 ) ) ;
#27899 = AXIS2_PLACEMENT_3D ( 'NONE', #29039, #3752, #32130 ) ;
#27900 = DIRECTION ( 'NONE',  ( -1.000000000000000000, -0.000000000000000000, -0.000000000000000000 ) ) ;
#27901 = CARTESIAN_POINT ( 'NONE',  ( 0.3986242379676584457, -2.054315208824561090, -0.4776734711709474945 ) ) ;
#27902 = AXIS2_PLACEMENT_3D ( 'NONE', #35337, #14330, #14522 ) ;
#27903 = CARTESIAN_POINT ( 'NONE',  ( 0.1289834210817078219, -0.6043023202742757727, 0.3280125156933150210 ) ) ;
#27904 = CARTESIAN_POINT ( 'NONE',  ( 0.4773291537012285812, -1.665277132842807539, 0.4700098364638956583 ) ) ;
#27905 = DIRECTION ( 'NONE',  ( 0.8660512985181134660, 0.4999551463232373427, 0.000000000000000000 ) ) ;
#27906 = AXIS2_PLACEMENT_3D ( 'NONE', #12671, #25235, #37775 ) ;
#27907 = CARTESIAN_POINT ( 'NONE',  ( -0.02231181081520786438, 0.4612879682508959078, 0.2235517164227159292 ) ) ;
#27908 = AXIS2_PLACEMENT_3D ( 'NONE', #31699, #34982, #38264 ) ;
#27909 = CARTESIAN_POINT ( 'NONE',  ( 0.5909188805876135486, -1.601585752074797142, 0.4182417262808776348 ) ) ;
#27910 = CARTESIAN_POINT ( 'NONE',  ( -0.07216878364870298046, 0.07999999999999969635, -0.1249999999999999029 ) ) ;
#27911 = CARTESIAN_POINT ( 'NONE',  ( 0.1840556061914042918, -0.8547754003400971357, 0.1463983740523600863 ) ) ;
#27912 = AXIS2_PLACEMENT_3D ( 'NONE', #29216, #13769, #19364 ) ;
#27913 = CARTESIAN_POINT ( 'NONE',  ( 0.2575330336140166931, -0.6922558787343077169, 0.5832620184353838333 ) ) ;
#27914 = CARTESIAN_POINT ( 'NONE',  ( -0.04285534776242195393, 0.2295064659597298717, 0.4383723578020115585 ) ) ;
#27915 = CARTESIAN_POINT ( 'NONE',  ( 0.07216878364870175921, 0.000000000000000000, -0.1249999999999971689 ) ) ;
#27916 = CARTESIAN_POINT ( 'NONE',  ( 0.5894785928677049869, -1.594119400354429672, -0.4403033262486665267 ) ) ;
#27917 = FACE_OUTER_BOUND ( 'NONE', #18358, .T. ) ;
#27918 = CARTESIAN_POINT ( 'NONE',  ( 0.08736999187406781220, -0.8328363605256602353, 0.2358003664843119906 ) ) ;
#27919 = CARTESIAN_POINT ( 'NONE',  ( -0.2399999999999999079, -2.461298705151934829, -0.7594706439553173816 ) ) ;
#27920 = CARTESIAN_POINT ( 'NONE',  ( -2.070754768975509919, -0.09959325338431655739, 0.1000000000000005745 ) ) ;
#27921 = B_SPLINE_CURVE_WITH_KNOTS ( 'NONE', 3,
 ( #25063, #37597, #21998, #9418, #20, #3849, #34522, #28558, #3663, #22203 ),
 .UNSPECIFIED., .F., .F.,
 ( 4, 2, 2, 2, 4 ),
 ( 0.002185774412332532404, 0.002876031867927643197, 0.003566289323522753556, 0.004256546779117863916, 0.004946804234712974709 ),
 .UNSPECIFIED. ) ;
#27922 = VERTEX_POINT ( 'NONE', #34367 ) ;
#27923 = CARTESIAN_POINT ( 'NONE',  ( 0.3626713113217782114, -1.760022178122295777, -0.5161757929854556837 ) ) ;
#27924 = DIRECTION ( 'NONE',  ( 0.4999551463232372317, -0.8660512985181135770, 0.000000000000000000 ) ) ;
#27925 = CIRCLE ( 'NONE', #6236, 0.1000000000000000194 ) ;
#27926 = CARTESIAN_POINT ( 'NONE',  ( 0.6498387395261642219, -1.464631408770378895, 0.4182417262808778013 ) ) ;
#27927 = CARTESIAN_POINT ( 'NONE',  ( 0.3912779971226761355, -1.730232005297420717, 0.6096916113967504325 ) ) ;
#27928 = AXIS2_PLACEMENT_3D ( 'NONE', #18821, #34027, #24373 ) ;
#27929 = ORIENTED_EDGE ( 'NONE', *, *, #15292, .T. ) ;
#27930 = CARTESIAN_POINT ( 'NONE',  ( 0.5122377809615301647, -1.683552081278821833, -0.5849915291001885898 ) ) ;
#27931 = CARTESIAN_POINT ( 'NONE',  ( 0.4265404446467185307, -1.123912635142109817, 0.5182417262812248904 ) ) ;
#27932 = LOCAL_TIME ( 0, 53, 7.000000000000000000, #32446 ) ;
#27933 = CARTESIAN_POINT ( 'NONE',  ( -0.02000000000000000042, -2.183180860297908144, -0.4937760292030871079 ) ) ;
#27934 = CARTESIAN_POINT ( 'NONE',  ( 0.05076679145661696507, 0.2374648372614248382, -0.4099810879409672149 ) ) ;
#27935 = CARTESIAN_POINT ( 'NONE',  ( 0.3927094301483936567, -1.138811079655472902, 0.7324022214491040517 ) ) ;
#27937 = ORIENTED_EDGE ( 'NONE', *, *, #35065, .F. ) ;
#27936 = CARTESIAN_POINT ( 'NONE',  ( -0.02587796518899032269, 0.000000000000000000, 0.000000000000000000 ) ) ;
#27938 = CARTESIAN_POINT ( 'NONE',  ( 0.2554252512568409572, -0.9178124959013912454, 0.5002157811656953168 ) ) ;
#27939 = VERTEX_POINT ( 'NONE', #31695 ) ;
#27940 = DATE_TIME_ROLE ( 'creation_date' ) ;
#27941 =( REPRESENTATION_RELATIONSHIP ('NONE','NONE', #27514, #30147 ) REPRESENTATION_RELATIONSHIP_WITH_TRANSFORMATION ( #23508 )SHAPE_REPRESENTATION_RELATIONSHIP( ) );
#27942 = VECTOR ( 'NONE', #3018, 39.37007874015748854 ) ;
#27943 = CARTESIAN_POINT ( 'NONE',  ( 0.1047008573566304973, -1.402533878584439453, 0.6140111174542888239 ) ) ;
#27944 = ORIENTED_EDGE ( 'NONE', *, *, #25995, .T. ) ;
#27945 = VERTEX_POINT ( 'NONE', #3514 ) ;
#27946 = CARTESIAN_POINT ( 'NONE',  ( 0.3775997949916232166, -1.569494078844261731, 0.7643415720515360778 ) ) ;
#27948 = CARTESIAN_POINT ( 'NONE',  ( 0.1135149208409055033, -0.6240967447601386553, -0.08736365982372026884 ) ) ;
#27947 = DIRECTION ( 'NONE',  ( 1.000000000000000000, 0.000000000000000000, 0.000000000000000000 ) ) ;
#27949 = CARTESIAN_POINT ( 'NONE',  ( 0.01548846960707524721, 0.4638115001430962447, -0.2459753896937880435 ) ) ;
#27950 = EDGE_LOOP ( 'NONE', ( #33017, #17601, #19816, #22726, #3699 ) ) ;
#27951 = VERTEX_POINT ( 'NONE', #18336 ) ;
#27952 = CARTESIAN_POINT ( 'NONE',  ( 0.4610375578740096847, -1.058108534101625198, 0.6327206492055766907 ) ) ;
#27953 = CARTESIAN_POINT ( 'NONE',  ( 0.5534818102155456554, -1.511209893663564952, 0.5824172004013893345 ) ) ;
#27954 = ORIENTED_EDGE ( 'NONE', *, *, #4642, .F. ) ;
#27955 = CARTESIAN_POINT ( 'NONE',  ( 0.2065475242433257030, -1.810140062844285413, -0.3513024119729122874 ) ) ;
#27956 = CARTESIAN_POINT ( 'NONE',  ( -2.372745691485074626E-32, 5.828670879282072084E-17, 0.1749999999999999889 ) ) ;
#27957 = CARTESIAN_POINT ( 'NONE',  ( 0.5648676111026831315, -1.582764309389034896, -0.4871114102051288253 ) ) ;
#27958 = CIRCLE ( 'NONE', #1688, 0.01500000000000001853 ) ;
#27959 = DIRECTION ( 'NONE',  ( 1.000000000000000000, 2.280301054154495132E-31, -1.664003471950577689E-31 ) ) ;
#27960 = CIRCLE ( 'NONE', #30594, 0.02999999999999997113 ) ;
#27961 = CARTESIAN_POINT ( 'NONE',  ( 0.3999999999999787059, -2.120797187169804143, -0.5256435360466945594 ) ) ;
#27962 = CARTESIAN_POINT ( 'NONE',  ( -0.2399999999999999079, -3.961846414800720861, -0.6040940090217902236 ) ) ;
#27963 = CARTESIAN_POINT ( 'NONE',  ( -0.2136509456379323546, -0.4946207598421927254, 0.1000000000000000194 ) ) ;
#27964 = CARTESIAN_POINT ( 'NONE',  ( 0.4263817149093077630, -1.123637674285695276, 0.5237040708327734828 ) ) ;
#27965 = CARTESIAN_POINT ( 'NONE',  ( 0.07801557919154505916, -1.344960384177054546, 0.6336995499099050688 ) ) ;
#27966 = PERSON_AND_ORGANIZATION ( #28500, #32463 ) ;
#27967 = APPLIED_APPROVAL_ASSIGNMENT ( #28254, ( #35536 ) ) ;
#27968 = CARTESIAN_POINT ( 'NONE',  ( 0.2225775331702970761, -0.9343733720331020010, 0.4090965549137709489 ) ) ;
#27969 = CARTESIAN_POINT ( 'NONE',  ( 0.4676908246382645018, -1.116468242743651418, 0.5700470834645430251 ) ) ;
#27970 = CARTESIAN_POINT ( 'NONE',  ( 0.4567988949776999319, -1.218949203222925659, 0.6057417262810179670 ) ) ;
#27971 = AXIS2_PLACEMENT_3D ( 'NONE', #20371, #4707, #1670 ) ;
#27972 = DIRECTION ( 'NONE',  ( 0.000000000000000000, 6.829619984160661399E-15, -1.000000000000000000 ) ) ;
#27973 = CARTESIAN_POINT ( 'NONE',  ( 0.0006292437964357017102, -0.9180166443092167006, 0.3683461522897012452 ) ) ;
#27974 = DIRECTION ( 'NONE',  ( 0.4999999999999955591, 0.000000000000000000, -0.8660254037844411501 ) ) ;
#27975 = CARTESIAN_POINT ( 'NONE',  ( 0.1786812025795815329, -1.892228462347241624, -0.6870626404130494302 ) ) ;
#27976 = CARTESIAN_POINT ( 'NONE',  ( -0.02000000000000000042, -2.122347498858831116, -0.8313396097929491857 ) ) ;
#27977 = VERTEX_POINT ( 'NONE', #487 ) ;
#27978 = ORIENTED_EDGE ( 'NONE', *, *, #14964, .T. ) ;
#27979 = FACE_OUTER_BOUND ( 'NONE', #30405, .T. ) ;
#27980 = ORIENTED_EDGE ( 'NONE', *, *, #12873, .T. ) ;
#27981 = LINE ( 'NONE', #22029, #7228 ) ;
#27982 = CARTESIAN_POINT ( 'NONE',  ( -0.05562144613422675271, -0.4441896308501013246, -0.1229845283801413863 ) ) ;
#27983 = CARTESIAN_POINT ( 'NONE',  ( 0.5185199569154549382, -1.918301849770578604, 0.5182417262812423209 ) ) ;
#27985 = ORIENTED_EDGE ( 'NONE', *, *, #10652, .T. ) ;
#27984 = DIRECTION ( 'NONE',  ( -1.000000000000000000, -2.341930812374887555E-31, 1.664003471950578127E-31 ) ) ;
#27986 = CLOSED_SHELL ( 'NONE', ( #7443, #8990, #37655, #10265, #37928, #11260, #666, #34530, #31417, #39798, #3962, #34181, #16948, #1992, #3843, #22069, #1166, #24143 ) ) ;
#27987 = CIRCLE ( 'NONE', #3668, 0.2200000000000000566 ) ;
#27988 = ORIENTED_EDGE ( 'NONE', *, *, #30340, .F. ) ;
#27989 = FACE_OUTER_BOUND ( 'NONE', #24936, .T. ) ;
#27990 = ORIENTED_EDGE ( 'NONE', *, *, #29028, .F. ) ;
#27991 = CARTESIAN_POINT ( 'NONE',  ( -0.001323340259884761604, -0.5441669509461014576, 0.2330429837679495741 ) ) ;
#27993 = CARTESIAN_POINT ( 'NONE',  ( 0.09320273485841774896, -1.292715317639649308, 0.5862264040831728362 ) ) ;
#27992 = CARTESIAN_POINT ( 'NONE',  ( 0.4974655663051580357, -1.692079803311779873, -0.4360563182030788854 ) ) ;
#27994 = LOCAL_TIME ( 0, 53, 7.000000000000000000, #24446 ) ;
#27995 = APPLIED_PERSON_AND_ORGANIZATION_ASSIGNMENT ( #2129, #14663, ( #6983 ) ) ;
#27996 = CARTESIAN_POINT ( 'NONE',  ( 0.05999999999999990757, 0.4783370154475778957, 0.2940679337375899927 ) ) ;
#27997 = CARTESIAN_POINT ( 'NONE',  ( 0.4183807527607137922, -1.702160111122825059, -0.4180178025648325080 ) ) ;
#27999 = ORIENTED_EDGE ( 'NONE', *, *, #24063, .F. ) ;
#27998 = ORIENTED_EDGE ( 'NONE', *, *, #8168, .F. ) ;
#28000 = LINE ( 'NONE', #12552, #3392 ) ;
#28001 = AXIS2_PLACEMENT_3D ( 'NONE', #35293, #19466, #16181 ) ;
#28002 = CARTESIAN_POINT ( 'NONE',  ( 0.4022495603007555931, -1.747046214996282432, -0.4499298451809822796 ) ) ;
#28003 = PERSON ( 'NAUO-PER2', 'UNSPECIFIED', 'UNSPECIFIED', ('UNSPECIFIED'), ('UNSPECIFIED'), ('UNSPECIFIED') ) ;
#28004 = CARTESIAN_POINT ( 'NONE',  ( -0.05634115714581228868, -0.4380405955734085199, 0.1368374331724208914 ) ) ;
#28005 = CARTESIAN_POINT ( 'NONE',  ( 0.4107868727942790010, -1.187545294887579095, 0.8166605323444690034 ) ) ;
#28006 =( BOUNDED_SURFACE ( )  B_SPLINE_SURFACE ( 3, 2, ( 
 ( #10526, #16116, #6607 ),
 ( #25776, #25989, #38295 ),
 ( #28655, #29044, #9914 ),
 ( #38513, #13019, #19406 ),
 ( #38096, #3330, #10126 ),
 ( #912, #22702, #25568 ),
 ( #16313, #22486, #35233 ),
 ( #35011, #4142, #6823 ),
 ( #31940, #7034, #10343 ),
 ( #19603, #22905, #32325 ),
 ( #16711, #36029, #14621 ),
 ( #17108, #13808, #26377 ),
 ( #38907, #16914, #11559 ),
 ( #26792, #26975, #20404 ),
 ( #39724, #7647, #4742 ),
 ( #23698, #4542, #20211 ),
 ( #10735, #24122, #36439 ),
 ( #32736, #36644, #32535 ),
 ( #20002, #39509, #4353 ),
 ( #23514, #1501, #20615 ),
 ( #1900, #23910, #36225 ),
 ( #14413, #14015, #7833 ),
 ( #29869, #11341, #17313 ),
 ( #29459, #39128, #1303 ),
 ( #39319, #1708, #27190 ),
 ( #23309, #8253, #29656 ),
 ( #35834, #26589, #10952 ),
 ( #32936, #14227, #11139 ),
 ( #8040, #33150, #20825 ),
 ( #4957, #17522, #30072 ),
 ( #33345, #5155, #17706 ),
 ( #30252, #2082, #12362 ),
 ( #33970, #25112, #2302 ),
 ( #40540, #8643, #40330 ),
 ( #17908, #8449, #5774 ),
 ( #15650, #39932, #2500 ),
 ( #33752, #2902, #21016 ),
 ( #28199, #63, #12555 ),
 ( #30473, #11748, #24306 ),
 ( #14843, #37042, #24918 ),
 ( #18328, #33534, #27406 ),
 ( #34155, #5344, #8864 ),
 ( #27590, #36830, #37445 ),
 ( #28005, #15042, #21217 ),
 ( #18128, #18525, #15237 ),
 ( #5566, #24511, #30874 ),
 ( #21443, #30683, #9256 ),
 ( #2692, #27796, #9070 ),
 ( #21834, #12161, #24724 ),
 ( #37253, #21633, #34362 ),
 ( #5966, #40117, #11947 ),
 ( #31081, #15453, #6176 ),
 ( #18745, #31297, #3107 ),
 ( #25329, #22444, #31486 ),
 ( #37654, #31897, #9685 ),
 ( #28998, #3717, #25530 ),
 ( #25723, #22250, #38254 ),
 ( #32279, #29211, #16457 ),
 ( #6571, #483, #19149 ),
 ( #12979, #1073, #22052 ),
 ( #19360, #32093, #31686 ),
 ( #37869, #16269, #9871 ),
 ( #28808, #34764, #9470 ),
 ( #38470, #16663, #13371 ),
 ( #862, #10084, #34972 ),
 ( #3293, #670, #22657 ) ),
 .UNSPECIFIED., .F., .F., .T. ) 
 B_SPLINE_SURFACE_WITH_KNOTS ( ( 4, 2, 2, 2, 2, 2, 2, 2, 2, 2, 2, 2, 2, 2, 2, 2, 2, 2, 2, 2, 2, 2, 2, 2, 2, 2, 2, 2, 2, 2, 2, 2, 4 ),
 ( 3, 3 ),
 ( 0.003862184171445387244, 0.004005911543370605475, 0.004077775229333214374, 0.004113707072314519257, 0.004149638915295824140, 0.004437093659146261471, 0.005012003146847136131, 0.006161822122248884585, 0.006736731609949758379, 0.007311641097650633039, 0.008461460073052382361, 0.01306073597465937618, 0.01421055495006112376, 0.01536037392546287308, 0.01651019290086462241, 0.01766001187626637173, 0.01995964982706986690, 0.02225928777787336554, 0.02340910675327511486, 0.02455892572867686419, 0.02685856367948035936, 0.02915820163028385453, 0.03145783958108735318, 0.03260765855648910250, 0.03375747753189084488, 0.03490729650729259420, 0.03605711548269434352, 0.03663202497039522165, 0.03720693445809609284, 0.03778184394579696403, 0.03835675343349784217, 0.03950657240889959149, 0.04065639138430134081 ),
 ( 0.000000000000000000, 1.000000000000000000 ),
 .UNSPECIFIED. ) 
 GEOMETRIC_REPRESENTATION_ITEM ( )  RATIONAL_B_SPLINE_SURFACE ( (
 ( 1.000000000000000000, 0.7659831817177167324, 1.000000000000000000),
 ( 1.000000000000000000, 0.7659831817177167324, 1.000000000000000000),
 ( 1.000000000000000000, 0.7659831817177171764, 1.000000000000000000),
 ( 1.000000000000000000, 0.7659831817177171764, 1.000000000000000000),
 ( 1.000000000000000000, 0.7659831817177167324, 1.000000000000000000),
 ( 1.000000000000000000, 0.7659831817177167324, 1.000000000000000000),
 ( 1.000000000000000000, 0.7659823156457327142, 1.000000000000000000),
 ( 1.000000000000000000, 0.7659781499614458644, 1.000000000000000000),
 ( 1.000000000000000000, 0.7659750002451379824, 1.000000000000000000),
 ( 1.000000000000000000, 0.7659380538139435313, 1.000000000000000000),
 ( 1.000000000000000000, 0.7658458401200891608, 1.000000000000000000),
 ( 1.000000000000000000, 0.7655236400952580844, 1.000000000000000000),
 ( 1.000000000000000000, 0.7652407285018256733, 1.000000000000000000),
 ( 1.000000000000000000, 0.7644032511843058542, 1.000000000000000000),
 ( 1.000000000000000000, 0.7639223851950867061, 1.000000000000000000),
 ( 1.000000000000000000, 0.7630220264715582568, 1.000000000000000000),
 ( 1.000000000000000000, 0.7627024615980096955, 1.000000000000000000),
 ( 1.000000000000000000, 0.7620247162771555116, 1.000000000000000000),
 ( 1.000000000000000000, 0.7616570060786606033, 1.000000000000000000),
 ( 1.000000000000000000, 0.7604379540530756820, 1.000000000000000000),
 ( 1.000000000000000000, 0.7595531301201857710, 1.000000000000000000),
 ( 1.000000000000000000, 0.7545224428441196229, 1.000000000000000000),
 ( 1.000000000000000000, 0.7493009569406670067, 1.000000000000000000),
 ( 1.000000000000000000, 0.7423160112036807368, 1.000000000000000000),
 ( 1.000000000000000000, 0.7409110957858757729, 1.000000000000000000),
 ( 1.000000000000000000, 0.7381237456055174118, 1.000000000000000000),
 ( 1.000000000000000000, 0.7367470398672157916, 1.000000000000000000),
 ( 1.000000000000000000, 0.7341806964246635481, 1.000000000000000000),
 ( 1.000000000000000000, 0.7329567133465884066, 1.000000000000000000),
 ( 1.000000000000000000, 0.7308089355666729237, 1.000000000000000000),
 ( 1.000000000000000000, 0.7298844137523633480, 1.000000000000000000),
 ( 1.000000000000000000, 0.7279463615642568497, 1.000000000000000000),
 ( 1.000000000000000000, 0.7277005349271021828, 1.000000000000000000),
 ( 1.000000000000000000, 0.7325814144033533371, 1.000000000000000000),
 ( 1.000000000000000000, 0.7379337678855741878, 1.000000000000000000),
 ( 1.000000000000000000, 0.7540011851016407141, 1.000000000000000000),
 ( 1.000000000000000000, 0.7607161262302054583, 1.000000000000000000),
 ( 1.000000000000000000, 0.7755360273599477550, 1.000000000000000000),
 ( 1.000000000000000000, 0.7835406870239474131, 1.000000000000000000),
 ( 1.000000000000000000, 0.8061417792357221668, 1.000000000000000000),
 ( 1.000000000000000000, 0.8187798214764351323, 1.000000000000000000),
 ( 1.000000000000000000, 0.8359312486381417218, 1.000000000000000000),
 ( 1.000000000000000000, 0.8408816577689636196, 1.000000000000000000),
 ( 1.000000000000000000, 0.8450128811913334426, 1.000000000000000000),
 ( 1.000000000000000000, 0.8442046636671193260, 1.000000000000000000),
 ( 1.000000000000000000, 0.8395230928915869972, 1.000000000000000000),
 ( 1.000000000000000000, 0.8373721201386176149, 1.000000000000000000),
 ( 1.000000000000000000, 0.8317843866040760537, 1.000000000000000000),
 ( 1.000000000000000000, 0.8283573055353494752, 1.000000000000000000),
 ( 1.000000000000000000, 0.8200239860571119088, 1.000000000000000000),
 ( 1.000000000000000000, 0.8150997353630367037, 1.000000000000000000),
 ( 1.000000000000000000, 0.8031390929375081811, 1.000000000000000000),
 ( 1.000000000000000000, 0.7961772277509610030, 1.000000000000000000),
 ( 1.000000000000000000, 0.7836509786413579093, 1.000000000000000000),
 ( 1.000000000000000000, 0.7791219561609438182, 1.000000000000000000),
 ( 1.000000000000000000, 0.7693659621982237296, 1.000000000000000000),
 ( 1.000000000000000000, 0.7641340825345092069, 1.000000000000000000),
 ( 1.000000000000000000, 0.7536989215030908129, 1.000000000000000000),
 ( 1.000000000000000000, 0.7484621702622018535, 1.000000000000000000),
 ( 1.000000000000000000, 0.7385966617950382451, 1.000000000000000000),
 ( 1.000000000000000000, 0.7339569418095627240, 1.000000000000000000),
 ( 1.000000000000000000, 0.7219887718280880717, 1.000000000000000000),
 ( 1.000000000000000000, 0.7165447210591409100, 1.000000000000000000),
 ( 1.000000000000000000, 0.7095247715316972403, 1.000000000000000000),
 ( 1.000000000000000000, 0.7079216154009045914, 1.000000000000000000),
 ( 1.000000000000000000, 0.7071730258920838619, 1.000000000000000000) ) ) 
 REPRESENTATION_ITEM ( '' )  SURFACE ( )  );
#28007 = CARTESIAN_POINT ( 'NONE',  ( 0.1633339118204678586, -0.8580491329167432291, 0.4791465288558531821 ) ) ;
#28008 = DIRECTION ( 'NONE',  ( 0.000000000000000000, 0.000000000000000000, -1.000000000000000000 ) ) ;
#28009 = CARTESIAN_POINT ( 'NONE',  ( 0.1032247015330990531, -0.8975257853914290207, 0.8793098326616880511 ) ) ;
#28010 = CARTESIAN_POINT ( 'NONE',  ( 0.05999999999999990757, 0.5209315849442416324, 0.3202538583802939098 ) ) ;
#28011 = CARTESIAN_POINT ( 'NONE',  ( 0.7472019744968698696, -1.513150647243692637, 0.5707417262808793801 ) ) ;
#28012 = EDGE_CURVE ( 'NONE', #33041, #40153, #8790, .T. ) ;
#28013 = DIRECTION ( 'NONE',  ( 0.4999551463232373427, -0.8660512985181134660, 0.000000000000000000 ) ) ;
#28014 = CARTESIAN_POINT ( 'NONE',  ( 5.463695987328526437E-16, -0.2899999999999993694, -7.171100983368691195E-16 ) ) ;
#28015 =( NAMED_UNIT ( * ) PLANE_ANGLE_UNIT ( ) SI_UNIT ( $, .RADIAN. ) );
#28016 = CIRCLE ( 'NONE', #18825, 0.1849999999999994982 ) ;
#28017 = CARTESIAN_POINT ( 'NONE',  ( 0.02881408050861827136, -0.2420347005671091012, 0.4354489374660209244 ) ) ;
#28018 = EDGE_CURVE ( 'NONE', #21667, #3878, #18605, .T. ) ;
#28019 = CARTESIAN_POINT ( 'NONE',  ( 0.002083146443013504916, -0.4777046557262296100, 0.1457185332388684640 ) ) ;
#28020 = CARTESIAN_POINT ( 'NONE',  ( 0.09334160340306593695, -1.332730469180070765, 0.7045675880059063534 ) ) ;
#28021 = EDGE_CURVE ( 'NONE', #14789, #37239, #6388, .T. ) ;
#28022 = CALENDAR_DATE ( 2026, 13, 10 ) ;
#28023 = CARTESIAN_POINT ( 'NONE',  ( 0.4627885704097156050, -1.051432690887019072, 0.8329284434066291931 ) ) ;
#28024 = APPLIED_APPROVAL_ASSIGNMENT ( #2358, ( #39812 ) ) ;
#28025 = EDGE_CURVE ( 'NONE', #38731, #27338, #28900, .T. ) ;
#28026 = DIRECTION ( 'NONE',  ( 0.4261641068392729714, 0.9046458721742364206, 0.000000000000000000 ) ) ;
#28027 = EDGE_CURVE ( 'NONE', #36736, #17902, #39625, .T. ) ;
#28028 = FACE_OUTER_BOUND ( 'NONE', #17577, .T. ) ;
#28029 = EDGE_CURVE ( 'NONE', #4635, #35563, #16274, .T. ) ;
#28030 = VECTOR ( 'NONE', #4596, 39.37007874015748143 ) ;
#28031 = CARTESIAN_POINT ( 'NONE',  ( 0.05634301242525744519, -0.2780425975185431553, 0.3652000572937675882 ) ) ;
#28032 = EDGE_LOOP ( 'NONE', ( #30600, #7541, #27437, #14348 ) ) ;
#28033 = LINE ( 'NONE', #30896, #164 ) ;
#28034 = VERTEX_POINT ( 'NONE', #38859 ) ;
#28035 = CARTESIAN_POINT ( 'NONE',  ( -0.2399999999999999079, -4.289222312108804225, -0.5708809693675255259 ) ) ;
#28036 = CARTESIAN_POINT ( 'NONE',  ( 0.1995336070936418182, -1.402089414342744700, 0.9384260727155151471 ) ) ;
#28037 = CARTESIAN_POINT ( 'NONE',  ( 0.5877737341208254529, -1.491194589871079001, 0.5703655673359632194 ) ) ;
#28039 = ORIENTED_EDGE ( 'NONE', *, *, #34780, .T. ) ;
#28038 = CARTESIAN_POINT ( 'NONE',  ( -0.3000000000000000999, -3.941790907013290823, -0.4709369376873030477 ) ) ;
#28040 = CARTESIAN_POINT ( 'NONE',  ( 0.4795791402848185725, -1.087578995800233095, 0.7487995513514865698 ) ) ;
#28042 = ORIENTED_EDGE ( 'NONE', *, *, #17915, .F. ) ;
#28041 = ORIENTED_EDGE ( 'NONE', *, *, #24305, .F. ) ;
#28043 = CARTESIAN_POINT ( 'NONE',  ( 0.6988918244707941207, -1.438898845315309094, 0.5752146833678662974 ) ) ;
#28044 = CARTESIAN_POINT ( 'NONE',  ( 0.3396305973613506501, -1.637478036087311350, -0.5914524579777636903 ) ) ;
#28045 = EDGE_CURVE ( 'NONE', #19865, #4879, #35791, .T. ) ;
#28046 = APPLIED_PERSON_AND_ORGANIZATION_ASSIGNMENT ( #16234, #22008, ( #26625 ) ) ;
#28047 = CARTESIAN_POINT ( 'NONE',  ( 0.4588468109159730135, -1.044667397767246708, -0.4248180574663139586 ) ) ;
#28048 = APPROVAL_DATE_TIME ( #13198, #2358 ) ;
#28049 = CARTESIAN_POINT ( 'NONE',  ( -0.2136509456379324934, -0.4946207598421927254, 0.08499999999999977018 ) ) ;
#28050 = B_SPLINE_CURVE_WITH_KNOTS ( 'NONE', 3,
 ( #25595, #15917, #25805, #10364 ),
 .UNSPECIFIED., .F., .F.,
 ( 4, 4 ),
 ( 5.485677294651091042E-18, 0.003354154147083482796 ),
 .UNSPECIFIED. ) ;
#28051 = ORIENTED_EDGE ( 'NONE', *, *, #19064, .T. ) ;
#28052 = CARTESIAN_POINT ( 'NONE',  ( 0.1357061440364132343, -0.8234802076881400090, 0.4864660559418247376 ) ) ;
#28053 = CARTESIAN_POINT ( 'NONE',  ( 0.1909286924077255032, -1.257064795538239022, -0.5931747813493344346 ) ) ;
#28054 = CARTESIAN_POINT ( 'NONE',  ( 0.4899971463290487828, -1.463357359739534846, 0.7777802213075096782 ) ) ;
#28056 = CARTESIAN_POINT ( 'NONE',  ( 0.0007905216470313744179, -0.6035600366138994533, 4.286223126101739974E-05 ) ) ;
#28055 = CARTESIAN_POINT ( 'NONE',  ( 0.3320566521985225950, -1.758475802836519941, 0.4740614269747379095 ) ) ;
#28057 = DIRECTION ( 'NONE',  ( -1.000000000000000000, -0.000000000000000000, -0.000000000000000000 ) ) ;
#28058 = APPLIED_SECURITY_CLASSIFICATION_ASSIGNMENT ( #18145, ( #40658 ) ) ;
#28059 = ORIENTED_EDGE ( 'NONE', *, *, #4205, .F. ) ;
#28060 = CARTESIAN_POINT ( 'NONE',  ( 0.4175465041423866430, -1.703516643873120184, 0.6086626662040888203 ) ) ;
#28061 = CARTESIAN_POINT ( 'NONE',  ( 0.6811486575909255770, -1.402667997544871037, 0.7201154234290257916 ) ) ;
#28062 = AXIS2_PLACEMENT_3D ( 'NONE', #20308, #17417, #39417 ) ;
#28063 = CARTESIAN_POINT ( 'NONE',  ( 0.3784855106043947814, -1.091058466892998347, -0.5155029497116575543 ) ) ;
#28064 = DIRECTION ( 'NONE',  ( -7.000205099780314469E-17, -1.000000000000000000, 6.590151126658399604E-16 ) ) ;
#28065 = CARTESIAN_POINT ( 'NONE',  ( 0.4000062018654670370, -1.149314450333016380, 0.4182417262808721947 ) ) ;
#28066 = DIRECTION ( 'NONE',  ( 1.000000000000000000, 6.779273404243070203E-32, 4.314083075427408311E-32 ) ) ;
#28067 = CARTESIAN_POINT ( 'NONE',  ( 0.3466030059118228035, -1.167433418478718510, 0.4480105783002163444 ) ) ;
#28068 = CARTESIAN_POINT ( 'NONE',  ( 0.4384178598954188155, -1.040563892421024983, 0.6900182345289431751 ) ) ;
#28069 = EDGE_CURVE ( 'NONE', #30141, #31025, #34373, .T. ) ;
#28070 = DATE_TIME_ROLE ( 'creation_date' ) ;
#28071 = CARTESIAN_POINT ( 'NONE',  ( 0.4704749616853449168, -1.069673565160275341, -0.4234913399341371787 ) ) ;
#28072 = EDGE_CURVE ( 'NONE', #35465, #4497, #13235, .T. ) ;
#28073 = AXIS2_PLACEMENT_3D ( 'NONE', #38074, #10322, #7397 ) ;
#28074 = CARTESIAN_POINT ( 'NONE',  ( 0.4901745208690559408, -1.545214605713521205, 0.5488368183266709721 ) ) ;
#28075 = EDGE_CURVE ( 'NONE', #25550, #14915, #17283, .T. ) ;
#28076 = CARTESIAN_POINT ( 'NONE',  ( -0.05491348488830684327, 0.02524042857556436925, 0.4620240554957945056 ) ) ;
#28077 = ORIENTED_EDGE ( 'NONE', *, *, #28522, .F. ) ;
#28078 = CARTESIAN_POINT ( 'NONE',  ( 0.4676597105902504659, -1.237282431096226043, 0.6057417262810000924 ) ) ;
#28079 = DIRECTION ( 'NONE',  ( 1.000000000000000000, 0.000000000000000000, 0.000000000000000000 ) ) ;
#28080 = B_SPLINE_CURVE_WITH_KNOTS ( 'NONE', 3,
 ( #17635, #30182, #39636, #2419 ),
 .UNSPECIFIED., .F., .F.,
 ( 4, 4 ),
 ( 0.000000000000000000, 0.0002675641918131738258 ),
 .UNSPECIFIED. ) ;
#28081 = CARTESIAN_POINT ( 'NONE',  ( -0.2399999999999999079, -4.218511633990150500, -0.6415916474861803609 ) ) ;
#28082 = ORIENTED_EDGE ( 'NONE', *, *, #10795, .T. ) ;
#28083 = CARTESIAN_POINT ( 'NONE',  ( -0.04947837552028403613, -0.03507397079374865306, -0.4759739487165542404 ) ) ;
#28084 = CARTESIAN_POINT ( 'NONE',  ( 0.08250975870084176211, -1.108734649457161270, 0.7537977879433896966 ) ) ;
#28086 = ORIENTED_EDGE ( 'NONE', *, *, #10798, .F. ) ;
#28085 = ORIENTED_EDGE ( 'NONE', *, *, #32338, .T. ) ;
#28087 = CARTESIAN_POINT ( 'NONE',  ( 0.3135347772105874231, -1.762222029724279881, 0.5682242226546108110 ) ) ;
#28088 = DIRECTION ( 'NONE',  ( 7.771561172376107616E-16, -7.170354002788761615E-17, 1.000000000000000000 ) ) ;
#28089 = EDGE_CURVE ( 'NONE', #26082, #38131, #37628, .T. ) ;
#28090 = CARTESIAN_POINT ( 'NONE',  ( 0.3607657536367212536, -1.946668260980969345, -0.3283241642772302127 ) ) ;
#28091 = CARTESIAN_POINT ( 'NONE',  ( -0.05464101615137795936, -1.598492537578166672, -0.1971380022280825872 ) ) ;
#28093 = CARTESIAN_POINT ( 'NONE',  ( 0.5073704149278759346, -1.163922025721008557, 0.5182417262812423209 ) ) ;
#28092 = CARTESIAN_POINT ( 'NONE',  ( 0.05634115714581289930, 0.4380405955734021362, 0.1368374331724312720 ) ) ;
#28094 = CARTESIAN_POINT ( 'NONE',  ( 0.05634402396114377570, -0.2613837787620673092, -0.3773006586902102888 ) ) ;
#28095 = ORIENTED_EDGE ( 'NONE', *, *, #24402, .T. ) ;
#28096 = CARTESIAN_POINT ( 'NONE',  ( 0.1174566253694137585, -0.6744780707208714032, 0.4348850488351332921 ) ) ;
#28097 = ORIENTED_EDGE ( 'NONE', *, *, #17686, .T. ) ;
#28098 = FACE_OUTER_BOUND ( 'NONE', #40415, .T. ) ;
#28099 = CARTESIAN_POINT ( 'NONE',  ( 0.4717667268771776334, -1.556274250605339082, 0.6275438343556190013 ) ) ;
#28101 = CARTESIAN_POINT ( 'NONE',  ( 0.5730681724893124107, -1.614269927704049978, 0.5633518820464606947 ) ) ;
#28100 = CARTESIAN_POINT ( 'NONE',  ( 0.6699292074404794572, -1.569526485364059143, 0.6071573546319902759 ) ) ;
#28102 = CARTESIAN_POINT ( 'NONE',  ( 0.3969700875656382300, -1.750093955434189663, -0.5306525527942058673 ) ) ;
#28103 = PLANE ( 'NONE',  #25763 ) ;
#28104 = DIRECTION ( 'NONE',  ( 0.4747798520620566398, 0.000000000000000000, 0.8801045915548512122 ) ) ;
#28105 = CARTESIAN_POINT ( 'NONE',  ( 0.3940832238624992767, -1.985670795305536140, -0.2899752743292205448 ) ) ;
#28106 = CARTESIAN_POINT ( 'NONE',  ( 0.1252372108451314248, -0.5576925373213490467, 0.1984031368276146234 ) ) ;
#28107 = CARTESIAN_POINT ( 'NONE',  ( 0.4503334983497291888, -1.681198024010658543, 0.4342754154380044640 ) ) ;
#28108 = CARTESIAN_POINT ( 'NONE',  ( -0.04211471441534295201, 0.2826022563027020817, -0.3743350969764919212 ) ) ;
#28109 = CARTESIAN_POINT ( 'NONE',  ( -0.2746410161513782033, -2.183180860297908144, -0.4937760292030871079 ) ) ;
#28110 = CARTESIAN_POINT ( 'NONE',  ( 0.6672263256168233791, -1.559577713309469038, 0.6159734170043378310 ) ) ;
#28111 = CARTESIAN_POINT ( 'NONE',  ( 0.1784968570797965948, -1.218054820023663831, -0.5155029497116575543 ) ) ;
#28112 = CARTESIAN_POINT ( 'NONE',  ( -0.2399999999999999079, -4.250025578259899461, -0.8852376261118949374 ) ) ;
#28113 = CARTESIAN_POINT ( 'NONE',  ( 0.1896879205916190136, -0.5058468364965200692, 0.1731371019803292222 ) ) ;
#28114 = CARTESIAN_POINT ( 'NONE',  ( -0.03171102739523045527, 0.3312744048890978177, 0.3635303745205920589 ) ) ;
#28115 = CARTESIAN_POINT ( 'NONE',  ( 0.01511362640256554493, -1.029621820521785525, 0.5875183992405329514 ) ) ;
#28116 = ADVANCED_FACE ( 'NONE', ( #16879 ), #1459, .T. ) ;
#28117 = CARTESIAN_POINT ( 'NONE',  ( 0.6618556493260480122, -1.443346534042697638, -0.4155153992717031675 ) ) ;
#28118 = CARTESIAN_POINT ( 'NONE',  ( 0.3903407250317349475, -1.765467622026976491, -0.4499573014716374830 ) ) ;
#28119 = DIRECTION ( 'NONE',  ( 0.8660512985181135770, 0.4999551463232370652, -1.983296656985675225E-15 ) ) ;
#28120 = DIRECTION ( 'NONE',  ( -1.387778780781449620E-15, 6.590151126658376924E-16, -1.000000000000000000 ) ) ;
#28121 = B_SPLINE_CURVE_WITH_KNOTS ( 'NONE', 3,
 ( #9583, #19049, #31584, #32950, #34674, #16726, #32747, #1314, #13629, #4753, #22160, #25438, #9779, #7844, #6481, #6681, #23325, #3403, #22350, #29272, #19256, #31798, #28295, #26194, #4159, #38918, #35636, #15959, #165, #1124, #38718, #20018, #28504, #380, #20416, #10750, #23525, #12655, #29669, #10540, #23111, #32547, #4367, #12880, #16926, #29470, #10965, #14029, #13821, #26391, #35846, #7658, #20226, #4552 ),
 .UNSPECIFIED., .F., .F.,
 ( 4, 2, 2, 2, 2, 2, 2, 2, 2, 2, 2, 2, 2, 2, 2, 2, 2, 2, 2, 2, 2, 2, 2, 2, 2, 2, 4 ),
 ( -5.999999999642378183E-08, 0.0001480793356628742755, 0.0002962186713257449421, 0.0005924973426514890942, 0.001185054685302977615, 0.002370169370605954440, 0.003555284055908931699, 0.004740398741211909392, 0.009480857482423813223, 0.01185108685302976687, 0.01303620153833274717, 0.01422131622363572399, 0.01896177496484765038, 0.02133200433545361097, 0.02370223370605956809, 0.02607246307666552174, 0.02844269244727147886, 0.02962780713257446782, 0.03081292181787745679, 0.03199803650318044229, 0.03318315118848343126, 0.03436826587378641329, 0.03496082321643790430, 0.03555338055908939532, 0.03614593790174088633, 0.03673849524439237735, 0.03792360992969536632 ),
 .UNSPECIFIED. ) ;
#28122 = DIRECTION ( 'NONE',  ( 1.000000000000000000, 0.000000000000000000, 0.000000000000000000 ) ) ;
#28123 = ORIENTED_EDGE ( 'NONE', *, *, #32364, .F. ) ;
#28124 = EDGE_CURVE ( 'NONE', #29632, #4981, #6114, .T. ) ;
#28125 = DIRECTION ( 'NONE',  ( 8.881784197001246407E-16, -2.361472542561082612E-16, 1.000000000000000000 ) ) ;
#28126 = CARTESIAN_POINT ( 'NONE',  ( 0.4813244371982610681, -1.269896034304244248, 0.7940112196239507147 ) ) ;
#28127 = CARTESIAN_POINT ( 'NONE',  ( -0.2746410161513779258, -2.761122741982423801, -0.2878817176880067996 ) ) ;
#28128 = CARTESIAN_POINT ( 'NONE',  ( 0.5368080558625972776, -1.632053713898605984, -0.4360733739357021133 ) ) ;
#28129 = CARTESIAN_POINT ( 'NONE',  ( 0.4195420834447322611, -1.713617687370894593, 0.6096044365181384483 ) ) ;
#28130 = ORIENTED_EDGE ( 'NONE', *, *, #9139, .T. ) ;
#28131 = CARTESIAN_POINT ( 'NONE',  ( 0.5360939587443181997, -1.669780357970381601, -0.5511600881812523944 ) ) ;
#28132 = CARTESIAN_POINT ( 'NONE',  ( 0.2952349374191504672, -1.312115508766679817, 0.5179655188836596036 ) ) ;
#28133 = CARTESIAN_POINT ( 'NONE',  ( 0.07779920321647403048, -1.322114474344633583, 0.5682417262808776570 ) ) ;
#28134 = EDGE_CURVE ( 'NONE', #25255, #3822, #12730, .T. ) ;
#28135 = CARTESIAN_POINT ( 'NONE',  ( 0.04308558661661724548, 0.2425983775171377810, -0.4306836113028226776 ) ) ;
#28136 = CARTESIAN_POINT ( 'NONE',  ( 0.5003935287345969707, -1.293448292103240638, 0.6068886689937365020 ) ) ;
#28138 = ORIENTED_EDGE ( 'NONE', *, *, #1522, .T. ) ;
#28137 = LINE ( 'NONE', #2, #35121 ) ;
#28139 = CARTESIAN_POINT ( 'NONE',  ( 0.5099336548069899333, -1.112575729146672243, 0.5993070616419141627 ) ) ;
#28140 = ORIENTED_EDGE ( 'NONE', *, *, #7614, .F. ) ;
#28141 = ADVANCED_FACE ( 'NONE', ( #36185 ), #23210, .T. ) ;
#28142 = APPLICATION_PROTOCOL_DEFINITION ( 'international standard', 'automotive_design', 2000, #30042 ) ;
#28143 = CARTESIAN_POINT ( 'NONE',  ( -0.01736481776669303659, -0.6872203660140440151, 0.1457185332388702681 ) ) ;
#28144 = ORIENTED_EDGE ( 'NONE', *, *, #26043, .F. ) ;
#28145 = CARTESIAN_POINT ( 'NONE',  ( 0.3853064297010572736, -1.605638540110655210, 0.5751012791866177976 ) ) ;
#28147 = CARTESIAN_POINT ( 'NONE',  ( 0.1867164799886507631, -0.6336341480852951680, -0.01319825145230188283 ) ) ;
#28146 = CARTESIAN_POINT ( 'NONE',  ( 0.1499999999999997724, 0.2306506793134120714, 0.4716198300880287131 ) ) ;
#28148 = CARTESIAN_POINT ( 'NONE',  ( -0.02000000000000000042, -2.253856486606507836, -0.7252438489935795207 ) ) ;
#28149 = ORIENTED_EDGE ( 'NONE', *, *, #32895, .T. ) ;
#28150 = ORIENTED_EDGE ( 'NONE', *, *, #15801, .T. ) ;
#28151 = ORIENTED_EDGE ( 'NONE', *, *, #19687, .F. ) ;
#28152 = CARTESIAN_POINT ( 'NONE',  ( 0.4367293978554446787, -1.042335339574861131, 0.6370487242724790500 ) ) ;
#28153 = CARTESIAN_POINT ( 'NONE',  ( 0.1178863413097692436, -0.5755085003802594690, 0.2594340787492229183 ) ) ;
#28154 = ORIENTED_EDGE ( 'NONE', *, *, #31822, .F. ) ;
#28155 = CARTESIAN_POINT ( 'NONE',  ( 0.1357105165892663889, -2.107936428766272741, -0.2870436526301869407 ) ) ;
#28156 = CARTESIAN_POINT ( 'NONE',  ( -0.01548846960707531660, -0.3772621329472692908, -0.3651003739303438911 ) ) ;
#28157 = CARTESIAN_POINT ( 'NONE',  ( 0.5810193296476801050, -1.554241992011831996, -0.4294310414331839465 ) ) ;
#28158 = CARTESIAN_POINT ( 'NONE',  ( 0.1176733790823393522, -1.298938889880303371, 0.5182417262812425429 ) ) ;
#28159 = CARTESIAN_POINT ( 'NONE',  ( 0.4419048264407517412, -1.686280600454952205, 0.4284299735157269251 ) ) ;
#28160 = CARTESIAN_POINT ( 'NONE',  ( 0.4000099798367660608, -1.704638381955401183, 0.4182417262808776903 ) ) ;
#28161 = CARTESIAN_POINT ( 'NONE',  ( 0.2208526919740124717, -1.239328936468657272, 0.5723503595998229443 ) ) ;
#28162 = ORIENTED_EDGE ( 'NONE', *, *, #27341, .F. ) ;
#28163 = CARTESIAN_POINT ( 'NONE',  ( 0.2569741121304622844, -1.653347272235380361, -0.6637523221072149093 ) ) ;
#28164 = CARTESIAN_POINT ( 'NONE',  ( -0.08000000000000000167, -1.659335422034822205, 0.2169804935274543545 ) ) ;
#28165 = CALENDAR_DATE ( 2026, 13, 10 ) ;
#28166 = EDGE_CURVE ( 'NONE', #4225, #16603, #33102, .T. ) ;
#28167 = CARTESIAN_POINT ( 'NONE',  ( 0.2159838750730762591, -0.9307556585230835067, 0.3864363914520806964 ) ) ;
#28168 = LINE ( 'NONE', #3677, #7505 ) ;
#28169 = CARTESIAN_POINT ( 'NONE',  ( 0.4538010422723244286, -1.220679807276677575, 0.6057417262810179670 ) ) ;
#28170 = CARTESIAN_POINT ( 'NONE',  ( 0.3167162826948920484, -1.173191636801490745, 0.5491094731419751129 ) ) ;
#28171 = CARTESIAN_POINT ( 'NONE',  ( 0.1224152969000399382, -1.440949543414774547, 0.5682417262808782121 ) ) ;
#28172 = CARTESIAN_POINT ( 'NONE',  ( 0.2615594559960963683, -1.678060962790617783, 0.5376464678218270121 ) ) ;
#28173 = FACE_OUTER_BOUND ( 'NONE', #13263, .T. ) ;
#28174 = CARTESIAN_POINT ( 'NONE',  ( 0.3508778134978967067, -1.164926840218082127, 0.4278213320778186390 ) ) ;
#28175 = VERTEX_POINT ( 'NONE', #2463 ) ;
#28176 = ORIENTED_EDGE ( 'NONE', *, *, #33145, .F. ) ;
#28177 = FACE_OUTER_BOUND ( 'NONE', #11128, .T. ) ;
#28178 = ORIENTED_EDGE ( 'NONE', *, *, #23744, .T. ) ;
#28179 = CARTESIAN_POINT ( 'NONE',  ( 0.2616322387702281205, -1.678013124025769187, 0.5382687897764735219 ) ) ;
#28180 = CARTESIAN_POINT ( 'NONE',  ( -0.02953079040095707777, -0.5250338024619269905, -0.07436286310882420092 ) ) ;
#28181 = CARTESIAN_POINT ( 'NONE',  ( 0.5767892224792289246, -1.425666411081258467, 0.6016736859548048599 ) ) ;
#28183 = ORIENTED_EDGE ( 'NONE', *, *, #16729, .T. ) ;
#28182 = CARTESIAN_POINT ( 'NONE',  ( 0.1499999999999993561, 0.000000000000000000, 0.000000000000000000 ) ) ;
#28184 = VERTEX_POINT ( 'NONE', #11299 ) ;
#28185 = CARTESIAN_POINT ( 'NONE',  ( 0.000000000000000000, 0.000000000000000000, 0.000000000000000000 ) ) ;
#28186 = ORIENTED_EDGE ( 'NONE', *, *, #447, .T. ) ;
#28187 = CARTESIAN_POINT ( 'NONE',  ( 0.2974677162926867013, -1.656770836169560335, 0.5772130710687483068 ) ) ;
#28189 = CARTESIAN_POINT ( 'NONE',  ( 0.4440535265307390955, -1.714300051848237638, 0.5182417262812423209 ) ) ;
#28188 = CARTESIAN_POINT ( 'NONE',  ( 0.5136163779962517051, -1.682756243106886318, -0.4473473194278146936 ) ) ;
#28190 = CARTESIAN_POINT ( 'NONE',  ( -1.040834085586084010E-16, 4.942613344993767655E-17, -0.07499999999999977518 ) ) ;
#28191 = EDGE_CURVE ( 'NONE', #12748, #13839, #13349, .T. ) ;
#28192 = CARTESIAN_POINT ( 'NONE',  ( -0.1157923916715135615, -0.5295015842443983045, 0.3181161673586299643 ) ) ;
#28194 = ORIENTED_EDGE ( 'NONE', *, *, #38083, .F. ) ;
#28193 = VERTEX_POINT ( 'NONE', #33493 ) ;
#28195 = B_SPLINE_CURVE_WITH_KNOTS ( 'NONE', 3,
 ( #17897, #39500, #11331, #33335, #5335, #33138, #30464, #15031, #33526, #8030, #8241, #24112, #17304, #23690 ),
 .UNSPECIFIED., .F., .F.,
 ( 4, 2, 2, 2, 2, 2, 4 ),
 ( 0.000000000000000000, 0.001093382690672758516, 0.001640074036009137558, 0.002186765381345516599, 0.002733456726681895640, 0.003280148072018274682, 0.004373530762691031464 ),
 .UNSPECIFIED. ) ;
#28196 = DIRECTION ( 'NONE',  ( -0.7173209392562553965, -0.6967428969270202943, -7.540734276611761816E-05 ) ) ;
#28197 = CARTESIAN_POINT ( 'NONE',  ( 0.3984114568195522010, -1.599003643269838904, -0.5155029497116575543 ) ) ;
#28198 = CARTESIAN_POINT ( 'NONE',  ( -0.05616044724337241473, -0.4336395721329119879, 0.1516614036261227927 ) ) ;
#28199 = CARTESIAN_POINT ( 'NONE',  ( 0.2721784717217399230, -0.9829408826315968462, 0.7561764537945854237 ) ) ;
#28200 = CARTESIAN_POINT ( 'NONE',  ( 0.3444280284632370015, -1.101336781896232075, 0.7393691862850351182 ) ) ;
#28201 = CARTESIAN_POINT ( 'NONE',  ( 0.2734857512113577083, -1.671572137726918816, 0.6513199796913040629 ) ) ;
#28202 = CARTESIAN_POINT ( 'NONE',  ( 0.3202835734604576046, -1.704999925949175710, 0.8356439209704767945 ) ) ;
#28203 = DIRECTION ( 'NONE',  ( 0.000000000000000000, 1.000000000000000000, -1.224646799147353207E-16 ) ) ;
#28204 = DIRECTION ( 'NONE',  ( -0.6967428928481391726, 0.7173209432181241185, -7.540734276603101752E-05 ) ) ;
#28205 = DIRECTION ( 'NONE',  ( 7.000205099780496893E-17, 1.000000000000000000, 6.590151126658374952E-16 ) ) ;
#28206 = DIRECTION ( 'NONE',  ( 0.000000000000000000, 0.2751755752258863152, 0.9613939893712164508 ) ) ;
#28207 = DIRECTION ( 'NONE',  ( 1.215715279674078196E-17, 0.5890747513118477219, -0.8080785465329993755 ) ) ;
#28208 = CARTESIAN_POINT ( 'NONE',  ( 0.05201840200955108739, -0.2617120493658864344, 0.3909676859878761790 ) ) ;
#28209 = DIRECTION ( 'NONE',  ( 8.881784197001246407E-16, -2.361472542561082612E-16, 1.000000000000000000 ) ) ;
#28210 = CARTESIAN_POINT ( 'NONE',  ( 0.1019768089910752101, -1.315145345007704192, 0.7228722810749433902 ) ) ;
#28211 = CALENDAR_DATE ( 2026, 13, 10 ) ;
#28212 = CARTESIAN_POINT ( 'NONE',  ( 0.6347819612394876021, -1.328236395719069263, 0.8269854195084552773 ) ) ;
#28213 = CARTESIAN_POINT ( 'NONE',  ( -0.02238826743733216343, 0.4611641377668438957, 0.2234181651772507715 ) ) ;
#28214 = CARTESIAN_POINT ( 'NONE',  ( 0.6727416549544570357, -1.556482965640024974, 0.6140251777818144241 ) ) ;
#28215 = CARTESIAN_POINT ( 'NONE',  ( -0.2399999999999999079, -2.183180860297908144, -0.3591170932241134484 ) ) ;
#28216 = FACE_OUTER_BOUND ( 'NONE', #21806, .T. ) ;
#28217 = ORIENTED_EDGE ( 'NONE', *, *, #14499, .F. ) ;
#28218 = CARTESIAN_POINT ( 'NONE',  ( 0.4623247243936773332, -1.147348113996353502, -0.6255478604071451620 ) ) ;
#28219 = CARTESIAN_POINT ( 'NONE',  ( 0.2559586117443874986, -1.601769494230190327, 0.8408691708661252262 ) ) ;
#28220 = CARTESIAN_POINT ( 'NONE',  ( 0.5875213160827347236, -1.472591613620396922, 0.6829739459387013101 ) ) ;
#28222 = ORIENTED_EDGE ( 'NONE', *, *, #30439, .F. ) ;
#28221 = DIRECTION ( 'NONE',  ( -0.3468893892380667254, -0.2594111197898709698, 0.9013177145509825294 ) ) ;
#28223 = CARTESIAN_POINT ( 'NONE',  ( 0.2139922239084591227, -0.7322259512090013578, 0.4012976140435131622 ) ) ;
#28225 = ORIENTED_EDGE ( 'NONE', *, *, #25869, .F. ) ;
#28224 = EDGE_LOOP ( 'NONE', ( #9205, #25814, #15981, #4040 ) ) ;
#28226 = DIRECTION ( 'NONE',  ( -1.000000000000000000, -2.280301054154495132E-31, 1.664003471950577689E-31 ) ) ;
#28227 =( BOUNDED_SURFACE ( )  B_SPLINE_SURFACE ( 3, 2, ( 
 ( #22560, #6687, #32394 ),
 ( #4218, #25444, #7087 ),
 ( #34880, #25848, #28511 ),
 ( #1178, #6895, #38366 ),
 ( #35477, #22958, #10593 ),
 ( #9990, #16183, #28725 ),
 ( #976, #7498, #388 ),
 ( #16368, #20077, #37975 ),
 ( #13677, #9785, #13491 ),
 ( #22356, #26055, #586 ),
 ( #13079, #28907, #10205 ),
 ( #26239, #25635, #19657 ),
 ( #35091, #19468, #32001 ),
 ( #22771, #35295, #32193 ),
 ( #7282, #4007, #16571 ),
 ( #38576, #19859, #16784 ),
 ( #4598, #11205, #30135 ),
 ( #36094, #27050, #23772 ) ),
 .UNSPECIFIED., .F., .F., .T. ) 
 B_SPLINE_SURFACE_WITH_KNOTS ( ( 4, 2, 2, 2, 2, 2, 2, 2, 4 ),
 ( 3, 3 ),
 ( -0.001532620576208853364, -0.0007637936630077653581, 5.033250193322647351E-06, 0.0007738601633944106528, 0.001542687076595498658, 0.002311513989796586989, 0.003080340902997674886, 0.003849167816198762783, 0.004617994729399850680 ),
 ( 0.000000000000000000, 1.000000000000000000 ),
 .UNSPECIFIED. ) 
 GEOMETRIC_REPRESENTATION_ITEM ( )  RATIONAL_B_SPLINE_SURFACE ( (
 ( 1.000000000000000000, 0.7283825911960453148, 1.000000000000000000),
 ( 1.000000000000000000, 0.7404385082113110750, 1.000000000000000000),
 ( 1.000000000000000000, 0.7521504257739634047, 1.000000000000000000),
 ( 1.000000000000000000, 0.7744497410760246003, 1.000000000000000000),
 ( 1.000000000000000000, 0.7845654757373008437, 1.000000000000000000),
 ( 1.000000000000000000, 0.8022083990893182914, 1.000000000000000000),
 ( 1.000000000000000000, 0.8094167424698777147, 1.000000000000000000),
 ( 1.000000000000000000, 0.8194491993617203374, 1.000000000000000000),
 ( 1.000000000000000000, 0.8220634900780806609, 1.000000000000000000),
 ( 1.000000000000000000, 0.8220705070823161043, 1.000000000000000000),
 ( 1.000000000000000000, 0.8194468812482857967, 1.000000000000000000),
 ( 1.000000000000000000, 0.8094220769837565665, 1.000000000000000000),
 ( 1.000000000000000000, 0.8022659121984583308, 1.000000000000000000),
 ( 1.000000000000000000, 0.7845681159036421715, 1.000000000000000000),
 ( 1.000000000000000000, 0.7744426415184756385, 1.000000000000000000),
 ( 1.000000000000000000, 0.7522890290929223900, 1.000000000000000000),
 ( 1.000000000000000000, 0.7403540167214975876, 1.000000000000000000),
 ( 1.000000000000000000, 0.7283825911960206678, 1.000000000000000000) ) ) 
 REPRESENTATION_ITEM ( '' )  SURFACE ( )  );
#28228 = CARTESIAN_POINT ( 'NONE',  ( -0.2746410161513776482, -3.849534981189179028, -0.1910928155360645808 ) ) ;
#28229 = DIRECTION ( 'NONE',  ( -1.000000000000000000, -0.000000000000000000, -0.000000000000000000 ) ) ;
#28230 = DATE_AND_TIME ( #6602, #2380 ) ;
#28231 = CARTESIAN_POINT ( 'NONE',  ( -0.2399999999999999079, -2.154189217240303655, -0.3012881438978375903 ) ) ;
#28232 = ORIENTED_EDGE ( 'NONE', *, *, #40595, .F. ) ;
#28233 = B_SPLINE_CURVE_WITH_KNOTS ( 'NONE', 3,
 ( #1306, #10956, #1114, #13621, #29660, #36032, #20007, #26186, #14018, #38710, #10530, #13811, #35626, #7836 ),
 .UNSPECIFIED., .F., .F.,
 ( 4, 2, 2, 2, 2, 2, 4 ),
 ( 0.000000000000000000, 0.0007668932026506553078, 0.001150339803975984100, 0.001533786405301312784, 0.001917233006626641468, 0.002300679607951969935, 0.003067572810602619930 ),
 .UNSPECIFIED. ) ;
#28234 = EDGE_CURVE ( 'NONE', #14594, #23808, #16642, .T. ) ;
#28235 = EDGE_CURVE ( 'NONE', #17780, #23287, #38952, .T. ) ;
#28236 = CARTESIAN_POINT ( 'NONE',  ( 0.2404999449471016959, -0.9448023322974971050, 0.6708547505071026373 ) ) ;
#28237 = CARTESIAN_POINT ( 'NONE',  ( 0.2059273467974225835, -1.283046334493782359, -0.4400554600884078460 ) ) ;
#28238 = CARTESIAN_POINT ( 'NONE',  ( 0.4304258907306922621, -1.358867810424106315, 0.8370822606288357282 ) ) ;
#28239 = CARTESIAN_POINT ( 'NONE',  ( -0.1679467284716811559, 0.5217198260998645587, 0.1377606880063828310 ) ) ;
#28240 = ORIENTED_EDGE ( 'NONE', *, *, #15256, .F. ) ;
#28241 = ADVANCED_FACE ( 'NONE', ( #11515 ), #8600, .T. ) ;
#28242 = CARTESIAN_POINT ( 'NONE',  ( 0.4778061690595215572, -1.668017292664590645, 0.5682417262808788783 ) ) ;
#28243 = CARTESIAN_POINT ( 'NONE',  ( 0.6659438668093399238, -1.561559416909786613, 0.5697186424223757983 ) ) ;
#28244 = EDGE_CURVE ( 'NONE', #16545, #357, #22090, .T. ) ;
#28245 = CARTESIAN_POINT ( 'NONE',  ( 0.4634712904840416758, -1.711704060178988129, -0.5155029497116575543 ) ) ;
#28246 =( NAMED_UNIT ( * ) SI_UNIT ( $, .STERADIAN. ) SOLID_ANGLE_UNIT ( ) );
#28247 = LINE ( 'NONE', #15905, #466 ) ;
#28248 = CARTESIAN_POINT ( 'NONE',  ( 0.2059273467974226945, -1.283046334493782803, -0.2869361388274795921 ) ) ;
#28249 = CARTESIAN_POINT ( 'NONE',  ( 0.07539036843641495900, -1.329185100875404313, 0.6514330093269139477 ) ) ;
#28250 = CARTESIAN_POINT ( 'NONE',  ( 0.1874843899254543811, -0.7932266022496337055, 0.2338244398510780642 ) ) ;
#28251 = PERSON_AND_ORGANIZATION ( #28500, #32463 ) ;
#28252 = CARTESIAN_POINT ( 'NONE',  ( 0.3571225321066454073, -1.899149384614340130, -0.5066234194226268972 ) ) ;
#28253 = EDGE_CURVE ( 'NONE', #4285, #12872, #29426, .T. ) ;
#28254 = APPROVAL ( #4557, 'UNSPECIFIED' ) ;
#28255 = CARTESIAN_POINT ( 'NONE',  ( 0.5845704849289827809, -1.492672057029025279, 0.5599513125418986714 ) ) ;
#28256 = CARTESIAN_POINT ( 'NONE',  ( -0.03877220711930370878, 0.03321538116298803495, 0.4752084053751550186 ) ) ;
#28257 = B_SPLINE_CURVE_WITH_KNOTS ( 'NONE', 3,
 ( #26559, #23486, #36003, #7809 ),
 .UNSPECIFIED., .F., .F.,
 ( 4, 4 ),
 ( 0.000000000000000000, 0.0003243177824960875302 ),
 .UNSPECIFIED. ) ;
#28258 = VERTEX_POINT ( 'NONE', #36999 ) ;
#28259 = CARTESIAN_POINT ( 'NONE',  ( -0.07216878364870298046, 0.07999999999999969635, -0.1249999999999999029 ) ) ;
#28260 = LINE ( 'NONE', #9550, #1342 ) ;
#28261 = CIRCLE ( 'NONE', #34168, 0.2000000000000000111 ) ;
#28262 = CARTESIAN_POINT ( 'NONE',  ( 0.08828290717378418917, -0.6324995549925619409, 0.03536146464536887857 ) ) ;
#28263 = ORIENTED_EDGE ( 'NONE', *, *, #1224, .T. ) ;
#28264 = CARTESIAN_POINT ( 'NONE',  ( 0.3405242896115078244, -1.744906522954274175, 0.4484829386636804971 ) ) ;
#28265 = CARTESIAN_POINT ( 'NONE',  ( 0.1251005810423869713, -1.257534650344321880, 0.7423098211221518250 ) ) ;
#28267 = ORIENTED_EDGE ( 'NONE', *, *, #31898, .T. ) ;
#28266 = VERTEX_POINT ( 'NONE', #18691 ) ;
#28268 = CARTESIAN_POINT ( 'NONE',  ( -0.1212602505241952427, -0.5073146173415898907, 0.1498414178977066080 ) ) ;
#28269 = AXIS2_PLACEMENT_3D ( 'NONE', #1326, #35257, #23341 ) ;
#28270 = ORIENTED_EDGE ( 'NONE', *, *, #39452, .T. ) ;
#28271 = DIRECTION ( 'NONE',  ( -8.881784197001246407E-16, 2.361472542561082612E-16, -1.000000000000000000 ) ) ;
#28272 = CARTESIAN_POINT ( 'NONE',  ( 0.1984983582844195016, -2.028698869828995388, -0.3115429933617774316 ) ) ;
#28274 = DIRECTION ( 'NONE',  ( 1.000000000000000000, -0.000000000000000000, -0.000000000000000000 ) ) ;
#28273 = CARTESIAN_POINT ( 'NONE',  ( 0.05634490452572782360, 0.4348542811545040854, 0.1466173361067543424 ) ) ;
#28275 = CARTESIAN_POINT ( 'NONE',  ( -0.002218965743620939825, -1.368565310413371705, -0.3828039145932563558 ) ) ;
#28276 = ORIENTED_EDGE ( 'NONE', *, *, #7983, .F. ) ;
#28277 = CARTESIAN_POINT ( 'NONE',  ( 0.09797155024083728514, -0.5964682206075406778, 0.3201474151171130322 ) ) ;
#28278 = ORIENTED_EDGE ( 'NONE', *, *, #29559, .F. ) ;
#28279 = EDGE_CURVE ( 'NONE', #22522, #21046, #18910, .T. ) ;
#28280 = CARTESIAN_POINT ( 'NONE',  ( 0.1499999999999994671, -0.5198120922912051745, 0.07362328916749301400 ) ) ;
#28281 = CARTESIAN_POINT ( 'NONE',  ( 0.07414319037446265304, -0.5634787072276313813, 0.2482676990552415974 ) ) ;
#28283 = DIRECTION ( 'NONE',  ( -1.000000000000000000, -0.000000000000000000, -0.000000000000000000 ) ) ;
#28282 = CARTESIAN_POINT ( 'NONE',  ( 0.4833924548366955731, -1.608298341119788422, -0.3888178814765106406 ) ) ;
#28284 = DIRECTION ( 'NONE',  ( -8.881784197001246407E-16, 2.361472542561082612E-16, -1.000000000000000000 ) ) ;
#28285 = CARTESIAN_POINT ( 'NONE',  ( 0.4122350904075519074, -1.076876625835822887, 0.6345610635168674740 ) ) ;
#28286 = EDGE_CURVE ( 'NONE', #33071, #25669, #34725, .T. ) ;
#28287 = CARTESIAN_POINT ( 'NONE',  ( 0.1266223302490341873, -1.314440782070608327, 0.5182417262812423209 ) ) ;
#28288 = CARTESIAN_POINT ( 'NONE',  ( 0.1897113924121462125, -0.5340544967971894152, 0.1465862501021127640 ) ) ;
#28289 = EDGE_CURVE ( 'NONE', #5485, #40210, #4782, .T. ) ;
#28290 = CARTESIAN_POINT ( 'NONE',  ( 0.5807000928386124583, -1.495207826712593890, 0.5692575695771724398 ) ) ;
#28291 = CARTESIAN_POINT ( 'NONE',  ( -0.05283102792148795107, 0.2421768296208693105, 0.4008516595826041029 ) ) ;
#28292 = DIRECTION ( 'NONE',  ( 1.000000000000000000, 1.138269997360101095E-15, -8.881784197001243449E-16 ) ) ;
#28293 = CARTESIAN_POINT ( 'NONE',  ( -0.03174036153405623839, -0.4702001351683494090, -0.2325364317535350001 ) ) ;
#28294 = TOROIDAL_SURFACE ( 'NONE', #5934, 0.5250000000000000222, 0.01499999999999999944 ) ;
#28295 = CARTESIAN_POINT ( 'NONE',  ( 0.1531253909584859019, -0.7850955375911295997, 0.6127314896756340667 ) ) ;
#28296 = LINE ( 'NONE', #19462, #31252 ) ;
#28297 = CARTESIAN_POINT ( 'NONE',  ( 0.4514527476588715560, -1.032880248282614266, 0.8272311760340308462 ) ) ;
#28298 = AXIS2_PLACEMENT_3D ( 'NONE', #33279, #32864, #26727 ) ;
#28299 = CARTESIAN_POINT ( 'NONE',  ( -0.05543910610525158017, 0.2544236545520490167, 0.3848133000241384383 ) ) ;
#28300 = EDGE_CURVE ( 'NONE', #1103, #23955, #38301, .T. ) ;
#28301 = CARTESIAN_POINT ( 'NONE',  ( 0.03387208585097720159, -1.140508953265759962, 0.6721967346510711039 ) ) ;
#28302 = CIRCLE ( 'NONE', #29629, 0.1875727115490685715 ) ;
#28303 = CARTESIAN_POINT ( 'NONE',  ( 0.6033996618073826923, -1.480667803124354531, -0.5155029497116575543 ) ) ;
#28304 = CARTESIAN_POINT ( 'NONE',  ( 0.1934354357533958624, -0.7450421482614953961, 0.3186346416980788132 ) ) ;
#28305 = B_SPLINE_CURVE_WITH_KNOTS ( 'NONE', 3,
 ( #29744, #5048, #23597, #17403, #1799, #26874, #39405, #2580, #24604, #18004, #1982, #27676, #30354, #34046, #37332, #14927, #24390, #24003 ),
 .UNSPECIFIED., .F., .F.,
 ( 4, 2, 2, 2, 2, 2, 2, 2, 4 ),
 ( 0.000000000000000000, 0.0007746617437634291566, 0.001549323487526858313, 0.002323985231290287470, 0.003098646975053716626, 0.003873308718817145783, 0.004647970462580574939, 0.005422632206344004530, 0.006197293950107433252 ),
 .UNSPECIFIED. ) ;
#28306 = CARTESIAN_POINT ( 'NONE',  ( 0.06443582815874859815, -0.8352844082028778594, 0.1457185332388699350 ) ) ;
#28307 = CARTESIAN_POINT ( 'NONE',  ( 0.000000000000000000, 0.000000000000000000, 0.000000000000000000 ) ) ;
#28308 = FACE_OUTER_BOUND ( 'NONE', #4784, .T. ) ;
#28309 = ORIENTED_EDGE ( 'NONE', *, *, #2228, .F. ) ;
#28310 = CARTESIAN_POINT ( 'NONE',  ( 0.1499999999999993283, 0.3232818887608624459, -0.4449593469062196882 ) ) ;
#28311 = CARTESIAN_POINT ( 'NONE',  ( 0.3853365039963215222, -1.652093682163140453, -0.3956870249903657322 ) ) ;
#28312 = CARTESIAN_POINT ( 'NONE',  ( 0.6642913206916110092, -1.495764917729122123, 0.4182417262808777458 ) ) ;
#28313 = CARTESIAN_POINT ( 'NONE',  ( 0.6985364634159124675, -1.438850461896725275, 0.5682400285031795617 ) ) ;
#28314 = DIRECTION ( 'NONE',  ( 0.4999999999999972800, -0.7377595849475294676, -0.4535535192433765017 ) ) ;
#28315 = EDGE_LOOP ( 'NONE', ( #33531, #5901, #39228, #13982 ) ) ;
#28316 = CARTESIAN_POINT ( 'NONE',  ( 0.3544525855956190963, -1.628498139902242681, -0.6593841416022943047 ) ) ;
#28317 = CARTESIAN_POINT ( 'NONE',  ( 0.2232773634713763056, -1.353530203713960045, 0.4677345876144705095 ) ) ;
#28318 = CARTESIAN_POINT ( 'NONE',  ( 0.1856533569311497323, -0.7573055082216308964, 0.1457185332388697685 ) ) ;
#28319 = CARTESIAN_POINT ( 'NONE',  ( 0.04575185649130700943, 0.3363955107642143116, -0.3523382570435943384 ) ) ;
#28320 = CARTESIAN_POINT ( 'NONE',  ( 0.5120345133055148601, -1.314022687763800157, 0.5963220732961661552 ) ) ;
#28321 = VECTOR ( 'NONE', #34508, 39.37007874015748143 ) ;
#28323 = CARTESIAN_POINT ( 'NONE',  ( -0.02000000000000000042, -2.183180860297908144, -0.4937760292030871079 ) ) ;
#28322 = DIRECTION ( 'NONE',  ( -7.000205099780314469E-17, -1.000000000000000000, 6.590151126658399604E-16 ) ) ;
#28324 = CARTESIAN_POINT ( 'NONE',  ( 0.4709147388527493705, -1.070627459034787954, 0.6206731519243955386 ) ) ;
#28325 = EDGE_LOOP ( 'NONE', ( #5183, #8009, #30137, #37323, #8741, #27187, #14781 ) ) ;
#28326 = APPROVAL_STATUS ( 'not_yet_approved' ) ;
#28327 = AXIS2_PLACEMENT_3D ( 'NONE', #31248, #27743, #14572 ) ;
#28328 = CARTESIAN_POINT ( 'NONE',  ( 0.05267389698015547544, -1.086150594168910466, 0.7379831432407867320 ) ) ;
#28329 = ORIENTED_EDGE ( 'NONE', *, *, #5102, .F. ) ;
#28330 = EDGE_CURVE ( 'NONE', #7024, #19095, #12028, .T. ) ;
#28331 = ORIENTED_EDGE ( 'NONE', *, *, #15969, .F. ) ;
#28332 = CIRCLE ( 'NONE', #2054, 0.2149999999999999967 ) ;
#28333 = CARTESIAN_POINT ( 'NONE',  ( 0.3852216438992382419, -1.605616193201484965, 0.5739667088636910552 ) ) ;
#28335 = CARTESIAN_POINT ( 'NONE',  ( 0.1114066244466402900, -0.9052510818166191742, 0.04196736182216751626 ) ) ;
#28334 = CARTESIAN_POINT ( 'NONE',  ( -0.2399999999999999079, -3.730063144961804245, -0.1064410973704724706 ) ) ;
#28336 = CARTESIAN_POINT ( 'NONE',  ( -0.2399999999999999079, -3.701811653776600597, -0.3192834175180690459 ) ) ;
#28337 = ORIENTED_EDGE ( 'NONE', *, *, #35051, .F. ) ;
#28338 = AXIS2_PLACEMENT_3D ( 'NONE', #4771, #8071, #36472 ) ;
#28339 = EDGE_CURVE ( 'NONE', #890, #40614, #1541, .T. ) ;
#28340 = ORIENTED_EDGE ( 'NONE', *, *, #40559, .F. ) ;
#28341 = CARTESIAN_POINT ( 'NONE',  ( 0.1734973056165642902, -1.209394307038482497, -0.5155029497116575543 ) ) ;
#28342 = EDGE_CURVE ( 'NONE', #12586, #38403, #8082, .T. ) ;
#28343 = CARTESIAN_POINT ( 'NONE',  ( 0.5663790608840560958, -1.497944059049526988, 0.6446960571708316712 ) ) ;
#28344 = EDGE_LOOP ( 'NONE', ( #6810, #18215, #4600, #13838, #23192, #33949, #9818, #33699, #36064 ) ) ;
#28345 = CARTESIAN_POINT ( 'NONE',  ( 0.01405263366207808347, -0.9640798247225310647, 0.3811368675598582612 ) ) ;
#28346 = CARTESIAN_POINT ( 'NONE',  ( 0.07420452683010890504, -1.738585387657813675, -0.3647249226900559083 ) ) ;
#28347 = FACE_OUTER_BOUND ( 'NONE', #31871, .T. ) ;
#28348 = CARTESIAN_POINT ( 'NONE',  ( 0.6572879434354249595, -1.449559110403086049, -0.6172981636778317460 ) ) ;
#28349 = ADVANCED_FACE ( 'NONE', ( #12323 ), #28353, .F. ) ;
#28350 = CARTESIAN_POINT ( 'NONE',  ( 0.2983165958604226398, -1.151818276997767621, 0.5182417262812423209 ) ) ;
#28351 = CARTESIAN_POINT ( 'NONE',  ( 0.3436484202359983975, -1.636297845364965697, -0.6542514959024295917 ) ) ;
#28352 = AXIS2_PLACEMENT_3D ( 'NONE', #17617, #30967, #8750 ) ;
#28353 = PLANE ( 'NONE',  #5425 ) ;
#28354 = CARTESIAN_POINT ( 'NONE',  ( 0.4264202721361137760, -1.467519734074644200, -0.5166151207188711680 ) ) ;
#28355 = CARTESIAN_POINT ( 'NONE',  ( 0.1210494546010137118, -1.266445924951928204, 0.6212394332447065404 ) ) ;
#28356 = EDGE_CURVE ( 'NONE', #9095, #21137, #6531, .T. ) ;
#28357 = CARTESIAN_POINT ( 'NONE',  ( 0.3005522690096895100, -1.423263844426111868, -0.7187326247832939163 ) ) ;
#28358 = CARTESIAN_POINT ( 'NONE',  ( 0.1166065821415037673, -1.415338206367125817, 0.5822564622277803803 ) ) ;
#28359 = DATE_AND_TIME ( #18698, #23340 ) ;
#28360 = ADVANCED_FACE ( 'NONE', ( #37823 ), #37714, .T. ) ;
#28361 = CIRCLE ( 'NONE', #30996, 0.05000000000000000971 ) ;
#28362 = CARTESIAN_POINT ( 'NONE',  ( 0.3689192748036780878, -1.014666054483551294, 0.6186952232919745720 ) ) ;
#28363 = EDGE_CURVE ( 'NONE', #6766, #8015, #25068, .T. ) ;
#28364 = CARTESIAN_POINT ( 'NONE',  ( 0.1916453137239563509, -1.371753268179084717, 0.4817276165294532841 ) ) ;
#28365 = CARTESIAN_POINT ( 'NONE',  ( 0.5523000078138265989, -1.163818204720048266, 0.6057417262810179670 ) ) ;
#28366 = DIRECTION ( 'NONE',  ( 0.8660512985181131329, 0.4999551463232376758, 0.000000000000000000 ) ) ;
#28367 = VECTOR ( 'NONE', #14408, 39.37007874015748143 ) ;
#28368 = CIRCLE ( 'NONE', #6087, 0.1033070866141732880 ) ;
#28369 = CARTESIAN_POINT ( 'NONE',  ( 0.0002700364102348538193, -0.8386493658592084621, 0.3780876778669690075 ) ) ;
#28370 = CARTESIAN_POINT ( 'NONE',  ( 0.0001126841386759542179, -0.5849248619627643864, -0.08138210067616551135 ) ) ;
#28371 = AXIS2_PLACEMENT_3D ( 'NONE', #7510, #26066, #1370 ) ;
#28372 = CARTESIAN_POINT ( 'NONE',  ( 0.6929208297549553919, -1.429122597532291650, 0.5682417262808779901 ) ) ;
#28373 = CARTESIAN_POINT ( 'NONE',  ( 0.1960722456818423942, -1.288731303253011218, -0.2917126172454974631 ) ) ;
#28374 = ORIENTED_EDGE ( 'NONE', *, *, #440, .T. ) ;
#28375 = ORIENTED_EDGE ( 'NONE', *, *, #23735, .T. ) ;
#28376 = CARTESIAN_POINT ( 'NONE',  ( 0.04582889109739201466, -0.2312034125369023252, -0.4285435303321084577 ) ) ;
#28377 = ORIENTED_EDGE ( 'NONE', *, *, #29103, .T. ) ;
#28378 = DIRECTION ( 'NONE',  ( 8.881784197001246407E-16, -2.361472542561082612E-16, 1.000000000000000000 ) ) ;
#28379 = CARTESIAN_POINT ( 'NONE',  ( -0.02953079040095693900, -0.4684706630666107263, -0.2484463060367401721 ) ) ;
#28380 = CARTESIAN_POINT ( 'NONE',  ( 0.6113557282315684738, -1.476144099735155368, 0.5498370725323885599 ) ) ;
#28382 = VERTEX_POINT ( 'NONE', #21592 ) ;
#28381 = CARTESIAN_POINT ( 'NONE',  ( 0.3690965330173307524, -1.099411688709415413, 0.5182417262812423209 ) ) ;
#28383 = AXIS2_PLACEMENT_3D ( 'NONE', #19040, #18630, #12869 ) ;
#28384 = VERTEX_POINT ( 'NONE', #34117 ) ;
#28385 = CARTESIAN_POINT ( 'NONE',  ( 0.2024457102403973141, -0.7198351356486335506, 0.3420682486339518547 ) ) ;
#28386 = ORIENTED_EDGE ( 'NONE', *, *, #17205, .T. ) ;
#28387 = CARTESIAN_POINT ( 'NONE',  ( 0.2974186907859220352, -1.656756618909332124, 0.5765815979583946982 ) ) ;
#28389 = CARTESIAN_POINT ( 'NONE',  ( 0.1190963382269523835, -1.288349449013993508, 0.6004008909010771777 ) ) ;
#28388 = CARTESIAN_POINT ( 'NONE',  ( 0.5026806121458677890, -1.673566903547699436, -0.4262783769486948593 ) ) ;
#28390 = FACE_OUTER_BOUND ( 'NONE', #4232, .T. ) ;
#28391 = CARTESIAN_POINT ( 'NONE',  ( -0.02000000000000000042, -2.097192720079996242, -0.6592403319832980113 ) ) ;
#28392 = APPROVAL_DATE_TIME ( #9675, #38939 ) ;
#28393 = VECTOR ( 'NONE', #33255, 39.37007874015748143 ) ;
#28394 = EDGE_CURVE ( 'NONE', #36916, #11923, #17923, .T. ) ;
#28395 = CARTESIAN_POINT ( 'NONE',  ( 0.1909286924077255032, -1.257064795538239022, -0.7462941026102624109 ) ) ;
#28397 = ORIENTED_EDGE ( 'NONE', *, *, #9477, .F. ) ;
#28396 = EDGE_LOOP ( 'NONE', ( #37378, #17995, #38727, #58 ) ) ;
#28398 = EDGE_CURVE ( 'NONE', #11030, #33002, #19594, .T. ) ;
#28399 = CARTESIAN_POINT ( 'NONE',  ( 5.330214113969031311E-16, -0.2899999999999993139, 0.07499999999999919231 ) ) ;
#28400 = CARTESIAN_POINT ( 'NONE',  ( 0.3817504269947164519, -1.726033828776057266, 0.4251703030630530900 ) ) ;
#28401 = CARTESIAN_POINT ( 'NONE',  ( -0.02235124290213139076, -0.07000983313419636977, -0.5077112423787091267 ) ) ;
#28402 = CARTESIAN_POINT ( 'NONE',  ( -0.05464101615137761936, -1.906060000575976243, -0.2916525572568464675 ) ) ;
#28403 = AXIS2_PLACEMENT_3D ( 'NONE', #6390, #38065, #15656 ) ;
#28404 = CARTESIAN_POINT ( 'NONE',  ( 0.1261292094506294148, -0.8244062005499848134, 0.1786220713650574499 ) ) ;
#28405 = CARTESIAN_POINT ( 'NONE',  ( -0.2746410161513779258, -2.183180860297908144, -0.4937760292030871079 ) ) ;
#28406 = CARTESIAN_POINT ( 'NONE',  ( 0.1822227791794524265, -1.186887416757892888, 1.012788992251323350 ) ) ;
#28407 = CARTESIAN_POINT ( 'NONE',  ( 0.1399999999999994582, 0.2149999999999997469, -5.463695987328526437E-16 ) ) ;
#28408 = CARTESIAN_POINT ( 'NONE',  ( -0.1210148435730038635, -0.5061394519556884353, 0.1438724812234773442 ) ) ;
#28409 = CARTESIAN_POINT ( 'NONE',  ( -0.06919656468380704084, -0.09959325338431368468, 0.09813923389047332635 ) ) ;
#28410 = DIRECTION ( 'NONE',  ( -0.000000000000000000, -0.9343694307158671997, 0.3563057211773426602 ) ) ;
#28411 =( NAMED_UNIT ( * ) SI_UNIT ( $, .STERADIAN. ) SOLID_ANGLE_UNIT ( ) );
#28412 = FACE_BOUND ( 'NONE', #11078, .T. ) ;
#28413 = CARTESIAN_POINT ( 'NONE',  ( 0.1249840844849290228, -1.018512954913863844, 0.9570223520903572423 ) ) ;
#28414 = CARTESIAN_POINT ( 'NONE',  ( 0.1017718266971927438, -1.363853815782150924, 0.6879803626369204173 ) ) ;
#28415 = PERSON_AND_ORGANIZATION ( #28500, #32463 ) ;
#28416 = AXIS2_PLACEMENT_3D ( 'NONE', #34162, #33977, #278 ) ;
#28417 = CARTESIAN_POINT ( 'NONE',  ( -0.05269111014005918581, 0.4484844745756846884, 0.1361491033660743311 ) ) ;
#28418 = CARTESIAN_POINT ( 'NONE',  ( 0.6965523178711373609, -1.533409646290749828, 0.5827623954312006749 ) ) ;
#28419 = AXIS2_PLACEMENT_3D ( 'NONE', #30381, #40236, #36952 ) ;
#28420 = ORIENTED_EDGE ( 'NONE', *, *, #26541, .F. ) ;
#28421 = ORIENTED_EDGE ( 'NONE', *, *, #15243, .T. ) ;
#28422 = CARTESIAN_POINT ( 'NONE',  ( 0.1055042220909814948, -1.411635777700159800, 0.5659469840222108861 ) ) ;
#28423 = CARTESIAN_POINT ( 'NONE',  ( 0.2493882130568067512, -1.574984837766822965, 0.8682191111569700359 ) ) ;
#28424 = AXIS2_PLACEMENT_3D ( 'NONE', #12751, #252, #25313 ) ;
#28425 = CARTESIAN_POINT ( 'NONE',  ( 0.1320129719769623233, -0.5716393116954411324, 0.2400138632674352901 ) ) ;
#28427 = ORIENTED_EDGE ( 'NONE', *, *, #699, .F. ) ;
#28426 = FACE_OUTER_BOUND ( 'NONE', #6858, .T. ) ;
#28429 = ORIENTED_EDGE ( 'NONE', *, *, #18086, .F. ) ;
#28428 = ORIENTED_EDGE ( 'NONE', *, *, #28363, .T. ) ;
#28430 = DIRECTION ( 'NONE',  ( 1.000000000000000000, -0.000000000000000000, -0.000000000000000000 ) ) ;
#28431 = ORIENTED_EDGE ( 'NONE', *, *, #17546, .F. ) ;
#28432 = AXIS2_PLACEMENT_3D ( 'NONE', #3853, #22607, #13320 ) ;
#28433 = CARTESIAN_POINT ( 'NONE',  ( -0.1707605070207384723, 0.4977265752128581799, 0.1434892898517914628 ) ) ;
#28434 = COORDINATED_UNIVERSAL_TIME_OFFSET ( 0, 0, .AHEAD. ) ;
#28435 = PLANE ( 'NONE',  #11300 ) ;
#28436 = ORIENTED_EDGE ( 'NONE', *, *, #6993, .T. ) ;
#28437 = CARTESIAN_POINT ( 'NONE',  ( 0.1005327108732830682, -0.7654220390130497265, 0.3417061460467297751 ) ) ;
#28438 = FACE_OUTER_BOUND ( 'NONE', #22935, .T. ) ;
#28439 = CARTESIAN_POINT ( 'NONE',  ( 0.5245207932248472371, -1.526647649442574473, 0.5610456953807425595 ) ) ;
#28440 = CARTESIAN_POINT ( 'NONE',  ( 0.5749953953004710572, -1.612551028885189863, -0.5288418706057514962 ) ) ;
#28441 = CARTESIAN_POINT ( 'NONE',  ( -0.05283710938261110268, -0.2421875768565582288, 0.4008269984734637026 ) ) ;
#28442 = VERTEX_POINT ( 'NONE', #22612 ) ;
#28443 = VECTOR ( 'NONE', #30031, 39.37007874015748854 ) ;
#28444 = CARTESIAN_POINT ( 'NONE',  ( 0.4486004395777776210, -1.685563693236277416, 0.6043086445225501757 ) ) ;
#28445 = CARTESIAN_POINT ( 'NONE',  ( 0.6990254338941188639, -1.438807163059433458, 0.5794947641723904308 ) ) ;
#28446 = LINE ( 'NONE', #22494, #16101 ) ;
#28447 = AXIS2_PLACEMENT_3D ( 'NONE', #1040, #26118, #35749 ) ;
#28448 = CARTESIAN_POINT ( 'NONE',  ( 0.6097404743490668633, -1.478808349948183443, 0.5913594100522746588 ) ) ;
#28449 = DIRECTION ( 'NONE',  ( 0.4999551463232372317, -0.8660512985181135770, 0.000000000000000000 ) ) ;
#28450 = CARTESIAN_POINT ( 'NONE',  ( 0.1852718761952666104, -0.8389489029336036907, 0.1457185345930598341 ) ) ;
#28451 = CARTESIAN_POINT ( 'NONE',  ( 0.01548846960712783535, -0.5203207976466778240, -0.08861466064782558272 ) ) ;
#28452 = CARTESIAN_POINT ( 'NONE',  ( 0.04329528483221436325, -1.226008797194266586, 0.6628706426414217034 ) ) ;
#28453 = CIRCLE ( 'NONE', #29781, 0.1600000000000005584 ) ;
#28454 = CARTESIAN_POINT ( 'NONE',  ( 0.5138235575674273692, -1.118575097671381080, 0.5744212141803229921 ) ) ;
#28455 = PRODUCT_CONTEXT ( 'NONE', #27157, 'mechanical' ) ;
#28456 = DIRECTION ( 'NONE',  ( 0.8660512985181135770, 0.4999551463232372317, 0.000000000000000000 ) ) ;
#28457 = B_SPLINE_CURVE_WITH_KNOTS ( 'NONE', 3,
 ( #34234, #24597, #28087, #27669, #12243, #21520 ),
 .UNSPECIFIED., .F., .F.,
 ( 4, 2, 4 ),
 ( 0.000000000000000000, 0.5000000000000000000, 1.000000000000000000 ),
 .UNSPECIFIED. ) ;
#28458 = CARTESIAN_POINT ( 'NONE',  ( 0.4662642109249354738, -1.558585770123256387, 0.5489026516414302614 ) ) ;
#28459 = APPLICATION_CONTEXT ( 'configuration controlled 3d designs of mechanical parts and assemblies' ) ;
#28460 = CARTESIAN_POINT ( 'NONE',  ( -0.05076541221973600304, -0.04887304573182980894, 0.4712631214448610439 ) ) ;
#28461 =( BOUNDED_SURFACE ( )  B_SPLINE_SURFACE ( 3, 2, ( 
 ( #7953, #23826, #11670 ),
 ( #20938, #36348, #12076 ),
 ( #8774, #2217, #8561 ),
 ( #36750, #4867, #17827 ),
 ( #15147, #27320, #30386 ),
 ( #21351, #8165, #14757 ),
 ( #40034, #40240, #14538 ),
 ( #33890, #36141, #30791 ),
 ( #8369, #39849, #24226 ),
 ( #20525, #17436, #29991 ),
 ( #27510, #27102, #14340 ),
 ( #21134, #33661, #5474 ) ),
 .UNSPECIFIED., .F., .F., .F. ) 
 B_SPLINE_SURFACE_WITH_KNOTS ( ( 4, 2, 2, 2, 2, 4 ),
 ( 3, 3 ),
 ( -2.194247311574145322E-05, 0.0004166382859409436027, 0.0008552190449976286146, 0.001732380563110998747, 0.002609542081224368662, 0.003486703599337739011 ),
 ( 0.000000000000000000, 1.000000000000000000 ),
 .UNSPECIFIED. ) 
 GEOMETRIC_REPRESENTATION_ITEM ( )  RATIONAL_B_SPLINE_SURFACE ( (
 ( 1.000000000000000000, 0.7032244542329121328, 1.000000000000000000),
 ( 1.000000000000000000, 0.7033233483186307478, 1.000000000000000000),
 ( 1.000000000000000000, 0.7045246448745312584, 1.000000000000000000),
 ( 1.000000000000000000, 0.7073062858921952412, 1.000000000000000000),
 ( 1.000000000000000000, 0.7090759679026412687, 1.000000000000000000),
 ( 1.000000000000000000, 0.7151776825359495993, 1.000000000000000000),
 ( 1.000000000000000000, 0.7200725892538363260, 1.000000000000000000),
 ( 1.000000000000000000, 0.7289630251952065043, 1.000000000000000000),
 ( 1.000000000000000000, 0.7326908029506756792, 1.000000000000000000),
 ( 1.000000000000000000, 0.7366628156064797261, 1.000000000000000000),
 ( 1.000000000000000000, 0.7367803224921714023, 1.000000000000000000),
 ( 1.000000000000000000, 0.7348357107204075422, 1.000000000000000000) ) ) 
 REPRESENTATION_ITEM ( '' )  SURFACE ( )  );
#28462 = VERTEX_POINT ( 'NONE', #20126 ) ;
#28463 = CARTESIAN_POINT ( 'NONE',  ( 0.4390406754936738154, -1.575939765669403192, 0.6014929107880048198 ) ) ;
#28464 = DIRECTION ( 'NONE',  ( 1.000000000000000000, 0.000000000000000000, 0.000000000000000000 ) ) ;
#28465 = AXIS2_PLACEMENT_3D ( 'NONE', #19264, #38167, #3619 ) ;
#28466 = CARTESIAN_POINT ( 'NONE',  ( 0.08592534930546107119, -0.7849569399949006820, 0.07020894479808938160 ) ) ;
#28467 = VERTEX_POINT ( 'NONE', #4266 ) ;
#28468 = CARTESIAN_POINT ( 'NONE',  ( 0.1999999999999789724, -2.183180860297921466, -0.4937760292030871079 ) ) ;
#28469 = CARTESIAN_POINT ( 'NONE',  ( 0.1700065278191711104, -1.375428071273553376, 0.6154404651844289642 ) ) ;
#28471 = VERTEX_POINT ( 'NONE', #26106 ) ;
#28470 = VERTEX_POINT ( 'NONE', #13119 ) ;
#28472 = CARTESIAN_POINT ( 'NONE',  ( -0.08000000000000000167, -1.906060000575976021, -0.2916525572568466340 ) ) ;
#28473 = CIRCLE ( 'NONE', #10071, 0.1849999999999994982 ) ;
#28474 = ORIENTED_EDGE ( 'NONE', *, *, #16068, .T. ) ;
#28475 = CARTESIAN_POINT ( 'NONE',  ( -0.01548846960707524721, 0.000000000000000000, 0.000000000000000000 ) ) ;
#28476 = CARTESIAN_POINT ( 'NONE',  ( 0.3959837544953576094, -1.690093441653652162, -0.5214913642057524834 ) ) ;
#28478 = LINE ( 'NONE', #6654, #35334 ) ;
#28477 = CARTESIAN_POINT ( 'NONE',  ( 0.05616044724337368454, 0.4336395721329034947, 0.1516614036261331178 ) ) ;
#28479 = CARTESIAN_POINT ( 'NONE',  ( 0.03301162916267817715, -0.2303793641368927225, -0.4673060013142924518 ) ) ;
#28480 = ORIENTED_EDGE ( 'NONE', *, *, #11146, .F. ) ;
#28481 = LINE ( 'NONE', #355, #35681 ) ;
#28482 = VERTEX_POINT ( 'NONE', #35141 ) ;
#28483 = CARTESIAN_POINT ( 'NONE',  ( 0.09014882583140459982, -0.6063924461725455073, 0.1729119204149524025 ) ) ;
#28484 = EDGE_LOOP ( 'NONE', ( #2195, #13641, #23550, #32537 ) ) ;
#28485 = AXIS2_PLACEMENT_3D ( 'NONE', #28118, #37885, #21955 ) ;
#28486 = ORIENTED_EDGE ( 'NONE', *, *, #5104, .F. ) ;
#28487 = CARTESIAN_POINT ( 'NONE',  ( 0.03309058451312577726, 0.08822157290690298137, 0.5132714794726482843 ) ) ;
#28488 = CARTESIAN_POINT ( 'NONE',  ( 0.3101835799050875475, -1.221649658806551297, 0.8662723704748881426 ) ) ;
#28489 = EDGE_CURVE ( 'NONE', #357, #31608, #20585, .T. ) ;
#28491 = CARTESIAN_POINT ( 'NONE',  ( 0.1499999999999993561, -0.3880410510314710182, 0.3755318131855027719 ) ) ;
#28490 = CARTESIAN_POINT ( 'NONE',  ( 0.4501395481517306285, -1.610781249451892716, -0.3723713353267660287 ) ) ;
#28492 = CARTESIAN_POINT ( 'NONE',  ( 0.06843411546424661707, -1.327640554429453168, 0.5682417262808774350 ) ) ;
#28493 = CARTESIAN_POINT ( 'NONE',  ( 0.3347563140814358018, -1.025429894978651779, 0.6211877635660684183 ) ) ;
#28494 = APPROVAL ( #21377, 'UNSPECIFIED' ) ;
#28495 = ORIENTED_EDGE ( 'NONE', *, *, #20738, .F. ) ;
#28496 = DIRECTION ( 'NONE',  ( 0.4999999999999940603, 0.7308273574226435976, 0.4646411234949414659 ) ) ;
#28497 = CARTESIAN_POINT ( 'NONE',  ( 0.1887412855916241194, -0.4595320686313542624, 0.1446142472693910663 ) ) ;
#28498 = CARTESIAN_POINT ( 'NONE',  ( 0.1458595596271754224, -0.6542043499068329604, 0.4259781829602066194 ) ) ;
#28499 = CARTESIAN_POINT ( 'NONE',  ( -0.04582713223189541912, 0.2312054150958166299, 0.4285473768184982490 ) ) ;
#28500 = PERSON ( 'UNSPECIFIED', 'UNSPECIFIED', 'UNSPECIFIED', ('UNSPECIFIED'), ('UNSPECIFIED'), ('UNSPECIFIED') ) ;
#28501 = CARTESIAN_POINT ( 'NONE',  ( 0.08372836835944071077, -1.326477885028105375, 0.4882417262808781966 ) ) ;
#28502 = CARTESIAN_POINT ( 'NONE',  ( -0.2300000000000002043, 0.5182417262804744906, 0.08500000000000018652 ) ) ;
#28503 = AXIS2_PLACEMENT_3D ( 'NONE', #11034, #35922, #27065 ) ;
#28504 = CARTESIAN_POINT ( 'NONE',  ( 0.4196576349101079351, -1.201297826476563024, 0.8179721269271881257 ) ) ;
#28505 = CARTESIAN_POINT ( 'NONE',  ( -0.05464101615137767487, -1.737515812098395118, -0.8661170628529262228 ) ) ;
#28506 = CARTESIAN_POINT ( 'NONE',  ( 0.2318926187578342901, -0.6847811903715324000, 0.4821206442548801596 ) ) ;
#28507 = VECTOR ( 'NONE', #22073, 39.37007874015748854 ) ;
#28508 = CIRCLE ( 'NONE', #4814, 0.1499999999999990785 ) ;
#28509 = FACE_OUTER_BOUND ( 'NONE', #15335, .T. ) ;
#28510 = CARTESIAN_POINT ( 'NONE',  ( 0.05981300713595071039, -1.256039768099636689, 0.6499504827381740180 ) ) ;
#28511 = CARTESIAN_POINT ( 'NONE',  ( 0.03643058821097026889, 0.4544345964805225901, -0.2356993163710955352 ) ) ;
#28512 = FACE_OUTER_BOUND ( 'NONE', #12857, .T. ) ;
#28513 = EDGE_CURVE ( 'NONE', #26063, #38731, #814, .T. ) ;
#28514 = DIRECTION ( 'NONE',  ( -0.4999999999999981681, 0.5755298573121171435, -0.6471208413753152255 ) ) ;
#28515 = DIRECTION ( 'NONE',  ( 0.000000000000000000, -0.5365213554527478168, 0.8438867430782083234 ) ) ;
#28516 = AXIS2_PLACEMENT_3D ( 'NONE', #23655, #26328, #10682 ) ;
#28517 = CARTESIAN_POINT ( 'NONE',  ( 0.1909286924077254755, -1.257064795538238577, -0.6405900374560394850 ) ) ;
#28518 = EDGE_CURVE ( 'NONE', #29909, #37390, #10707, .T. ) ;
#28519 = EDGE_LOOP ( 'NONE', ( #31021, #5508, #34851, #7288 ) ) ;
#28520 = DIRECTION ( 'NONE',  ( 0.000000000000000000, -2.697841949839120611E-14, -1.000000000000000000 ) ) ;
#28521 = CARTESIAN_POINT ( 'NONE',  ( 0.4102377630207764692, -1.609602033329217141, -0.3618696079564429624 ) ) ;
#28522 = EDGE_CURVE ( 'NONE', #11393, #2067, #33694, .T. ) ;
#28523 = DIRECTION ( 'NONE',  ( 7.000205099780314469E-17, 1.000000000000000000, -6.590151126658399604E-16 ) ) ;
#28524 = CARTESIAN_POINT ( 'NONE',  ( -0.2399999999999999079, -1.874946189051298617, -0.07947534077849525980 ) ) ;
#28525 = EDGE_CURVE ( 'NONE', #20299, #20709, #6945, .T. ) ;
#28526 = CARTESIAN_POINT ( 'NONE',  ( 0.3249891007434509982, -1.168521056691680382, 0.5670768804972423638 ) ) ;
#28527 = ADVANCED_FACE ( 'NONE', ( #35526 ), #2499, .T. ) ;
#28528 = ORIENTED_EDGE ( 'NONE', *, *, #8618, .T. ) ;
#28529 = CARTESIAN_POINT ( 'NONE',  ( 0.5240088150632713493, -1.676756884404518200, -0.5894117387006844178 ) ) ;
#28530 = FACE_OUTER_BOUND ( 'NONE', #11920, .T. ) ;
#28531 = CARTESIAN_POINT ( 'NONE',  ( 0.4717517922261478813, -1.668493369395022796, 0.4596108401464155668 ) ) ;
#28532 = CARTESIAN_POINT ( 'NONE',  ( 0.04285427992854337620, 0.3459934409501857489, -0.3537438177964267183 ) ) ;
#28533 = VECTOR ( 'NONE', #29495, 39.37007874015748143 ) ;
#28534 = CARTESIAN_POINT ( 'NONE',  ( 0.4964455468594098919, -1.286167783046271440, 0.6305352476659182859 ) ) ;
#28536 = CARTESIAN_POINT ( 'NONE',  ( -0.07216878364870325802, 0.000000000000000000, -0.1249999999999999029 ) ) ;
#28535 = DIRECTION ( 'NONE',  ( 1.000000000000000000, -8.054771744420970720E-13, -1.518808759990548047E-12 ) ) ;
#28537 = CARTESIAN_POINT ( 'NONE',  ( 0.4162441775219429263, -1.040631601589554034, 0.6343403631529308528 ) ) ;
#28538 = EDGE_LOOP ( 'NONE', ( #17004, #36466 ) ) ;
#28539 = APPROVAL_STATUS ( 'not_yet_approved' ) ;
#28540 = CARTESIAN_POINT ( 'NONE',  ( -0.002288348195190195115, -0.8555288688122634211, 0.1914435222285272298 ) ) ;
#28541 = EDGE_LOOP ( 'NONE', ( #18521, #7734, #7882 ) ) ;
#28542 = CONICAL_SURFACE ( 'NONE', #16037, 0.1762268159172233339, 0.7853981633974500554 ) ;
#28543 = AXIS2_PLACEMENT_3D ( 'NONE', #12906, #34898, #12688 ) ;
#28544 = CARTESIAN_POINT ( 'NONE',  ( 0.04803016009707770928, -0.5362635619093905071, 0.1543674294428551697 ) ) ;
#28545 = EDGE_CURVE ( 'NONE', #16949, #17350, #230, .T. ) ;
#28547 = CARTESIAN_POINT ( 'NONE',  ( 0.1842062797954040487, -0.8537295084795349931, 0.1492890682281529657 ) ) ;
#28546 = CARTESIAN_POINT ( 'NONE',  ( 0.08672709535528307090, -0.7521132484280468322, 0.01666405986956852672 ) ) ;
#28548 = LINE ( 'NONE', #422, #20456 ) ;
#28549 = APPROVAL_PERSON_ORGANIZATION ( #24180, #39090, #40598 ) ;
#28550 = ORIENTED_EDGE ( 'NONE', *, *, #35879, .F. ) ;
#28551 = B_SPLINE_CURVE_WITH_KNOTS ( 'NONE', 3,
 ( #32804, #29727, #13874, #27273, #30142, #1367, #14096, #39391, #38987, #4816, #20284, #1573, #39204, #11631, #11025, #7905, #23583, #29948, #20477, #33010, #17390, #1787, #1970, #23990, #14301, #11212, #8522, #23778, #36295, #8118, #20695, #33226, #5035, #2169, #14489, #39801 ),
 .UNSPECIFIED., .F., .F.,
 ( 4, 2, 2, 2, 2, 2, 2, 2, 2, 2, 2, 2, 2, 2, 2, 2, 2, 4 ),
 ( -6.000000000055645558E-08, 0.001367160778072117446, 0.002050771167108184339, 0.002734381556144251449, 0.003417991945180318125, 0.004101602334216384801, 0.004785212723252451478, 0.005468823112288519021, 0.006152433501324586565, 0.006836043890360653241, 0.008203264668432784859, 0.008886875057468849801, 0.009570485446504914742, 0.01093770622457703942, 0.01230492700264916410, 0.01367214778072128704, 0.01640658933686554161, 0.02187547244915405420 ),
 .UNSPECIFIED. ) ;
#28552 = CARTESIAN_POINT ( 'NONE',  ( 0.3348264461528376867, -1.289438405178311209, 0.5735458425336941168 ) ) ;
#28553 = CARTESIAN_POINT ( 'NONE',  ( 0.3508289865554531928, -1.132338794321712916, 0.8154384950216992944 ) ) ;
#28554 = ORIENTED_EDGE ( 'NONE', *, *, #19742, .F. ) ;
#28555 = AXIS2_PLACEMENT_3D ( 'NONE', #32378, #36083, #757 ) ;
#28556 = CARTESIAN_POINT ( 'NONE',  ( 0.1874490856083247670, -0.6900333170255394943, 0.05073663252241766841 ) ) ;
#28557 = CARTESIAN_POINT ( 'NONE',  ( 0.1367339749541140737, -1.455102376090395389, -0.3611272873345107159 ) ) ;
#28558 = CARTESIAN_POINT ( 'NONE',  ( 0.6006288095222466206, -1.388058312517433057, -0.6250000000000001110 ) ) ;
#28559 = CIRCLE ( 'NONE', #22575, 0.04330708661417343591 ) ;
#28560 = DIRECTION ( 'NONE',  ( 0.8660512985181130219, 0.4999551463232377868, 0.000000000000000000 ) ) ;
#28561 = EDGE_LOOP ( 'NONE', ( #35927, #29078, #9751, #19774 ) ) ;
#28562 = DIRECTION ( 'NONE',  ( 0.9998941247116546194, -0.01455087607601020412, 0.0001066420868422379362 ) ) ;
#28563 = CARTESIAN_POINT ( 'NONE',  ( 0.08534891775908995393, -0.7691016309398805983, 0.1031615689448583950 ) ) ;
#28564 = CARTESIAN_POINT ( 'NONE',  ( 0.2637382839637063547, -0.6009449316864781121, 0.1932256475537140750 ) ) ;
#28565 = DIRECTION ( 'NONE',  ( 0.0001066307966868756642, -1.551735798904719862E-06, -0.9999999943137325431 ) ) ;
#28566 = CARTESIAN_POINT ( 'NONE',  ( 0.1281055102147601044, -1.260775204155497375, 0.6226496396147861434 ) ) ;
#28567 = CARTESIAN_POINT ( 'NONE',  ( -0.002385887202282944899, -1.874416880861737633, -0.6477095634347505015 ) ) ;
#28568 = CARTESIAN_POINT ( 'NONE',  ( 0.1316017208954911033, -1.248059642665102942, 0.5182417262812423209 ) ) ;
#28569 = APPROVAL_DATE_TIME ( #631, #906 ) ;
#28570 = CIRCLE ( 'NONE', #33820, 0.1600000000000004752 ) ;
#28571 = CARTESIAN_POINT ( 'NONE',  ( 0.4434061351937851336, -1.055534433944394390, 0.6333734109485414931 ) ) ;
#28572 = AXIS2_PLACEMENT_3D ( 'NONE', #26800, #20411, #39326 ) ;
#28573 = LINE ( 'NONE', #16417, #32380 ) ;
#28574 = CARTESIAN_POINT ( 'NONE',  ( 0.5534381859858074071, -1.186304665530027558, 0.6057417262809816627 ) ) ;
#28575 = DIRECTION ( 'NONE',  ( 0.000000000000000000, -0.3882559824134196313, 0.9215515678030125057 ) ) ;
#28576 = AXIS2_PLACEMENT_3D ( 'NONE', #35957, #7766, #20332 ) ;
#28577 = EDGE_CURVE ( 'NONE', #24913, #20299, #6743, .T. ) ;
#28578 = AXIS2_PLACEMENT_3D ( 'NONE', #14720, #33432, #40207 ) ;
#28579 = APPLIED_APPROVAL_ASSIGNMENT ( #8649, ( #26625 ) ) ;
#28580 = CARTESIAN_POINT ( 'NONE',  ( 0.06399702207960011879, -1.267566535398010563, 0.6886354586937382116 ) ) ;
#28581 = CARTESIAN_POINT ( 'NONE',  ( 0.6147843586992604026, -1.475607795738035577, -0.4128325507852580456 ) ) ;
#28582 = EDGE_CURVE ( 'NONE', #22431, #22474, #19262, .T. ) ;
#28583 = DIRECTION ( 'NONE',  ( 0.8660512985181134660, 0.4999551463232371762, 0.000000000000000000 ) ) ;
#28584 = CARTESIAN_POINT ( 'NONE',  ( -0.1157923916715203477, -0.5295015842444287246, 0.3599999999999988765 ) ) ;
#28585 = ADVANCED_FACE ( 'NONE', ( #23220, #3676 ), #1412, .F. ) ;
#28586 = ORIENTED_EDGE ( 'NONE', *, *, #33508, .T. ) ;
#28587 = ORIENTED_EDGE ( 'NONE', *, *, #37119, .F. ) ;
#28588 = FACE_OUTER_BOUND ( 'NONE', #2140, .T. ) ;
#28589 = ORIENTED_EDGE ( 'NONE', *, *, #6864, .T. ) ;
#28590 = CARTESIAN_POINT ( 'NONE',  ( -0.04155248107635972632, 0.01723053523177093399, 0.4699878081388670914 ) ) ;
#28591 = CARTESIAN_POINT ( 'NONE',  ( 0.04155248107635921284, 0.2623121065566131893, 0.3903559784317156556 ) ) ;
#28592 = CARTESIAN_POINT ( 'NONE',  ( 0.5755900408509843080, -1.422326445372266379, 0.6246236810960820174 ) ) ;
#28594 = EDGE_LOOP ( 'NONE', ( #4032, #6491, #39881 ) ) ;
#28593 = CARTESIAN_POINT ( 'NONE',  ( 0.01548846960712797240, -0.3688619771571953754, -0.3775276577326278082 ) ) ;
#28595 = ORIENTED_EDGE ( 'NONE', *, *, #26982, .T. ) ;
#28596 = CARTESIAN_POINT ( 'NONE',  ( 0.5859306440460040344, -1.604270562037251713, 0.4385162621962425678 ) ) ;
#28597 = EDGE_LOOP ( 'NONE', ( #38285, #25879, #37088, #9182 ) ) ;
#28598 = CARTESIAN_POINT ( 'NONE',  ( 0.2992444779679390154, -1.656912578960057170, 0.6025679435408887175 ) ) ;
#28599 = EDGE_CURVE ( 'NONE', #12256, #30547, #26291, .T. ) ;
#28601 = CARTESIAN_POINT ( 'NONE',  ( -0.3000000000000000999, -1.730153431576819001, -0.08301574631829751472 ) ) ;
#28600 = CARTESIAN_POINT ( 'NONE',  ( 0.5953197980378828191, -1.599064723402610300, 0.4311035055375505576 ) ) ;
#28602 = CARTESIAN_POINT ( 'NONE',  ( -0.02000000000000000042, -1.944084441611813707, -0.4562887203618206655 ) ) ;
#28603 = CARTESIAN_POINT ( 'NONE',  ( 0.1844975769085782369, -0.8266995537623093027, 0.05501147976861575639 ) ) ;
#28604 = VECTOR ( 'NONE', #3509, 39.37007874015748854 ) ;
#28605 = LINE ( 'NONE', #9250, #1457 ) ;
#28607 = ORIENTED_EDGE ( 'NONE', *, *, #28018, .F. ) ;
#28606 = VERTEX_POINT ( 'NONE', #16415 ) ;
#28608 = EDGE_CURVE ( 'NONE', #37954, #33895, #35016, .T. ) ;
#28609 = TOROIDAL_SURFACE ( 'NONE', #23371, 0.04249999999999999611, 0.02499999999999995628 ) ;
#28610 = CARTESIAN_POINT ( 'NONE',  ( 0.3923243630925510872, -1.966611948492501316, -0.4968729097670202544 ) ) ;
#28611 = CARTESIAN_POINT ( 'NONE',  ( 0.1862785929144180619, -0.9153889657460283491, 0.1591853427980846336 ) ) ;
#28612 = CARTESIAN_POINT ( 'NONE',  ( -0.03662792686184396240, 0.04111994379180689690, -0.4792679903722392165 ) ) ;
#28613 = CARTESIAN_POINT ( 'NONE',  ( -0.08000000000000000167, -2.321277022828569958, -0.5785054236952983375 ) ) ;
#28614 = CARTESIAN_POINT ( 'NONE',  ( 0.2149313114772367361, -0.9162195584033384632, 0.6271167533926740312 ) ) ;
#28615 = LOCAL_TIME ( 0, 53, 7.000000000000000000, #38319 ) ;
#28616 = CARTESIAN_POINT ( 'NONE',  ( 0.03315096893860772914, -0.7291808658770100315, 0.5842526001130612379 ) ) ;
#28617 = CARTESIAN_POINT ( 'NONE',  ( -0.1061036098701634706, -0.4827967145417200179, 0.3599999999999998757 ) ) ;
#28618 = CIRCLE ( 'NONE', #31905, 0.1700000000000000400 ) ;
#28619 = CARTESIAN_POINT ( 'NONE',  ( -0.05464101615137786222, -2.183180860297908144, -0.4937760292030871079 ) ) ;
#28620 = DIRECTION ( 'NONE',  ( 1.000000000000000000, 0.000000000000000000, 0.000000000000000000 ) ) ;
#28621 = CARTESIAN_POINT ( 'NONE',  ( 1.127432441697302489E-16, 4.942613344993744236E-17, 0.07499999999999998335 ) ) ;
#28622 = CARTESIAN_POINT ( 'NONE',  ( 0.3913752891026081038, -1.689869761680007576, -0.4075552329090693093 ) ) ;
#28623 = DIRECTION ( 'NONE',  ( 0.4999551463232376758, -0.8660512985181132439, -1.377297506757674532E-17 ) ) ;
#28624 = DIRECTION ( 'NONE',  ( 1.000000000000000000, -0.000000000000000000, -0.000000000000000000 ) ) ;
#28625 = CARTESIAN_POINT ( 'NONE',  ( -9.828236692375560680E-17, -0.4262518876079541830, 0.09312799375524088985 ) ) ;
#28626 = CARTESIAN_POINT ( 'NONE',  ( 0.1188901005336925887, -1.412173384746612470, 0.5925880645485681608 ) ) ;
#28627 = COORDINATED_UNIVERSAL_TIME_OFFSET ( 0, 0, .AHEAD. ) ;
#28628 = CARTESIAN_POINT ( 'NONE',  ( 0.4176572489918210507, -1.668871684954134071, -0.5229746796350916993 ) ) ;
#28629 = EDGE_CURVE ( 'NONE', #16008, #24171, #10063, .T. ) ;
#28630 = CARTESIAN_POINT ( 'NONE',  ( -0.04760578872587735433, 0.4435171289962510643, 0.1893230556938514941 ) ) ;
#28631 = B_SPLINE_CURVE_WITH_KNOTS ( 'NONE', 3,
 ( #16867, #13362, #7365, #7167, #29204, #26139, #13756, #22434, #29602, #34962, #658, #26322, #28988, #16261, #25937, #19735, #38847, #32689, #38458, #16445, #19553, #13148 ),
 .UNSPECIFIED., .F., .F.,
 ( 4, 2, 2, 2, 2, 2, 2, 2, 2, 2, 4 ),
 ( 0.009671489109998996150, 0.01088255487380758793, 0.01209362063761617798, 0.01269915351952047300, 0.01330468640142476802, 0.01451575216523336154, 0.01572681792904195158, 0.01633235081094624661, 0.01693788369285054163, 0.01814894945665913167, 0.01936001522046771825 ),
 .UNSPECIFIED. ) ;
#28632 = VECTOR ( 'NONE', #13432, 39.37007874015748854 ) ;
#28633 = CARTESIAN_POINT ( 'NONE',  ( 0.4688079631758284016, -1.116561345930851656, 0.5688791344137259509 ) ) ;
#28634 = ORIENTED_EDGE ( 'NONE', *, *, #177, .F. ) ;
#28635 = CARTESIAN_POINT ( 'NONE',  ( 0.1879136253127565159, -0.5789011793442228049, 0.2920474488862616069 ) ) ;
#28636 = ORIENTED_EDGE ( 'NONE', *, *, #29512, .T. ) ;
#28637 = CARTESIAN_POINT ( 'NONE',  ( 0.03113248654051816583, -0.1960639381401260983, -0.03948331496955503200 ) ) ;
#28638 = SECURITY_CLASSIFICATION ( '', '', #3435 ) ;
#28639 = CARTESIAN_POINT ( 'NONE',  ( 0.2638696491212411122, -1.678849922788173910, 0.6249181099526833760 ) ) ;
#28640 = CARTESIAN_POINT ( 'NONE',  ( 0.5947882614772961318, -1.487164117345723735, 0.5703039760230342869 ) ) ;
#28642 = ORIENTED_EDGE ( 'NONE', *, *, #2602, .F. ) ;
#28641 = CARTESIAN_POINT ( 'NONE',  ( 0.4710977142973158394, -1.661186711027925256, -0.4170720528719219500 ) ) ;
#28643 = VECTOR ( 'NONE', #20892, 39.37007874015748143 ) ;
#28645 = ORIENTED_EDGE ( 'NONE', *, *, #33707, .T. ) ;
#28644 = ORIENTED_EDGE ( 'NONE', *, *, #18790, .T. ) ;
#28646 = CARTESIAN_POINT ( 'NONE',  ( 0.000000000000000000, -0.2276394436010286959, -0.1339480508475833498 ) ) ;
#28647 = ORIENTED_EDGE ( 'NONE', *, *, #33015, .T. ) ;
#28648 = CARTESIAN_POINT ( 'NONE',  ( -0.1617315581917542211, 0.4682256792068184570, 0.1178658435936994764 ) ) ;
#28649 = ADVANCED_FACE ( 'NONE', ( #38816 ), #2841, .T. ) ;
#28650 = APPROVAL ( #4535, 'UNKNOWN' ) ;
#28651 = DIRECTION ( 'NONE',  ( -0.4999551463232372317, 0.8660512985181135770, -0.000000000000000000 ) ) ;
#28652 = ORIENTED_EDGE ( 'NONE', *, *, #2602, .T. ) ;
#28653 = EDGE_CURVE ( 'NONE', #27272, #25698, #19705, .T. ) ;
#28654 = CARTESIAN_POINT ( 'NONE',  ( 0.2038982337730780858, -0.9000317451160128046, 0.6260891870533979997 ) ) ;
#28655 = CARTESIAN_POINT ( 'NONE',  ( 0.06924657340765605351, -0.5400045880099076934, 0.1408780685345814021 ) ) ;
#28656 = CARTESIAN_POINT ( 'NONE',  ( 0.5384178852093373102, -1.518839747657279693, 0.5610560271465162563 ) ) ;
#28657 = EDGE_CURVE ( 'NONE', #12308, #37890, #13380, .T. ) ;
#28658 = CARTESIAN_POINT ( 'NONE',  ( 0.5964376879960640032, -1.583813977042451526, -0.6035257017628796739 ) ) ;
#28659 = CARTESIAN_POINT ( 'NONE',  ( -0.04582889109739251426, -0.2312034125369010207, 0.4285435303321099565 ) ) ;
#28660 = VERTEX_POINT ( 'NONE', #35745 ) ;
#28661 = CARTESIAN_POINT ( 'NONE',  ( 0.6670706299876395518, -1.560988262821363159, 0.5986134368056421629 ) ) ;
#28662 = AXIS2_PLACEMENT_3D ( 'NONE', #4593, #11198, #13671 ) ;
#28663 = EDGE_LOOP ( 'NONE', ( #1100, #31223, #14391, #3537 ) ) ;
#28664 = CARTESIAN_POINT ( 'NONE',  ( 0.4361429146967321646, -1.593406671728312185, -0.6128992538235386034 ) ) ;
#28665 = CARTESIAN_POINT ( 'NONE',  ( 0.1351500142932794135, -0.5720763397125275818, 0.2394465910792453189 ) ) ;
#28666 = CARTESIAN_POINT ( 'NONE',  ( -0.002366742664566666259, -0.8470346775007634443, 0.1487544527304272002 ) ) ;
#28667 = APPLIED_APPROVAL_ASSIGNMENT ( #19955, ( #24074 ) ) ;
#28668 = CARTESIAN_POINT ( 'NONE',  ( -0.1743922129835733248, -0.5166151207188712791, 0.09999999999999961697 ) ) ;
#28669 = CARTESIAN_POINT ( 'NONE',  ( 0.03664605387828179933, -0.4430871221163645290, -0.1871485295462639309 ) ) ;
#28670 = CARTESIAN_POINT ( 'NONE',  ( 0.01926973937230214845, -1.027504089262102349, 0.6199911605063174180 ) ) ;
#28671 = CARTESIAN_POINT ( 'NONE',  ( 0.3725907112986628911, -0.9732892004818366471, 0.6614114956809742374 ) ) ;
#28672 = PERSON_AND_ORGANIZATION ( #28500, #32463 ) ;
#28673 = CARTESIAN_POINT ( 'NONE',  ( -0.1071618391680946858, -0.4882221650595564011, 0.3591756789878952638 ) ) ;
#28674 = ADVANCED_FACE ( 'NONE', ( #7556 ), #30875, .F. ) ;
#28675 = B_SPLINE_CURVE_WITH_KNOTS ( 'NONE', 3,
 ( #1616, #20736, #26492, #19909, #11252, #36138, #7948, #32656, #39240, #39028, #23434, #4651, #20521, #1030, #33262, #13541, #32445, #33056 ),
 .UNSPECIFIED., .F., .F.,
 ( 4, 2, 2, 2, 2, 2, 2, 2, 4 ),
 ( 0.0003425652276237501682, 0.001007165397454255675, 0.001671765567284761020, 0.002336365737115266364, 0.003000965906945771925, 0.003665566076776277486, 0.004330166246606782614, 0.004994766416437288609, 0.005659366586267793736 ),
 .UNSPECIFIED. ) ;
#28676 = CARTESIAN_POINT ( 'NONE',  ( -0.02869942827333585647, 0.4892109928530948282, -0.09550568247005984668 ) ) ;
#28677 = CARTESIAN_POINT ( 'NONE',  ( -0.01896968469603592389, 0.07379952543979995117, 0.5147668824877569271 ) ) ;
#28678 = ORIENTED_EDGE ( 'NONE', *, *, #25816, .F. ) ;
#28679 = FACE_OUTER_BOUND ( 'NONE', #9718, .T. ) ;
#28680 = LINE ( 'NONE', #547, #17755 ) ;
#28681 = DIRECTION ( 'NONE',  ( -0.4999999999999972800, -0.7041083277100139703, -0.5042137075183601436 ) ) ;
#28682 = ORIENTED_EDGE ( 'NONE', *, *, #703, .T. ) ;
#28683 = AXIS2_PLACEMENT_3D ( 'NONE', #13958, #26323, #23251 ) ;
#28684 = DIRECTION ( 'NONE',  ( 0.3181970600707391683, -0.9480245940703956320, -2.369716614345735130E-16 ) ) ;
#28685 = CARTESIAN_POINT ( 'NONE',  ( 0.06831029412767206099, -1.252103505662720773, 0.7560490987658511353 ) ) ;
#28687 = ORIENTED_EDGE ( 'NONE', *, *, #21203, .F. ) ;
#28686 = VERTEX_POINT ( 'NONE', #18865 ) ;
#28688 = CARTESIAN_POINT ( 'NONE',  ( 0.5185199569154549382, -1.918301849770578604, 0.5182417262812423209 ) ) ;
#28689 = FACE_OUTER_BOUND ( 'NONE', #21752, .T. ) ;
#28690 = APPLIED_SECURITY_CLASSIFICATION_ASSIGNMENT ( #30020, ( #40664 ) ) ;
#28691 = DIRECTION ( 'NONE',  ( 0.4999551463232371762, -0.8660512985181134660, 0.000000000000000000 ) ) ;
#28693 = CARTESIAN_POINT ( 'NONE',  ( -0.2399999999999999079, -3.941790907013290823, -0.3362780017083292772 ) ) ;
#28692 = CARTESIAN_POINT ( 'NONE',  ( 0.05269191099235399217, 0.4442874273374635141, 0.1490603884548275249 ) ) ;
#28694 = CARTESIAN_POINT ( 'NONE',  ( 0.04575185649130820292, -0.2311416656438095019, -0.4288096517596551305 ) ) ;
#28695 = ORIENTED_EDGE ( 'NONE', *, *, #38860, .T. ) ;
#28696 = CARTESIAN_POINT ( 'NONE',  ( 0.01562500000000001041, -0.4734555301001455718, 0.3484897634354066631 ) ) ;
#28697 = ORIENTED_EDGE ( 'NONE', *, *, #20550, .T. ) ;
#28698 = VERTEX_POINT ( 'NONE', #37360 ) ;
#28699 = TOROIDAL_SURFACE ( 'NONE', #12936, 1.986674066779348768, 0.01499999999999999944 ) ;
#28700 = CARTESIAN_POINT ( 'NONE',  ( 0.2111055010124828490, -0.8551966691801877740, 0.6642139276148122384 ) ) ;
#28701 = EDGE_LOOP ( 'NONE', ( #11975, #6377, #13195, #7620 ) ) ;
#28702 = ORIENTED_EDGE ( 'NONE', *, *, #28394, .F. ) ;
#28703 = CARTESIAN_POINT ( 'NONE',  ( 0.007612700501528337112, -0.5283205944668291076, 0.4322922080670053013 ) ) ;
#28704 = CARTESIAN_POINT ( 'NONE',  ( 0.4664867455706405153, -1.541371222339207980, 0.7051371147911057458 ) ) ;
#28706 = CARTESIAN_POINT ( 'NONE',  ( -0.1133687188271862989, -0.5183431199921479937, 0.3403596628069215368 ) ) ;
#28705 = CARTESIAN_POINT ( 'NONE',  ( 0.04040949304222755945, -0.7990836459010076664, 0.6824493494041665720 ) ) ;
#28707 = CARTESIAN_POINT ( 'NONE',  ( 0.3572222731481287661, -1.622781385286526934, -0.3671481750039431446 ) ) ;
#28708 = CARTESIAN_POINT ( 'NONE',  ( 0.4271525060574433152, -1.046616626432022024, 0.6356164445927319218 ) ) ;
#28709 = ORIENTED_EDGE ( 'NONE', *, *, #17073, .T. ) ;
#28710 = EDGE_CURVE ( 'NONE', #34346, #11425, #36362, .T. ) ;
#28711 = FACE_OUTER_BOUND ( 'NONE', #22600, .T. ) ;
#28712 = FACE_OUTER_BOUND ( 'NONE', #29032, .T. ) ;
#28713 = CARTESIAN_POINT ( 'NONE',  ( 0.3964953586213888492, -1.184310263668996388, 0.8231536074751556464 ) ) ;
#28714 = B_SPLINE_CURVE_WITH_KNOTS ( 'NONE', 3,
 ( #3196, #6280, #25002, #37535 ),
 .UNSPECIFIED., .F., .F.,
 ( 4, 4 ),
 ( 0.000000000000000000, 0.001608604910876098313 ),
 .UNSPECIFIED. ) ;
#28715 = CARTESIAN_POINT ( 'NONE',  ( -0.05634301242525831949, 0.2780425975185427667, 0.3652000572937671996 ) ) ;
#28716 = CARTESIAN_POINT ( 'NONE',  ( -0.2399999999999999079, -3.970782550070895311, -0.6634248229925526763 ) ) ;
#28717 = B_SPLINE_CURVE_WITH_KNOTS ( 'NONE', 3,
 ( #7649, #17316, #20213, #32738, #35425, #29659, #14017, #23700, #4959, #26592, #20005, #19788, #32328, #1113, #4145, #22908 ),
 .UNSPECIFIED., .F., .F.,
 ( 4, 2, 2, 2, 2, 2, 2, 4 ),
 ( 0.000000000000000000, 0.0006596505163732249016, 0.001319301032746449803, 0.001978951549119674705, 0.002638602065492899607, 0.003957903098239352012, 0.004617553614612577781, 0.005277204130985802683 ),
 .UNSPECIFIED. ) ;
#28718 = CARTESIAN_POINT ( 'NONE',  ( 0.08978098643734198914, 1.231844511688120125E-16, 0.3698489655878005045 ) ) ;
#28719 = VECTOR ( 'NONE', #16736, 39.37007874015748854 ) ;
#28720 = CARTESIAN_POINT ( 'NONE',  ( 0.2055745749294108637, -0.6303510842867390274, 0.3631342511460070033 ) ) ;
#28721 =( BOUNDED_SURFACE ( )  B_SPLINE_SURFACE ( 3, 2, ( 
 ( #27466, #37121, #34024 ),
 ( #18601, #5826, #18386 ),
 ( #30936, #9123, #27866 ),
 ( #16332, #9547, #40604 ),
 ( #10153, #31541, #35254 ),
 ( #21905, #37721, #28460 ),
 ( #22309, #9742, #34828 ),
 ( #335, #15521, #24969 ),
 ( #34430, #37501, #3169 ),
 ( #12421, #37932, #2975 ),
 ( #3357, #22724, #18819 ),
 ( #31158, #7053, #28871 ),
 ( #31752, #6636, #9326 ),
 ( #6250, #31361, #19012 ),
 ( #15709, #25803, #28076 ),
 ( #28256, #34640, #12617 ),
 ( #6438, #120, #25180 ),
 ( #19213, #25591, #22123 ),
 ( #15915, #9942, #12840 ),
 ( #3571, #25400, #16140 ),
 ( #28677, #6845, #544 ),
 ( #13041, #38118, #22512 ) ),
 .UNSPECIFIED., .F., .F., .T. ) 
 B_SPLINE_SURFACE_WITH_KNOTS ( ( 4, 2, 2, 2, 2, 2, 2, 2, 2, 2, 4 ),
 ( 3, 3 ),
 ( 0.002013519961495850458, 0.002780892266055758240, 0.003548264570615665588, 0.004315636875175573803, 0.004699323027455527477, 0.005083009179735481151, 0.005466695332015434824, 0.005850381484295388498, 0.006617753788855296714, 0.007385126093415204929, 0.008152498397975112276 ),
 ( 0.000000000000000000, 1.000000000000000000 ),
 .UNSPECIFIED. ) 
 GEOMETRIC_REPRESENTATION_ITEM ( )  RATIONAL_B_SPLINE_SURFACE ( (
 ( 1.000000000000000000, 0.7283825911960383204, 1.000000000000000000),
 ( 1.000000000000000000, 0.7404375345927353136, 1.000000000000000000),
 ( 1.000000000000000000, 0.7521483142435556601, 1.000000000000000000),
 ( 1.000000000000000000, 0.7744460733776885597, 1.000000000000000000),
 ( 1.000000000000000000, 0.7845612039380673863, 1.000000000000000000),
 ( 1.000000000000000000, 0.8022035258263486845, 1.000000000000000000),
 ( 1.000000000000000000, 0.8093965293322147314, 1.000000000000000000),
 ( 1.000000000000000000, 0.8169028692725253116, 1.000000000000000000),
 ( 1.000000000000000000, 0.8188329634861961637, 1.000000000000000000),
 ( 1.000000000000000000, 0.8214004505365417597, 1.000000000000000000),
 ( 1.000000000000000000, 0.8220602406261303674, 1.000000000000000000),
 ( 1.000000000000000000, 0.8220736605435321476, 1.000000000000000000),
 ( 1.000000000000000000, 0.8214126668415498989, 1.000000000000000000),
 ( 1.000000000000000000, 0.8188520474558501627, 1.000000000000000000),
 ( 1.000000000000000000, 0.8169545908333391004, 1.000000000000000000),
 ( 1.000000000000000000, 0.8094771004221675836, 1.000000000000000000),
 ( 1.000000000000000000, 0.8022723753808758129, 1.000000000000000000),
 ( 1.000000000000000000, 0.7845733350636272529, 1.000000000000000000),
 ( 1.000000000000000000, 0.7744472902496011280, 1.000000000000000000),
 ( 1.000000000000000000, 0.7522916829160717356, 1.000000000000000000),
 ( 1.000000000000000000, 0.7403553004667872139, 1.000000000000000000),
 ( 1.000000000000000000, 0.7283825911960402077, 1.000000000000000000) ) ) 
 REPRESENTATION_ITEM ( '' )  SURFACE ( )  );
#28722 = CARTESIAN_POINT ( 'NONE',  ( 0.4338848837222285537, -1.129391978085439341, 0.4668060154234752179 ) ) ;
#28723 = CARTESIAN_POINT ( 'NONE',  ( 0.03165525491262633634, -1.070880979729221805, 0.6191223686483765531 ) ) ;
#28724 = B_SPLINE_CURVE_WITH_KNOTS ( 'NONE', 3,
 ( #37446, #28809, #6177, #25116 ),
 .UNSPECIFIED., .F., .F.,
 ( 4, 4 ),
 ( 0.000000000000000000, 2.831411885517509102E-06 ),
 .UNSPECIFIED. ) ;
#28725 = CARTESIAN_POINT ( 'NONE',  ( 0.05076679145662148229, 0.4330939261214885594, -0.1921033382362662412 ) ) ;
#28726 = CARTESIAN_POINT ( 'NONE',  ( 0.1947422056511775024, -0.6388409797470162577, 0.3264359486978148928 ) ) ;
#28727 = CARTESIAN_POINT ( 'NONE',  ( 0.1477639946820497596, -0.8713623285363897297, 0.5125172420040071675 ) ) ;
#28728 = LINE ( 'NONE', #16371, #10040 ) ;
#28729 = DIRECTION ( 'NONE',  ( 1.000000000000000000, 0.000000000000000000, 0.000000000000000000 ) ) ;
#28730 = ORIENTED_EDGE ( 'NONE', *, *, #5363, .F. ) ;
#28731 = CARTESIAN_POINT ( 'NONE',  ( 0.4700139829499337396, -1.130594080169405657, -0.6582979126921139068 ) ) ;
#28732 = CARTESIAN_POINT ( 'NONE',  ( 0.4151543154610584652, -1.647056610985331959, -0.4022728307239534229 ) ) ;
#28733 = CARTESIAN_POINT ( 'NONE',  ( -0.05561170715395130637, -0.02038383341412248334, 0.4604752114371309379 ) ) ;
#28734 = ORIENTED_EDGE ( 'NONE', *, *, #36470, .F. ) ;
#28735 = CARTESIAN_POINT ( 'NONE',  ( -0.01895884884825219802, -0.2428741539084911250, -0.4598572020609195121 ) ) ;
#28736 = CARTESIAN_POINT ( 'NONE',  ( 0.1157895654112029854, -1.415802608199387524, 0.5684094141069466755 ) ) ;
#28737 = CARTESIAN_POINT ( 'NONE',  ( 0.4880577024640926909, -1.660084872155127789, 0.5232815315491193831 ) ) ;
#28738 = CARTESIAN_POINT ( 'NONE',  ( 0.2059273467974226668, -1.283046334493782359, -0.7462941026102624109 ) ) ;
#28739 = CARTESIAN_POINT ( 'NONE',  ( 0.4831561709721949871, -1.265801553224180420, 0.6869631041800865479 ) ) ;
#28741 = CARTESIAN_POINT ( 'NONE',  ( -0.2300000000000002875, 0.5182417262804733804, 0.1000000000000000194 ) ) ;
#28740 = CARTESIAN_POINT ( 'NONE',  ( -0.3000000000000000999, -3.941790907013290823, -0.4709369376873030477 ) ) ;
#28742 = CARTESIAN_POINT ( 'NONE',  ( 0.4924424051965485827, -1.082438949443123688, 0.5780025781777323735 ) ) ;
#28743 = VERTEX_POINT ( 'NONE', #6078 ) ;
#28744 = ITEM_DEFINED_TRANSFORMATION ( 'NONE', 'NONE', #4885,  #27819 ) ;
#28745 = CARTESIAN_POINT ( 'NONE',  ( 0.01894369509073403832, -0.9414322060572338779, 0.6002815649858233016 ) ) ;
#28746 = ORIENTED_EDGE ( 'NONE', *, *, #6247, .F. ) ;
#28747 = CARTESIAN_POINT ( 'NONE',  ( 0.04522317044199464925, -0.6176467172810933270, 0.3942814645560069331 ) ) ;
#28749 = CARTESIAN_POINT ( 'NONE',  ( 0.1110068091790888528, -0.9275713612966570709, 0.1181997008846571301 ) ) ;
#28748 = CARTESIAN_POINT ( 'NONE',  ( 0.08508713924366427539, -0.8316154493940929315, 0.1485430111225241878 ) ) ;
#28750 = CARTESIAN_POINT ( 'NONE',  ( 0.1960940348462748284, -2.001616103433511817, -0.3183625921796859326 ) ) ;
#28751 = VERTEX_POINT ( 'NONE', #38523 ) ;
#28752 = VERTEX_POINT ( 'NONE', #12464 ) ;
#28753 = EDGE_LOOP ( 'NONE', ( #38833, #2079, #4038, #35499 ) ) ;
#28754 = LINE ( 'NONE', #32222, #31983 ) ;
#28755 = EDGE_CURVE ( 'NONE', #12063, #5206, #7433, .T. ) ;
#28756 = CARTESIAN_POINT ( 'NONE',  ( 0.5669386463960099931, -1.503236241879966739, 0.5732355569184157673 ) ) ;
#28757 = AXIS2_PLACEMENT_3D ( 'NONE', #2684, #22039, #21623 ) ;
#28758 = VERTEX_POINT ( 'NONE', #28303 ) ;
#28759 = DIRECTION ( 'NONE',  ( 1.000000000000000000, 2.280301054154495132E-31, -1.664003471950577689E-31 ) ) ;
#28760 = EDGE_CURVE ( 'NONE', #10276, #5846, #25184, .T. ) ;
#28761 = CYLINDRICAL_SURFACE ( 'NONE', #33569, 0.01500000000000005843 ) ;
#28762 = LINE ( 'NONE', #28946, #17223 ) ;
#28763 = CARTESIAN_POINT ( 'NONE',  ( 0.07824279859864782805, -1.322120931084001416, 0.4675977987765131960 ) ) ;
#28764 = EDGE_CURVE ( 'NONE', #26316, #7093, #2869, .T. ) ;
#28765 = DIRECTION ( 'NONE',  ( -1.000000000000000000, 0.000000000000000000, 0.000000000000000000 ) ) ;
#28766 = FACE_OUTER_BOUND ( 'NONE', #9466, .T. ) ;
#28767 = EDGE_CURVE ( 'NONE', #40210, #2772, #33722, .T. ) ;
#28768 = CARTESIAN_POINT ( 'NONE',  ( 0.5117021325268811260, -1.128961434293810129, 0.8718124831259003171 ) ) ;
#28769 = CARTESIAN_POINT ( 'NONE',  ( 0.1864595955553456363, -0.7573173291059521750, 0.1477569985384105666 ) ) ;
#28770 = CARTESIAN_POINT ( 'NONE',  ( -0.01548846960721190873, 0.4730347584884290191, -0.2341461249027944058 ) ) ;
#28771 = CARTESIAN_POINT ( 'NONE',  ( -0.2399999999999999079, -3.609310082097819894, -0.4498340178114252352 ) ) ;
#28772 = PERSON_AND_ORGANIZATION ( #28500, #32463 ) ;
#28773 = DIRECTION ( 'NONE',  ( -0.4999999999999973910, 0.6535520748299027405, 0.5682162312760273837 ) ) ;
#28774 = FACE_OUTER_BOUND ( 'NONE', #13607, .T. ) ;
#28775 = CARTESIAN_POINT ( 'NONE',  ( 0.4544922177887179005, -1.243424314323010593, 0.6057417262809816627 ) ) ;
#28776 = CARTESIAN_POINT ( 'NONE',  ( 0.1864550573006002465, -0.7573172630633775437, 0.1903174488078394899 ) ) ;
#28777 = ADVANCED_FACE ( 'NONE', ( #35695 ), #38761, .F. ) ;
#28778 = APPLIED_PERSON_AND_ORGANIZATION_ASSIGNMENT ( #31957, #10146, ( #2626 ) ) ;
#28779 = CARTESIAN_POINT ( 'NONE',  ( 0.2936473109780965429, -1.729059834919730809, 0.6366410771178455663 ) ) ;
#28780 = CARTESIAN_POINT ( 'NONE',  ( -0.0002002802745677785610, -0.8521680098439298190, -0.04184250874055703978 ) ) ;
#28781 = CARTESIAN_POINT ( 'NONE',  ( 0.4243666725459965261, -1.591076223527387867, -0.4156371400837810537 ) ) ;
#28782 = FACE_OUTER_BOUND ( 'NONE', #1936, .T. ) ;
#28783 = CIRCLE ( 'NONE', #14979, 0.04330708661417336652 ) ;
#28784 = ORIENTED_EDGE ( 'NONE', *, *, #33303, .T. ) ;
#28785 = ORIENTED_EDGE ( 'NONE', *, *, #17728, .F. ) ;
#28786 = DIRECTION ( 'NONE',  ( 1.060606950627616897E-16, 6.122684696619992497E-17, 1.000000000000000000 ) ) ;
#28787 = ORIENTED_EDGE ( 'NONE', *, *, #17058, .F. ) ;
#28788 = CARTESIAN_POINT ( 'NONE',  ( -0.03664605387828190342, 0.04106737781738832582, 0.4792329708773127583 ) ) ;
#28789 = CARTESIAN_POINT ( 'NONE',  ( -0.05464101615137762630, -1.944084441611813707, -0.4562887203618206655 ) ) ;
#28790 = CARTESIAN_POINT ( 'NONE',  ( 0.6233463770837441853, -1.469195350882636975, 0.5327916358142242848 ) ) ;
#28792 = ORIENTED_EDGE ( 'NONE', *, *, #24256, .T. ) ;
#28791 = DIRECTION ( 'NONE',  ( 0.4999551463232372317, -0.8660512985181135770, 0.000000000000000000 ) ) ;
#28793 = ORIENTED_EDGE ( 'NONE', *, *, #27558, .F. ) ;
#28794 = CARTESIAN_POINT ( 'NONE',  ( 2.048885995248197414E-16, 0.2981948553318907735, -1.707404996040164512E-16 ) ) ;
#28795 = ORIENTED_EDGE ( 'NONE', *, *, #16453, .T. ) ;
#28796 = CARTESIAN_POINT ( 'NONE',  ( 0.2973691820713019185, -1.656741485100140521, 0.5759490276894616567 ) ) ;
#28798 = CARTESIAN_POINT ( 'NONE',  ( -0.04155248107635823446, -0.4416604393009568863, 0.1616214326753697139 ) ) ;
#28797 = DIRECTION ( 'NONE',  ( 0.000000000000000000, 0.000000000000000000, -1.000000000000000000 ) ) ;
#28799 = FACE_OUTER_BOUND ( 'NONE', #29294, .T. ) ;
#28800 = CARTESIAN_POINT ( 'NONE',  ( 0.1903632525096057571, -0.9196856789278203825, -0.08446770797961487831 ) ) ;
#28801 = CARTESIAN_POINT ( 'NONE',  ( 0.1134872160414416992, -1.333634162614142360, -0.3503315144562280659 ) ) ;
#28803 = EDGE_LOOP ( 'NONE', ( #3177, #11554, #10732, #19089 ) ) ;
#28802 = EDGE_LOOP ( 'NONE', ( #33747, #8630, #29300, #15313 ) ) ;
#28804 = DIRECTION ( 'NONE',  ( 0.000000000000000000, 0.000000000000000000, -1.000000000000000000 ) ) ;
#28805 = CARTESIAN_POINT ( 'NONE',  ( 0.2125266968579154203, -0.8550337035768073024, 0.3872327398333365589 ) ) ;
#28806 = CARTESIAN_POINT ( 'NONE',  ( 0.05999999999999990757, 0.2954784694557334168, 0.05188905557145093855 ) ) ;
#28807 = ADVANCED_FACE ( 'NONE', ( #29331 ), #28227, .T. ) ;
#28808 = CARTESIAN_POINT ( 'NONE',  ( 0.5837773615624999302, -1.483316297997810729, 0.6618257327465461026 ) ) ;
#28809 = CARTESIAN_POINT ( 'NONE',  ( 0.6985179347537009420, -1.438818273427901584, 0.5682411603540067357 ) ) ;
#28810 = CARTESIAN_POINT ( 'NONE',  ( -0.3000000000000000999, -3.237612445311622622, -0.5419983935656527141 ) ) ;
#28811 = EDGE_CURVE ( 'NONE', #20188, #28752, #7898, .T. ) ;
#28812 = CARTESIAN_POINT ( 'NONE',  ( 0.4582099881933914820, -1.160100326466038112, 0.4182417262808778013 ) ) ;
#28813 = EDGE_CURVE ( 'NONE', #8744, #20771, #283, .T. ) ;
#28814 = AXIS2_PLACEMENT_3D ( 'NONE', #27246, #20451, #35884 ) ;
#28815 = CARTESIAN_POINT ( 'NONE',  ( -0.002282498291095993656, -0.8555267327002353817, 0.1457185332388701293 ) ) ;
#28816 = FACE_OUTER_BOUND ( 'NONE', #38734, .T. ) ;
#28817 = CARTESIAN_POINT ( 'NONE',  ( -1.019575837292303166, -0.04310840302197994911, 0.08499999999999990896 ) ) ;
#28818 = DIRECTION ( 'NONE',  ( -1.000000000000000000, -0.000000000000000000, -0.000000000000000000 ) ) ;
#28819 = CARTESIAN_POINT ( 'NONE',  ( 0.2715891618659975193, -1.490554006250174757, 0.5182417262812423209 ) ) ;
#28820 = DIRECTION ( 'NONE',  ( 1.000000000000000000, 6.779273404243070203E-32, 4.314083075427408311E-32 ) ) ;
#28821 = CARTESIAN_POINT ( 'NONE',  ( -3.276078897458520021E-17, -0.4262518876079541830, 0.1281883534109924672 ) ) ;
#28822 = CARTESIAN_POINT ( 'NONE',  ( 0.1032092726473410188, -1.372029763476367403, 0.6793900317012312451 ) ) ;
#28823 = COORDINATED_UNIVERSAL_TIME_OFFSET ( 0, 0, .AHEAD. ) ;
#28824 = EDGE_CURVE ( 'NONE', #21571, #5485, #10811, .T. ) ;
#28825 = CARTESIAN_POINT ( 'NONE',  ( 0.3817504269947160078, -1.726033828776056378, 0.4251703030630522018 ) ) ;
#28826 = CARTESIAN_POINT ( 'NONE',  ( 0.3674944553547283554, -1.749262848119110814, -0.6770320976117242262 ) ) ;
#28827 = CARTESIAN_POINT ( 'NONE',  ( -0.05279755784604217572, 0.4315508301037739858, 0.1821553064136667566 ) ) ;
#28828 = CARTESIAN_POINT ( 'NONE',  ( 0.3678947686560505304, -1.763302576097276697, -0.5854506657463419694 ) ) ;
#28829 = ORIENTED_EDGE ( 'NONE', *, *, #4851, .F. ) ;
#28830 = DIRECTION ( 'NONE',  ( 0.000000000000000000, -0.9510565162951568619, -0.3090169943749376258 ) ) ;
#28831 = ORIENTED_EDGE ( 'NONE', *, *, #32605, .T. ) ;
#28832 = DIRECTION ( 'NONE',  ( -1.000000000000000000, -2.341930812374887555E-31, 1.664003471950578127E-31 ) ) ;
#28833 = B_SPLINE_CURVE_WITH_KNOTS ( 'NONE', 3,
 ( #25561, #28648, #13197, #35006, #3933, #38091, #9910, #28433, #702, #25769 ),
 .UNSPECIFIED., .F., .F.,
 ( 4, 2, 2, 2, 4 ),
 ( 7.269816092101098720E-18, 0.0003553525228749281105, 0.0007107050457498489569, 0.001066057568624769912, 0.001421410091499690758 ),
 .UNSPECIFIED. ) ;
#28834 = CARTESIAN_POINT ( 'NONE',  ( 0.2607738564055140928, -1.679248230842525169, 0.5808287157383641430 ) ) ;
#28835 = CARTESIAN_POINT ( 'NONE',  ( 0.5448905143716247235, -1.417074983688033640, 0.7694088827245902928 ) ) ;
#28837 = ORIENTED_EDGE ( 'NONE', *, *, #39683, .T. ) ;
#28836 = CARTESIAN_POINT ( 'NONE',  ( 0.5254156872246980026, -1.636223382584907071, -0.4246476935767348748 ) ) ;
#28839 = EDGE_LOOP ( 'NONE', ( #18824, #40273, #2999, #24394 ) ) ;
#28838 = ORIENTED_EDGE ( 'NONE', *, *, #6175, .F. ) ;
#28840 = CARTESIAN_POINT ( 'NONE',  ( 0.4897592102757906130, -1.696528537887749932, -0.5984293649392183889 ) ) ;
#28841 = VERTEX_POINT ( 'NONE', #33219 ) ;
#28842 = DIRECTION ( 'NONE',  ( 1.000000000000000000, -0.000000000000000000, -0.000000000000000000 ) ) ;
#28843 = DIRECTION ( 'NONE',  ( -1.387778780781449225E-15, 6.402768735150633127E-16, -1.000000000000000000 ) ) ;
#28844 = DIRECTION ( 'NONE',  ( -1.000000000000000000, -0.000000000000000000, -0.000000000000000000 ) ) ;
#28845 = ORIENTED_EDGE ( 'NONE', *, *, #33417, .F. ) ;
#28846 = CARTESIAN_POINT ( 'NONE',  ( 0.09262226466725992369, -0.7756921188983920690, 0.2845593417137921577 ) ) ;
#28847 = EDGE_CURVE ( 'NONE', #11941, #1103, #35900, .T. ) ;
#28848 = CARTESIAN_POINT ( 'NONE',  ( -2.070754768975508586, -0.09959325338431662678, 0.3600000000000021516 ) ) ;
#28849 = CARTESIAN_POINT ( 'NONE',  ( 0.5400961048456246472, -1.518900631274988866, 0.5940360734052072544 ) ) ;
#28850 = ORIENTED_EDGE ( 'NONE', *, *, #34396, .T. ) ;
#28851 = CARTESIAN_POINT ( 'NONE',  ( 0.4621583407840581526, -1.042755713779721649, -0.5155029497116575543 ) ) ;
#28852 = CARTESIAN_POINT ( 'NONE',  ( -0.1638686671686519769, 0.5092269732921813619, 0.1413937977834208159 ) ) ;
#28853 = CARTESIAN_POINT ( 'NONE',  ( -0.1604632851855366527, 0.4983239941852555810, 0.1050370266831589100 ) ) ;
#28854 = EDGE_CURVE ( 'NONE', #26101, #39763, #23016, .T. ) ;
#28855 = FACE_OUTER_BOUND ( 'NONE', #23548, .T. ) ;
#28856 = CARTESIAN_POINT ( 'NONE',  ( 0.6587214591109057382, -1.529505462609035193, 0.7312054128241273210 ) ) ;
#28857 = FACE_OUTER_BOUND ( 'NONE', #17947, .T. ) ;
#28858 = CARTESIAN_POINT ( 'NONE',  ( 0.3799940994133568228, -1.120217080746673588, 0.7999332164991961314 ) ) ;
#28859 = CARTESIAN_POINT ( 'NONE',  ( 0.05083665881508948187, -0.4630607685881619751, 0.09936361682460788380 ) ) ;
#28860 = CARTESIAN_POINT ( 'NONE',  ( -0.2746410161513779258, -2.477126460671948749, -0.4732852368073287574 ) ) ;
#28861 = DIMENSIONAL_EXPONENTS ( 1.000000000000000000, 0.000000000000000000, 0.000000000000000000, 0.000000000000000000, 0.000000000000000000, 0.000000000000000000, 0.000000000000000000 ) ;
#28862 = DIRECTION ( 'NONE',  ( 1.000000000000000000, -7.012307549337885980E-13, -2.434866152052794803E-12 ) ) ;
#28863 = CARTESIAN_POINT ( 'NONE',  ( 0.05963972588713747913, -1.330888851906829595, 0.5826259623951950406 ) ) ;
#28864 = CARTESIAN_POINT ( 'NONE',  ( 0.4989999315605664343, -1.099494619349625113, 0.6223919996226902063 ) ) ;
#28865 = APPROVAL_ROLE ( '' ) ;
#28866 = EDGE_CURVE ( 'NONE', #12909, #9415, #36511, .T. ) ;
#28867 = CARTESIAN_POINT ( 'NONE',  ( -0.1061036098701638175, -0.4827967145417200179, 0.3599999999999999867 ) ) ;
#28868 = EDGE_CURVE ( 'NONE', #29847, #2400, #20893, .T. ) ;
#28869 = ADVANCED_FACE ( 'NONE', ( #5223 ), #17774, .T. ) ;
#28870 = CARTESIAN_POINT ( 'NONE',  ( -0.03662792686184409424, 0.4685177067346118496, -0.1089945633920606921 ) ) ;
#28871 = CARTESIAN_POINT ( 'NONE',  ( -0.05634490452572834401, 0.005064009952713930708, 0.4588782462578064880 ) ) ;
#28872 = ORIENTED_EDGE ( 'NONE', *, *, #8168, .T. ) ;
#28873 = CARTESIAN_POINT ( 'NONE',  ( 0.4330280987197626663, -1.579361639735390010, 0.5968389982114721271 ) ) ;
#28874 = CARTESIAN_POINT ( 'NONE',  ( 0.002296835029420926742, -0.5198933010532099663, 0.1467999231854336672 ) ) ;
#28875 = CARTESIAN_POINT ( 'NONE',  ( 0.1852083516168847588, -0.8428145337524144409, 0.2138870730384467567 ) ) ;
#28876 = ORIENTED_EDGE ( 'NONE', *, *, #39057, .F. ) ;
#28877 = CARTESIAN_POINT ( 'NONE',  ( 0.05567535398968421340, -1.335339640988971288, 0.4687417262808780127 ) ) ;
#28878 = CARTESIAN_POINT ( 'NONE',  ( 0.6802496923668470696, -1.403733334520502973, 0.6188728273484885856 ) ) ;
#28880 = EDGE_LOOP ( 'NONE', ( #29596, #33689, #13741, #23277, #29974, #24070 ) ) ;
#28879 = EDGE_LOOP ( 'NONE', ( #32921, #23966, #4426, #17593 ) ) ;
#28881 = CARTESIAN_POINT ( 'NONE',  ( -0.02000000000000000042, -1.538828486247671101, 0.2167077994389897955 ) ) ;
#28882 = DIRECTION ( 'NONE',  ( 0.8660512985181136880, 0.4999551463232369541, 0.000000000000000000 ) ) ;
#28883 = CARTESIAN_POINT ( 'NONE',  ( 0.03171102739522826258, 0.4481073524712099188, 0.2027236177532184824 ) ) ;
#28884 = CARTESIAN_POINT ( 'NONE',  ( 0.03875523708677781898, -0.3062771359410657035, -0.3649060648845485200 ) ) ;
#28885 = EDGE_LOOP ( 'NONE', ( #14074, #1299, #30056, #16854 ) ) ;
#28886 = CARTESIAN_POINT ( 'NONE',  ( 0.4212239597017563009, -1.699686401043103867, 0.5682417262808792113 ) ) ;
#28887 = CARTESIAN_POINT ( 'NONE',  ( 0.2513281675165960349, -0.9200942028859548927, 0.7135546038586990658 ) ) ;
#28888 = CARTESIAN_POINT ( 'NONE',  ( 0.03721266748343820402, -0.6194934239485735405, 0.6037397677565615739 ) ) ;
#28889 = CARTESIAN_POINT ( 'NONE',  ( 0.08524078840219724562, -0.5428247996486972315, 0.1539524137301193363 ) ) ;
#28891 = CARTESIAN_POINT ( 'NONE',  ( -0.1154414454259565792, -0.5279056935456777344, 0.3241024189951781653 ) ) ;
#28890 = CARTESIAN_POINT ( 'NONE',  ( 0.4819756813572292908, -1.590155287500744086, -0.4462383725080293351 ) ) ;
#28892 = CARTESIAN_POINT ( 'NONE',  ( 0.6091039633998347469, -1.477405756664260439, 0.4854686549615686575 ) ) ;
#28893 = CARTESIAN_POINT ( 'NONE',  ( 0.4531532885747490691, -1.103993380834564775, 0.5911741900463310939 ) ) ;
#28894 = ORIENTED_EDGE ( 'NONE', *, *, #19808, .F. ) ;
#28895 = ADVANCED_FACE ( 'NONE', ( #10132 ), #32424, .T. ) ;
#28896 = CARTESIAN_POINT ( 'NONE',  ( 0.6487533847785609264, -1.557452555468215483, -0.6098442386003093407 ) ) ;
#28897 = CARTESIAN_POINT ( 'NONE',  ( 0.1887417687075507722, -0.4595378961884863389, 0.1473935149025172031 ) ) ;
#28898 = ADVANCED_FACE ( 'NONE', ( #16317 ), #19791, .T. ) ;
#28899 = CARTESIAN_POINT ( 'NONE',  ( -0.05544444631433822351, 0.2544607094502333577, -0.3847718460475671454 ) ) ;
#28900 = B_SPLINE_CURVE_WITH_KNOTS ( 'NONE', 3,
 ( #5779, #15461, #15247, #27802, #40546, #12366, #29615, #22450, #1078, #19749, #32491, #32097, #25952, #31906, #7179, #29420 ),
 .UNSPECIFIED., .F., .F.,
 ( 4, 2, 2, 2, 2, 2, 2, 4 ),
 ( 0.002977950600791165556, 0.003350110441325639555, 0.003722270281860113553, 0.004094430122394587986, 0.004466589962929061984, 0.004838749803463535983, 0.005210909643998009981, 0.005955229325066958845 ),
 .UNSPECIFIED. ) ;
#28901 = DIRECTION ( 'NONE',  ( 0.5000000000000009992, -0.7308273574226402669, -0.4646411234949391900 ) ) ;
#28902 = PLANE ( 'NONE',  #4306 ) ;
#28903 = CARTESIAN_POINT ( 'NONE',  ( 0.3225930820597290305, -0.8396780885765841029, 0.6764912411861826458 ) ) ;
#28904 = CARTESIAN_POINT ( 'NONE',  ( 0.4572296806421124460, -1.116135140744203502, 0.5564961385877081890 ) ) ;
#28905 = CARTESIAN_POINT ( 'NONE',  ( 0.03592955808354850872, -1.097415845682047753, 0.6391787347605660807 ) ) ;
#28906 = CIRCLE ( 'NONE', #23673, 0.009999999999999995004 ) ;
#28907 = CARTESIAN_POINT ( 'NONE',  ( 0.05201782277452383224, 0.4527080286589780234, -0.1280848763234450904 ) ) ;
#28908 = CARTESIAN_POINT ( 'NONE',  ( 0.1925648626342071068, -0.7537655587791137757, 0.3141518395702517785 ) ) ;
#28909 = CARTESIAN_POINT ( 'NONE',  ( 0.3182721343743615816, -1.037109716264222659, 0.7330233950017801536 ) ) ;
#28910 = CARTESIAN_POINT ( 'NONE',  ( 0.03868649100028160454, -0.3066017772948808062, 0.3648306000529322746 ) ) ;
#28911 = FACE_BOUND ( 'NONE', #145, .T. ) ;
#28912 = AXIS2_PLACEMENT_3D ( 'NONE', #22313, #6642, #21513 ) ;
#28913 = ORIENTED_EDGE ( 'NONE', *, *, #27253, .T. ) ;
#28914 = DIRECTION ( 'NONE',  ( -0.000000000000000000, -0.5365213554527455964, 0.8438867430782097667 ) ) ;
#28915 = CARTESIAN_POINT ( 'NONE',  ( 0.5561777791303107454, -1.388654548445044323, 0.7524667234028521445 ) ) ;
#28916 = CARTESIAN_POINT ( 'NONE',  ( 0.07550739411094989362, -0.8311898289549712882, 0.1457185332388705179 ) ) ;
#28917 = CARTESIAN_POINT ( 'NONE',  ( 0.3704697912810962501, -1.166474544107111377, 0.4182417262808778013 ) ) ;
#28918 = PERSON ( 'NAUO-PER9', 'UNSPECIFIED', 'UNSPECIFIED', ('UNSPECIFIED'), ('UNSPECIFIED'), ('UNSPECIFIED') ) ;
#28919 = ORIENTED_EDGE ( 'NONE', *, *, #17936, .T. ) ;
#28920 = CARTESIAN_POINT ( 'NONE',  ( -0.1638630105338990950, 0.5092090815894948497, 0.3148090297061075793 ) ) ;
#28921 = CARTESIAN_POINT ( 'NONE',  ( 0.1882419910544414765, -0.5601865779007185742, 0.2791098525572430766 ) ) ;
#28922 = CARTESIAN_POINT ( 'NONE',  ( 0.4650133494175291982, -1.133480851973431847, -0.6660426939124519663 ) ) ;
#28923 = CARTESIAN_POINT ( 'NONE',  ( -0.3000000000000000999, -2.878813263491020180, -0.3823467908819087602 ) ) ;
#28924 = CARTESIAN_POINT ( 'NONE',  ( 0.3363348836112549645, -1.066364408820902998, 0.7268484058858328822 ) ) ;
#28926 = DIRECTION ( 'NONE',  ( 1.000000000000000000, 1.138269997360101095E-15, -8.881784197001243449E-16 ) ) ;
#28925 = DIRECTION ( 'NONE',  ( -1.664003471950567617E-31, -0.8983234858820536850, 0.4393346272634515159 ) ) ;
#28927 = CARTESIAN_POINT ( 'NONE',  ( 0.3459602365858145401, -1.002069219538038736, 0.6041729112776661470 ) ) ;
#28928 = ORIENTED_EDGE ( 'NONE', *, *, #23993, .T. ) ;
#28929 = COORDINATED_UNIVERSAL_TIME_OFFSET ( 0, 0, .AHEAD. ) ;
#28930 = CARTESIAN_POINT ( 'NONE',  ( 0.5509968806096897653, -1.899553531783569449, 0.5182417262812423209 ) ) ;
#28931 = VERTEX_POINT ( 'NONE', #35627 ) ;
#28932 = ORIENTED_EDGE ( 'NONE', *, *, #17255, .T. ) ;
#28933 = CARTESIAN_POINT ( 'NONE',  ( 0.4136565266000814534, -1.589555752243668962, 0.5742607991556297753 ) ) ;
#28935 = FACE_OUTER_BOUND ( 'NONE', #5320, .T. ) ;
#28934 = CARTESIAN_POINT ( 'NONE',  ( 0.08600443180144776156, -0.7812038045049116697, 0.06558878796052790283 ) ) ;
#28936 = CARTESIAN_POINT ( 'NONE',  ( 0.06911925242283332993, -0.5409396888079850418, 0.1263946519415101166 ) ) ;
#28937 = EDGE_LOOP ( 'NONE', ( #10673, #23347 ) ) ;
#28938 = AXIS2_PLACEMENT_3D ( 'NONE', #4615, #38996, #33022 ) ;
#28939 = EDGE_LOOP ( 'NONE', ( #37724, #35663, #7578, #5752 ) ) ;
#28940 = CARTESIAN_POINT ( 'NONE',  ( 0.4898967846823991668, -1.079624215837351242, 0.5968486766476291949 ) ) ;
#28941 = CARTESIAN_POINT ( 'NONE',  ( 0.5664215386550598419, -1.503089260598527321, 0.5634370993589044030 ) ) ;
#28942 = EDGE_LOOP ( 'NONE', ( #857, #33915, #36208, #9713, #10990 ) ) ;
#28943 = CARTESIAN_POINT ( 'NONE',  ( 0.07172784347629639068, -1.333591952913690593, 0.4986392271462748438 ) ) ;
#28944 = CARTESIAN_POINT ( 'NONE',  ( 0.02063935039522163395, -1.619419422640626438, -0.3749979873294493338 ) ) ;
#28945 = TOROIDAL_SURFACE ( 'NONE', #26318, 1.986674066779348768, 0.01499999999999999944 ) ;
#28946 = CARTESIAN_POINT ( 'NONE',  ( -0.2789010053595598060, 0.4834754829570387935, 0.3749999999999999445 ) ) ;
#28947 = ORIENTED_EDGE ( 'NONE', *, *, #39069, .F. ) ;
#28948 = DIRECTION ( 'NONE',  ( 7.771561172376107616E-16, -7.170354002788761615E-17, 1.000000000000000000 ) ) ;
#28949 = AXIS2_PLACEMENT_3D ( 'NONE', #2586, #33863, #15339 ) ;
#28950 = CARTESIAN_POINT ( 'NONE',  ( 0.3262646141370696418, -1.756421352762273846, 0.5762462443359027686 ) ) ;
#28951 = CARTESIAN_POINT ( 'NONE',  ( 0.08657376948451865617, -0.8126112693459484060, 0.01976600836222000904 ) ) ;
#28952 = CARTESIAN_POINT ( 'NONE',  ( 0.5598795747092503161, -1.507486333647360510, 0.5722829373276135945 ) ) ;
#28953 = CARTESIAN_POINT ( 'NONE',  ( 0.1886993031460024173, -1.963322156380002292, -0.6958836544861118911 ) ) ;
#28954 = DIRECTION ( 'NONE',  ( 0.000000000000000000, 0.000000000000000000, -1.000000000000000000 ) ) ;
#28955 = CARTESIAN_POINT ( 'NONE',  ( 0.1102224200671288595, -1.400663116118479490, 0.6358304045325068321 ) ) ;
#28956 = APPROVAL_DATE_TIME ( #5221, #31795 ) ;
#28957 = CARTESIAN_POINT ( 'NONE',  ( 0.6426786216763176185, -1.413792888462838127, -0.6263067080391584440 ) ) ;
#28958 = CARTESIAN_POINT ( 'NONE',  ( 0.5965761245944036784, -1.493465029535157029, 0.5182417262812423209 ) ) ;
#28959 = CARTESIAN_POINT ( 'NONE',  ( -0.1129900121204313601, -0.5167580615070225258, 0.3146079272632537616 ) ) ;
#28960 = CARTESIAN_POINT ( 'NONE',  ( 0.4744622997635568606, -1.208877113836489547, 0.5084237165177825091 ) ) ;
#28961 = FACE_OUTER_BOUND ( 'NONE', #39915, .T. ) ;
#28962 = CARTESIAN_POINT ( 'NONE',  ( 0.2426062050407847281, -1.584949062848913348, 0.8214247301831154591 ) ) ;
#28963 = CARTESIAN_POINT ( 'NONE',  ( 0.5844093222531523413, -1.481270550429968136, -0.4312484634772048575 ) ) ;
#28964 = CARTESIAN_POINT ( 'NONE',  ( -0.02000000000000000042, -1.599201040860868339, 0.1842182323853684411 ) ) ;
#28965 = AXIS2_PLACEMENT_3D ( 'NONE', #28143, #5284, #33686 ) ;
#28966 = CARTESIAN_POINT ( 'NONE',  ( 0.03650581953630530757, -0.2290855126858360180, 0.4575806651622388865 ) ) ;
#28967 = CARTESIAN_POINT ( 'NONE',  ( -0.02000000000000000042, -2.196071624283071788, -0.8624000883860228894 ) ) ;
#28968 = VERTEX_POINT ( 'NONE', #35427 ) ;
#28969 = VERTEX_POINT ( 'NONE', #13622 ) ;
#28970 = AXIS2_PLACEMENT_3D ( 'NONE', #27933, #18260, #30805 ) ;
#28971 = DIRECTION ( 'NONE',  ( 2.682900528199988315E-31, -0.9510565162951527540, 0.3090169943749503378 ) ) ;
#28972 = ORIENTED_EDGE ( 'NONE', *, *, #32847, .T. ) ;
#28973 = AXIS2_PLACEMENT_3D ( 'NONE', #21144, #18054, #30607 ) ;
#28974 = DIRECTION ( 'NONE',  ( 2.532366176626899733E-12, -0.3090169943749518366, -0.9510565162951520879 ) ) ;
#28975 = CARTESIAN_POINT ( 'NONE',  ( 0.4480646913441768131, -1.099213350020603164, -0.6275147848854655264 ) ) ;
#28976 = AXIS2_PLACEMENT_3D ( 'NONE', #12385, #31329, #9502 ) ;
#28977 = CARTESIAN_POINT ( 'NONE',  ( 0.4451373613274108854, -1.213283134829647114, 0.7682095407564263345 ) ) ;
#28978 = EDGE_CURVE ( 'NONE', #31816, #21190, #30368, .T. ) ;
#28980 = ORIENTED_EDGE ( 'NONE', *, *, #22051, .T. ) ;
#28979 = DIRECTION ( 'NONE',  ( 1.000000000000000000, -0.000000000000000000, -0.000000000000000000 ) ) ;
#28981 = CARTESIAN_POINT ( 'NONE',  ( 0.4865355734717750624, -1.097175741254786452, 0.7494200075675998551 ) ) ;
#28982 = CARTESIAN_POINT ( 'NONE',  ( 0.3619943274630011421, -1.737009005337970313, -0.5415504813999939548 ) ) ;
#28983 = VERTEX_POINT ( 'NONE', #22910 ) ;
#28984 = DIRECTION ( 'NONE',  ( 0.4999551463232372317, -0.8660512985181133550, 0.000000000000000000 ) ) ;
#28985 = ORIENTED_EDGE ( 'NONE', *, *, #2430, .T. ) ;
#28986 = CARTESIAN_POINT ( 'NONE',  ( 0.2904216923373793002, -1.605717452676975077, 0.8056108489146471818 ) ) ;
#28988 = CARTESIAN_POINT ( 'NONE',  ( 0.1117172404438186717, -0.8790865271448059515, -0.001403887437530376659 ) ) ;
#28987 = CARTESIAN_POINT ( 'NONE',  ( -0.02000000000000000042, -2.071870001606465284, -0.3441689154348898660 ) ) ;
#28989 = PLANE ( 'NONE',  #10920 ) ;
#28990 = CARTESIAN_POINT ( 'NONE',  ( 0.3926032618789407347, -1.756026311479913948, -0.5284552501753293496 ) ) ;
#28991 = CARTESIAN_POINT ( 'NONE',  ( 0.001255696819123910566, -1.915471855958320146, -0.3089908321627916066 ) ) ;
#28993 = ORIENTED_EDGE ( 'NONE', *, *, #17973, .F. ) ;
#28992 = ORIENTED_EDGE ( 'NONE', *, *, #18311, .F. ) ;
#28994 = VECTOR ( 'NONE', #32219, 39.37007874015748143 ) ;
#28995 = CARTESIAN_POINT ( 'NONE',  ( -2.112273405726188513E-14, -2.183180860297921466, -0.4937760292030871079 ) ) ;
#28996 = CARTESIAN_POINT ( 'NONE',  ( 0.1109049718728861156, -0.9286333055842311834, 0.1443021394692906578 ) ) ;
#28997 = DIRECTION ( 'NONE',  ( 0.000000000000000000, 0.000000000000000000, -1.000000000000000000 ) ) ;
#28998 = CARTESIAN_POINT ( 'NONE',  ( 0.5582418957589161401, -1.431870684052794385, 0.7524718376146050103 ) ) ;
#28999 = EDGE_CURVE ( 'NONE', #16603, #4682, #20024, .T. ) ;
#29000 = CARTESIAN_POINT ( 'NONE',  ( 0.3828917794701993671, -1.259344239476607452, 0.5976400823309563348 ) ) ;
#29001 = CARTESIAN_POINT ( 'NONE',  ( -0.2399999999999999079, -2.289343986263487896, -0.7686455968847020204 ) ) ;
#29002 = APPLIED_PERSON_AND_ORGANIZATION_ASSIGNMENT ( #37194, #34297, ( #17475 ) ) ;
#29003 = AXIS2_PLACEMENT_3D ( 'NONE', #13761, #32276, #26327 ) ;
#29004 = CARTESIAN_POINT ( 'NONE',  ( 0.05634304521267768928, -2.731847993664263218E-15, -0.4588823192046729837 ) ) ;
#29005 = CARTESIAN_POINT ( 'NONE',  ( -0.1668894944043932960, 0.4852776769345376606, 0.3312153816179764232 ) ) ;
#29006 = VECTOR ( 'NONE', #40376, 39.37007874015748854 ) ;
#29007 = CARTESIAN_POINT ( 'NONE',  ( -2.112273405726188513E-14, -2.183180860297921466, -0.4937760292030871079 ) ) ;
#29008 = CARTESIAN_POINT ( 'NONE',  ( 0.1499999999999994671, 0.5198120922912046193, -0.07362328916749301400 ) ) ;
#29009 = CARTESIAN_POINT ( 'NONE',  ( 0.4030327056921976792, -1.680968334469209680, -0.4031266960524464982 ) ) ;
#29010 = SECURITY_CLASSIFICATION_LEVEL ( 'unclassified' ) ;
#29011 = AXIS2_PLACEMENT_3D ( 'NONE', #14647, #27215, #33559 ) ;
#29012 = CARTESIAN_POINT ( 'NONE',  ( 0.01896931156526606224, -0.3622781579086280512, 0.3730773604463891169 ) ) ;
#29013 = CARTESIAN_POINT ( 'NONE',  ( 0.1808332695554492053, -0.4986102965419587085, 0.1174482592749270665 ) ) ;
#29014 = CARTESIAN_POINT ( 'NONE',  ( 0.1991480113865206902, -2.054949600705703983, -0.6841806413415666421 ) ) ;
#29015 = DIRECTION ( 'NONE',  ( 1.000000000000000000, -0.000000000000000000, -0.000000000000000000 ) ) ;
#29016 = DIRECTION ( 'NONE',  ( 4.622231866529356468E-33, -0.6954292836768481978, -0.7185945389471769529 ) ) ;
#29017 = CARTESIAN_POINT ( 'NONE',  ( -0.01548846960707503904, 0.5203207976467937312, 0.08861466064782108631 ) ) ;
#29018 = LINE ( 'NONE', #25546, #40544 ) ;
#29019 = EDGE_CURVE ( 'NONE', #19020, #16852, #37011, .T. ) ;
#29020 = ADVANCED_FACE ( 'NONE', ( #32540 ), #4358, .T. ) ;
#29021 = LINE ( 'NONE', #689, #6679 ) ;
#29022 = ORIENTED_EDGE ( 'NONE', *, *, #14430, .F. ) ;
#29023 = CARTESIAN_POINT ( 'NONE',  ( 0.4688079631758284016, -1.116561345930851656, 0.5688791344137259509 ) ) ;
#29024 = CARTESIAN_POINT ( 'NONE',  ( 0.2662821865085873707, -1.672322712245089882, 0.6834728152926629052 ) ) ;
#29025 = ADVANCED_FACE ( 'NONE', ( #35839 ), #23914, .T. ) ;
#29026 = CIRCLE ( 'NONE', #7993, 0.04999999999999994726 ) ;
#29027 = CARTESIAN_POINT ( 'NONE',  ( 0.1313240903384290670, -0.5586677835130641201, 0.1977070789115515925 ) ) ;
#29028 = EDGE_CURVE ( 'NONE', #10991, #34346, #12066, .T. ) ;
#29030 = ORIENTED_EDGE ( 'NONE', *, *, #18803, .T. ) ;
#29029 = CARTESIAN_POINT ( 'NONE',  ( 0.1273306340341417431, -1.236045459326737150, -0.5155029497116575543 ) ) ;
#29031 = ADVANCED_FACE ( 'NONE', ( #9748 ), #6146, .T. ) ;
#29033 = ORIENTED_EDGE ( 'NONE', *, *, #32055, .F. ) ;
#29032 = EDGE_LOOP ( 'NONE', ( #28331, #12814, #5341, #7780, #34339, #18194 ) ) ;
#29034 = CARTESIAN_POINT ( 'NONE',  ( -0.05464101615137761936, -2.039246558356380135, -0.5681570558249129377 ) ) ;
#29035 = AXIS2_PLACEMENT_3D ( 'NONE', #37342, #7984, #17467 ) ;
#29036 = ORIENTED_EDGE ( 'NONE', *, *, #8194, .T. ) ;
#29037 = CIRCLE ( 'NONE', #1520, 0.04330708661417322775 ) ;
#29038 = CARTESIAN_POINT ( 'NONE',  ( -0.1399999999999997358, 0.000000000000000000, 0.000000000000000000 ) ) ;
#29039 = CARTESIAN_POINT ( 'NONE',  ( 0.05999999999999990757, 0.1428018198284763673, -0.2638325989215043466 ) ) ;
#29040 = AXIS2_PLACEMENT_3D ( 'NONE', #12627, #25191, #37735 ) ;
#29041 = CARTESIAN_POINT ( 'NONE',  ( 0.05999999999999990757, -0.3852620677835773555, -0.4748740771268961103 ) ) ;
#29042 = ORIENTED_EDGE ( 'NONE', *, *, #13025, .F. ) ;
#29043 = CARTESIAN_POINT ( 'NONE',  ( 0.08560004179328287166, -0.7895966635341131745, 0.1829049723430900276 ) ) ;
#29044 = CARTESIAN_POINT ( 'NONE',  ( 0.08990936761269285871, -0.5436479961250832993, 0.1408780685345787931 ) ) ;
#29045 = CARTESIAN_POINT ( 'NONE',  ( 0.5285810829098267494, -1.495792263264798860, 0.7113523899947146178 ) ) ;
#29046 = CARTESIAN_POINT ( 'NONE',  ( -0.09908070219615519592, -0.09959325338431371244, 0.09550516381870127747 ) ) ;
#29047 = ADVANCED_FACE ( 'NONE', ( #26021 ), #5082, .T. ) ;
#29048 = FACE_OUTER_BOUND ( 'NONE', #24434, .T. ) ;
#29049 = CARTESIAN_POINT ( 'NONE',  ( 0.2284923717121198627, -1.304659949875474068, -0.5155029497116575543 ) ) ;
#29050 = DIRECTION ( 'NONE',  ( -7.771561172376107616E-16, 7.170354002788761615E-17, -1.000000000000000000 ) ) ;
#29051 = DIRECTION ( 'NONE',  ( -1.000000000000000000, 0.000000000000000000, 0.000000000000000000 ) ) ;
#29052 = CARTESIAN_POINT ( 'NONE',  ( 0.5187558892663555188, -1.611665626061807854, -0.5500361812898686420 ) ) ;
#29053 = CARTESIAN_POINT ( 'NONE',  ( 0.2279584765017062808, -0.8282534240391157265, 0.6402501348084159716 ) ) ;
#29054 = CARTESIAN_POINT ( 'NONE',  ( -1.627503956099404352E-05, -0.7038055984667742626, -0.1033392639723096362 ) ) ;
#29055 = B_SPLINE_CURVE_WITH_KNOTS ( 'NONE', 3,
 ( #33031, #23794, #26687, #36316 ),
 .UNSPECIFIED., .F., .F.,
 ( 4, 4 ),
 ( 0.003768912384866303020, 0.004058730305933713235 ),
 .UNSPECIFIED. ) ;
#29056 = CIRCLE ( 'NONE', #11320, 0.1946589359789743512 ) ;
#29057 = CARTESIAN_POINT ( 'NONE',  ( -0.02000000000000000042, -2.070343076906777213, -0.2454056712452573896 ) ) ;
#29058 = FACE_OUTER_BOUND ( 'NONE', #19437, .T. ) ;
#29059 = CARTESIAN_POINT ( 'NONE',  ( 0.1362517741244128056, -1.308408735431443093, 0.8505046261270597929 ) ) ;
#29060 = CARTESIAN_POINT ( 'NONE',  ( 0.4898164652207312453, -1.090206986453526872, 0.6335228833721541220 ) ) ;
#29061 = CALENDAR_DATE ( 2026, 13, 10 ) ;
#29062 = CIRCLE ( 'NONE', #5372, 0.1000000000000000056 ) ;
#29063 = AXIS2_PLACEMENT_3D ( 'NONE', #1039, #29384, #23439 ) ;
#29064 = CARTESIAN_POINT ( 'NONE',  ( 0.4559880809074943753, -1.138690969949424314, -0.5155029497116575543 ) ) ;
#29065 = AXIS2_PLACEMENT_3D ( 'NONE', #38089, #3538, #38287 ) ;
#29066 = CARTESIAN_POINT ( 'NONE',  ( -0.08000000000000000167, -1.646519645934556131, -0.1171471737359304072 ) ) ;
#29067 = CARTESIAN_POINT ( 'NONE',  ( -0.04828289906928919656, 0.05688126243839940199, -0.1249999999999999029 ) ) ;
#29068 = EDGE_CURVE ( 'NONE', #13737, #35448, #17319, .T. ) ;
#29069 = EDGE_LOOP ( 'NONE', ( #7113, #516, #32581, #33468, #16903 ) ) ;
#29070 = CARTESIAN_POINT ( 'NONE',  ( -0.09624682736800360683, 0.06028806207340060841, -0.08329560493130658272 ) ) ;
#29071 = DIRECTION ( 'NONE',  ( 0.000000000000000000, -0.9246857012436752177, 0.3807313408632033713 ) ) ;
#29072 = EDGE_CURVE ( 'NONE', #6871, #199, #32393, .T. ) ;
#29073 = CARTESIAN_POINT ( 'NONE',  ( 0.08544226047625283482, -0.8041154030964468014, 0.1055056433848701458 ) ) ;
#29074 = VERTEX_POINT ( 'NONE', #22731 ) ;
#29075 = CARTESIAN_POINT ( 'NONE',  ( 0.4970273525888077026, -1.079783658718535877, 0.3157417262808778213 ) ) ;
#29076 = ADVANCED_FACE ( 'NONE', ( #38539 ), #15121, .T. ) ;
#29077 = CARTESIAN_POINT ( 'NONE',  ( 0.6145270684574122289, -1.293427813764720824, 0.7790094959668801833 ) ) ;
#29079 = ORIENTED_EDGE ( 'NONE', *, *, #32577, .F. ) ;
#29078 = ORIENTED_EDGE ( 'NONE', *, *, #7367, .F. ) ;
#29080 = B_SPLINE_CURVE_WITH_KNOTS ( 'NONE', 3,
 ( #1615, #14533, #36746, #30178, #4650, #20735, #5070, #30380, #11251, #26708 ),
 .UNSPECIFIED., .F., .F.,
 ( 4, 2, 2, 2, 4 ),
 ( 2.347203303329887743E-16, 0.0006195027968147369868, 0.001239005593629237184, 0.001858508390443737489, 0.002478011187258237578 ),
 .UNSPECIFIED. ) ;
#29081 = CARTESIAN_POINT ( 'NONE',  ( 0.01548846960707524721, 0.000000000000000000, 0.000000000000000000 ) ) ;
#29082 = VERTEX_POINT ( 'NONE', #26209 ) ;
#29083 = CARTESIAN_POINT ( 'NONE',  ( 0.3624697024925027655, -1.755837373810828383, -0.4903785605043212148 ) ) ;
#29084 = CARTESIAN_POINT ( 'NONE',  ( 0.6835481475269494789, -1.411548362123641098, 0.6057417262805111502 ) ) ;
#29085 = AXIS2_PLACEMENT_3D ( 'NONE', #37258, #28203, #37449 ) ;
#29086 = CARTESIAN_POINT ( 'NONE',  ( -0.02872242845530520450, 0.5252126300208032061, -0.08844866507292868663 ) ) ;
#29087 = ORIENTED_EDGE ( 'NONE', *, *, #11241, .F. ) ;
#29088 = CARTESIAN_POINT ( 'NONE',  ( 0.008360580759598704517, -0.6769370512592758349, -0.01223308801627121661 ) ) ;
#29089 = CARTESIAN_POINT ( 'NONE',  ( 0.1843596291497116846, -0.8425532430273316997, 0.6072516196132035082 ) ) ;
#29090 = AXIS2_PLACEMENT_3D ( 'NONE', #1410, #8162, #17432 ) ;
#29091 = CARTESIAN_POINT ( 'NONE',  ( 0.0004836969055040355077, -0.4494541051812985799, 0.2297460066914376320 ) ) ;
#29092 = AXIS2_PLACEMENT_3D ( 'NONE', #35887, #37772, #6081 ) ;
#29093 = CARTESIAN_POINT ( 'NONE',  ( 0.1472789844204966947, -0.7831370643385257013, 0.6122178998912563008 ) ) ;
#29094 = EDGE_CURVE ( 'NONE', #8354, #23099, #7765, .T. ) ;
#29096 = CARTESIAN_POINT ( 'NONE',  ( -1.019575837292305609, -0.04310840302198148261, 0.08500000000000004774 ) ) ;
#29095 = CARTESIAN_POINT ( 'NONE',  ( 0.07642826425048794559, -0.9569100421164248305, 0.8158992369460693617 ) ) ;
#29097 = EDGE_CURVE ( 'NONE', #34796, #12108, #33185, .T. ) ;
#29098 = DIRECTION ( 'NONE',  ( -1.000000000000000000, -2.341930812374887555E-31, 1.664003471950578127E-31 ) ) ;
#29099 = ORIENTED_EDGE ( 'NONE', *, *, #10734, .F. ) ;
#29100 = EDGE_CURVE ( 'NONE', #3369, #35103, #8073, .T. ) ;
#29101 = VECTOR ( 'NONE', #21159, 39.37007874015748143 ) ;
#29102 = CARTESIAN_POINT ( 'NONE',  ( 0.6635773287780962759, -1.472843899867129158, -0.6183064675240305119 ) ) ;
#29103 = EDGE_CURVE ( 'NONE', #23460, #4891, #17557, .T. ) ;
#29104 = CARTESIAN_POINT ( 'NONE',  ( 0.1153471661800037629, -0.4465907051537517658, 0.1365881794216603218 ) ) ;
#29105 = DIRECTION ( 'NONE',  ( 0.000000000000000000, 0.000000000000000000, -1.000000000000000000 ) ) ;
#29106 = CIRCLE ( 'NONE', #29750, 0.9087847906030128708 ) ;
#29107 = CARTESIAN_POINT ( 'NONE',  ( -0.02000000000000000042, -1.806850731084499673, -0.8362717670553321270 ) ) ;
#29108 = FACE_OUTER_BOUND ( 'NONE', #33812, .T. ) ;
#29109 = CIRCLE ( 'NONE', #11370, 0.01499999999999995781 ) ;
#29110 = CARTESIAN_POINT ( 'NONE',  ( 0.1943341254738605584, -0.5992045414336306663, 0.2618067726929366734 ) ) ;
#29111 = CARTESIAN_POINT ( 'NONE',  ( -0.01548846960712804005, -0.07651041855114824874, 0.5222379212567086482 ) ) ;
#29112 = CARTESIAN_POINT ( 'NONE',  ( 0.06493940447479917832, -1.341270385318114045, 0.5780714437177661980 ) ) ;
#29113 = AXIS2_PLACEMENT_3D ( 'NONE', #39890, #8209, #26544 ) ;
#29114 = CARTESIAN_POINT ( 'NONE',  ( 4.816453576238493819E-16, 0.2949999999999991518, -0.06434668806854160206 ) ) ;
#29115 = DIRECTION ( 'NONE',  ( 0.000000000000000000, 0.000000000000000000, -1.000000000000000000 ) ) ;
#29116 = VERTEX_POINT ( 'NONE', #39539 ) ;
#29117 = CARTESIAN_POINT ( 'NONE',  ( 0.2101388107736075483, -0.9193160678141170106, 0.6295685468235113769 ) ) ;
#29118 = CARTESIAN_POINT ( 'NONE',  ( 0.02235124290213094667, -0.3550643254722144482, 0.3695962758878555410 ) ) ;
#29119 = CARTESIAN_POINT ( 'NONE',  ( 0.7066109249242027435, -1.499057094600571238, 0.5182417262806440217 ) ) ;
#29120 = CIRCLE ( 'NONE', #10069, 0.01499999999999999424 ) ;
#29121 = CIRCLE ( 'NONE', #18614, 0.08769881541126034463 ) ;
#29122 = ORIENTED_EDGE ( 'NONE', *, *, #37717, .F. ) ;
#29123 = DIRECTION ( 'NONE',  ( -0.4999551463232352333, 0.8660512985181146872, 0.000000000000000000 ) ) ;
#29124 = CARTESIAN_POINT ( 'NONE',  ( 0.09027510456495055347, -0.5695500423695799563, 0.1845836558560018104 ) ) ;
#29125 = EDGE_CURVE ( 'NONE', #18610, #35757, #32969, .T. ) ;
#29126 = CARTESIAN_POINT ( 'NONE',  ( 0.3545348113318227412, -1.718921438480950581, -0.4824991667906958215 ) ) ;
#29127 = CARTESIAN_POINT ( 'NONE',  ( -0.03309058451312555521, -0.08822157290689428000, 0.5132714794726503937 ) ) ;
#29128 = B_SPLINE_CURVE_WITH_KNOTS ( 'NONE', 3,
 ( #20716, #33247, #30162, #1989, #14512, #27078, #39611, #11446, #24013, #28100 ),
 .UNSPECIFIED., .F., .F.,
 ( 4, 2, 2, 2, 4 ),
 ( 0.000000000000000000, 0.0004980634626862015047, 0.0009961269253724030093, 0.001494190388058604622, 0.001992253850744806019 ),
 .UNSPECIFIED. ) ;
#29129 = EDGE_CURVE ( 'NONE', #25252, #31920, #21263, .T. ) ;
#29130 = CARTESIAN_POINT ( 'NONE',  ( 0.1050700346926137646, -0.9324735298191096922, 0.6219226790663787696 ) ) ;
#29131 = ORIENTED_EDGE ( 'NONE', *, *, #23821, .T. ) ;
#29132 = CARTESIAN_POINT ( 'NONE',  ( 0.2059273467974226113, -1.283046334493782359, -0.3194715457588298002 ) ) ;
#29133 = CARTESIAN_POINT ( 'NONE',  ( 0.6620678144876760429, -1.446799780631947252, -0.4151272395384200675 ) ) ;
#29134 = CARTESIAN_POINT ( 'NONE',  ( 0.5959315179729184342, -1.587052097778459236, 0.4182417262808776903 ) ) ;
#29135 = CARTESIAN_POINT ( 'NONE',  ( 0.1856533569311497323, -0.7573055082216308964, 0.1457185332388697685 ) ) ;
#29136 = CARTESIAN_POINT ( 'NONE',  ( 0.4466969641109395095, -1.208888639451673130, 0.6872926701319916898 ) ) ;
#29138 = CARTESIAN_POINT ( 'NONE',  ( 0.3088664963667265839, -1.757905065063136263, 0.5295467280985149960 ) ) ;
#29137 = CARTESIAN_POINT ( 'NONE',  ( -2.070754768975505034, -0.09959325338431362917, 0.1178658435936983939 ) ) ;
#29139 = CARTESIAN_POINT ( 'NONE',  ( 0.5849095050029387011, -1.491341823319836335, -0.5960747874205124530 ) ) ;
#29140 = EDGE_LOOP ( 'NONE', ( #12034, #33748, #8742, #37016, #23291 ) ) ;
#29141 = COORDINATED_UNIVERSAL_TIME_OFFSET ( 0, 0, .AHEAD. ) ;
#29142 = LINE ( 'NONE', #1006, #34897 ) ;
#29143 = ORIENTED_EDGE ( 'NONE', *, *, #28134, .T. ) ;
#29144 = CARTESIAN_POINT ( 'NONE',  ( 0.3372045214619368569, -1.404289603606768022, 0.8754725392422132435 ) ) ;
#29146 = CARTESIAN_POINT ( 'NONE',  ( 0.1978587402095110526, -0.5849795632144990654, 0.3178455878192493200 ) ) ;
#29145 = CARTESIAN_POINT ( 'NONE',  ( 0.08513964112126702621, -0.8107931711784008844, 0.1400984422957800846 ) ) ;
#29147 = DIRECTION ( 'NONE',  ( 0.000000000000000000, 0.000000000000000000, 1.000000000000000000 ) ) ;
#29148 = ORIENTED_EDGE ( 'NONE', *, *, #18835, .F. ) ;
#29149 = AXIS2_PLACEMENT_3D ( 'NONE', #20009, #25994, #1115 ) ;
#29150 = VERTEX_POINT ( 'NONE', #4773 ) ;
#29151 = ADVANCED_FACE ( 'NONE', ( #1928 ), #17347, .F. ) ;
#29152 = CARTESIAN_POINT ( 'NONE',  ( 0.06936654275873489761, -1.327133429011184917, 0.5458395137742713121 ) ) ;
#29153 = CARTESIAN_POINT ( 'NONE',  ( 0.1194264420602569737, -0.5625551924984868446, 0.2197023614733592256 ) ) ;
#29154 = ORIENTED_EDGE ( 'NONE', *, *, #29817, .T. ) ;
#29155 = CARTESIAN_POINT ( 'NONE',  ( 0.1874546992375723808, -0.6895993665818519469, 0.05733668763868348534 ) ) ;
#29156 = DIRECTION ( 'NONE',  ( 1.000000000000000000, 0.000000000000000000, 0.000000000000000000 ) ) ;
#29157 = VECTOR ( 'NONE', #32006, 39.37007874015748143 ) ;
#29158 = AXIS2_PLACEMENT_3D ( 'NONE', #9239, #21814, #11733 ) ;
#29159 = CARTESIAN_POINT ( 'NONE',  ( 0.1859644761936219692, -0.7910310107535581947, 0.1899855147966034163 ) ) ;
#29160 = CARTESIAN_POINT ( 'NONE',  ( 0.4062230848227149638, -1.145582794160931117, 0.4248905050063955802 ) ) ;
#29161 = FACE_OUTER_BOUND ( 'NONE', #10116, .T. ) ;
#29162 = CARTESIAN_POINT ( 'NONE',  ( 0.08630618708051779331, -0.7262393365227618469, 0.1454069901622962735 ) ) ;
#29163 = TOROIDAL_SURFACE ( 'NONE', #10137, 0.1333070866141734256, 0.02999999999999999889 ) ;
#29164 = B_SPLINE_CURVE_WITH_KNOTS ( 'NONE', 3,
 ( #35170, #13564, #19932, #25926, #34747, #19132, #38449, #10464, #12962, #31670 ),
 .UNSPECIFIED., .F., .F.,
 ( 4, 2, 2, 2, 4 ),
 ( 0.001190081892692469809, 0.001790126153740256160, 0.002390170414788042510, 0.002990214675835828860, 0.003590258936883615210 ),
 .UNSPECIFIED. ) ;
#29165 = CARTESIAN_POINT ( 'NONE',  ( 0.7032651991748780640, -1.440401145529036642, 0.7869155231269625572 ) ) ;
#29166 = CARTESIAN_POINT ( 'NONE',  ( 0.3880702231493639021, -1.818540937610624519, -0.4825054957597859628 ) ) ;
#29167 = CIRCLE ( 'NONE', #6801, 0.1000000000000000194 ) ;
#29168 = DIRECTION ( 'NONE',  ( 0.000000000000000000, 0.8063205929144885431, -0.5914787413272156735 ) ) ;
#29169 = CARTESIAN_POINT ( 'NONE',  ( 0.07779920321647403048, -1.322114474344633583, 0.5682417262808776570 ) ) ;
#29170 = PERSON_AND_ORGANIZATION_ROLE ( 'design_owner' ) ;
#29171 = CARTESIAN_POINT ( 'NONE',  ( 0.6430854927599457538, -1.494222493094318427, -0.6187715783251990231 ) ) ;
#29172 = CARTESIAN_POINT ( 'NONE',  ( 0.04762035657658417187, 0.2475516194925301006, 0.4138014489398430529 ) ) ;
#29173 = CARTESIAN_POINT ( 'NONE',  ( -0.1167294260180564980, -0.5331983351047929753, 0.3082670712249074296 ) ) ;
#29174 = CARTESIAN_POINT ( 'NONE',  ( 0.6960334162051958762, -1.427192076786115926, 0.4182417262808776348 ) ) ;
#29175 = CYLINDRICAL_SURFACE ( 'NONE', #37669, 0.1000000000000000194 ) ;
#29176 = CARTESIAN_POINT ( 'NONE',  ( 0.2493678129588278725, -1.619726033520551667, 0.7664167198318853069 ) ) ;
#29177 = CARTESIAN_POINT ( 'NONE',  ( -0.0004140221094746326480, -0.9366944287225720256, 0.1292664348825115495 ) ) ;
#29178 = CIRCLE ( 'NONE', #21971, 0.01499999999999996128 ) ;
#29179 = DIRECTION ( 'NONE',  ( 0.000000000000000000, 0.000000000000000000, -1.000000000000000000 ) ) ;
#29180 = EDGE_CURVE ( 'NONE', #19277, #26731, #31756, .T. ) ;
#29181 = CYLINDRICAL_SURFACE ( 'NONE', #36372, 0.4488493849861018847 ) ;
#29182 = CARTESIAN_POINT ( 'NONE',  ( 0.3584893225414327311, -1.160935888217208944, 0.4273648005544712358 ) ) ;
#29183 = VERTEX_POINT ( 'NONE', #38943 ) ;
#29184 = AXIS2_PLACEMENT_3D ( 'NONE', #35704, #20089, #23992 ) ;
#29185 = ORIENTED_EDGE ( 'NONE', *, *, #29072, .T. ) ;
#29186 = TOROIDAL_SURFACE ( 'NONE', #4881, 0.08830708661417342731, 0.01499999999999999944 ) ;
#29187 = CARTESIAN_POINT ( 'NONE',  ( 0.04293701532779508473, -0.3457382709204475102, -0.3536859687696385368 ) ) ;
#29188 = ORIENTED_EDGE ( 'NONE', *, *, #36575, .F. ) ;
#29189 = AXIS2_PLACEMENT_3D ( 'NONE', #8658, #24318, #15053 ) ;
#29190 = DIRECTION ( 'NONE',  ( 1.000000000000000000, 7.012307549337720382E-13, 2.434866152052798842E-12 ) ) ;
#29191 = DIRECTION ( 'NONE',  ( -1.000000000000000000, -7.857794173099924470E-32, -8.628166150854818811E-32 ) ) ;
#29192 = CARTESIAN_POINT ( 'NONE',  ( 0.5056812288904104502, -1.307114837766834903, 0.7688671359748000533 ) ) ;
#29194 = ORIENTED_EDGE ( 'NONE', *, *, #29100, .T. ) ;
#29193 = CARTESIAN_POINT ( 'NONE',  ( -0.1073276781670975538, -0.4890918960634569879, 0.09878957693462719902 ) ) ;
#29195 = CARTESIAN_POINT ( 'NONE',  ( 0.5342447626335863342, -1.156090923338821463, 0.6541422520001994867 ) ) ;
#29196 = CIRCLE ( 'NONE', #26599, 0.009999999999999991535 ) ;
#29197 = DIRECTION ( 'NONE',  ( 0.8660512985181133550, 0.4999551463232373982, 0.000000000000000000 ) ) ;
#29198 = ORIENTED_EDGE ( 'NONE', *, *, #18726, .F. ) ;
#29199 = CARTESIAN_POINT ( 'NONE',  ( 0.5776223404472408118, -1.608891578473971462, 0.4473154535768434914 ) ) ;
#29200 = ORIENTED_EDGE ( 'NONE', *, *, #17128, .T. ) ;
#29201 = AXIS2_PLACEMENT_3D ( 'NONE', #34528, #18911, #3255 ) ;
#29202 = CARTESIAN_POINT ( 'NONE',  ( 0.2958245360769962695, -1.526781842427403779, 0.8634596908947912430 ) ) ;
#29204 = CARTESIAN_POINT ( 'NONE',  ( 0.1126380441730984588, -0.7649468025915582281, -0.08306241175244397090 ) ) ;
#29203 = CARTESIAN_POINT ( 'NONE',  ( 0.5453720701673475668, -1.664424278530242329, -0.4777853237623809202 ) ) ;
#29205 = CARTESIAN_POINT ( 'NONE',  ( -2.112273405726188513E-14, -2.183180860297921466, -0.7437760292030870524 ) ) ;
#29206 = CARTESIAN_POINT ( 'NONE',  ( 0.04890254750393845107, -1.632792488206058712, -0.3425393862321154392 ) ) ;
#29207 = ORIENTED_EDGE ( 'NONE', *, *, #25749, .T. ) ;
#29208 = CARTESIAN_POINT ( 'NONE',  ( 0.5446892099791311725, -1.168309311726712929, 0.5668322337678470824 ) ) ;
#29209 = CARTESIAN_POINT ( 'NONE',  ( 0.1862143093560918450, -0.9153542374866598941, 0.1449575636331434381 ) ) ;
#29210 = CARTESIAN_POINT ( 'NONE',  ( -0.03868264068766699704, 0.03360988006412133494, -0.4753775160315154569 ) ) ;
#29211 = CARTESIAN_POINT ( 'NONE',  ( 0.5846648009247458200, -1.436025231029266491, 0.7313505297771951685 ) ) ;
#29212 = CARTESIAN_POINT ( 'NONE',  ( 0.1431253995614544250, -0.8748228831234901026, 0.5195852956218338647 ) ) ;
#29213 = LINE ( 'NONE', #16459, #3418 ) ;
#29214 = AXIS2_PLACEMENT_3D ( 'NONE', #4574, #14265, #39546 ) ;
#29215 = EDGE_CURVE ( 'NONE', #33041, #25042, #33785, .T. ) ;
#29216 = CARTESIAN_POINT ( 'NONE',  ( -0.2300000000000005651, 0.5182417262804733804, 0.08500000000000004774 ) ) ;
#29217 = CIRCLE ( 'NONE', #37757, 0.08830708661417320526 ) ;
#29218 = B_SPLINE_CURVE_WITH_KNOTS ( 'NONE', 3,
 ( #21539, #23471, #12058, #2401, #17061, #27689, #2591, #18016, #5672, #32883 ),
 .UNSPECIFIED., .F., .F.,
 ( 4, 2, 2, 2, 4 ),
 ( 0.000000000000000000, 0.0007428348738404900358, 0.001485669747680980072, 0.002228504621521470216, 0.002971339495361960143 ),
 .UNSPECIFIED. ) ;
#29219 = AXIS2_PLACEMENT_3D ( 'NONE', #26943, #23872, #30217 ) ;
#29220 = CARTESIAN_POINT ( 'NONE',  ( -0.1688425317846173890, 0.4915896084592923376, 0.3245441658521664996 ) ) ;
#29221 = CARTESIAN_POINT ( 'NONE',  ( 0.6580168967375891187, -1.537959750076741905, 0.4238314998512365261 ) ) ;
#29222 = CARTESIAN_POINT ( 'NONE',  ( 0.5959315179729184342, -1.587052097778459236, 0.4182417262808776903 ) ) ;
#29223 = CARTESIAN_POINT ( 'NONE',  ( 0.3223881462519361807, -1.760756727098002905, 0.4929000792678752130 ) ) ;
#29224 = CALENDAR_DATE ( 2026, 13, 10 ) ;
#29225 = APPROVAL_PERSON_ORGANIZATION ( #34934, #8649, #5924 ) ;
#29226 = CARTESIAN_POINT ( 'NONE',  ( 0.04157078424165575742, -0.2900150886686562179, 0.3701869471361556307 ) ) ;
#29227 = DIRECTION ( 'NONE',  ( 0.8660512985181132439, 0.4999551463232376758, -6.610988856618925964E-16 ) ) ;
#29228 = AXIS2_PLACEMENT_3D ( 'NONE', #37545, #2804, #37353 ) ;
#29229 = CARTESIAN_POINT ( 'NONE',  ( 0.1947176629093842759, -1.666009496152422331, -0.6564531187584504712 ) ) ;
#29230 = EDGE_LOOP ( 'NONE', ( #16648, #39758, #5512, #11440 ) ) ;
#29231 = CARTESIAN_POINT ( 'NONE',  ( 0.4542745521636228356, -1.690364615762230072, 0.4457110224561552925 ) ) ;
#29232 = CARTESIAN_POINT ( 'NONE',  ( -0.02953079040095693900, -0.2329676531120430660, 0.4763574306556350169 ) ) ;
#29233 = CARTESIAN_POINT ( 'NONE',  ( 0.01548846960707524721, 0.000000000000000000, 0.000000000000000000 ) ) ;
#29234 = DIRECTION ( 'NONE',  ( 1.000000000000000000, 1.445897915516965072E-15, -8.881784197001242463E-16 ) ) ;
#29235 = DIRECTION ( 'NONE',  ( 0.000000000000000000, 0.000000000000000000, 1.000000000000000000 ) ) ;
#29236 = VERTEX_POINT ( 'NONE', #13642 ) ;
#29237 = CARTESIAN_POINT ( 'NONE',  ( 0.2656489473450271976, -1.672876873347360460, 0.5357873754474390404 ) ) ;
#29238 = VECTOR ( 'NONE', #5337, 39.37007874015748854 ) ;
#29239 = CARTESIAN_POINT ( 'NONE',  ( 0.4665068745543000661, -1.281967417980122592, 0.8176874307884230975 ) ) ;
#29241 = ORIENTED_EDGE ( 'NONE', *, *, #19196, .T. ) ;
#29240 = CARTESIAN_POINT ( 'NONE',  ( 0.5454073695792218679, -1.172337910823015861, 0.5979107612308603992 ) ) ;
#29242 = AXIS2_PLACEMENT_3D ( 'NONE', #25165, #15695, #6832 ) ;
#29243 = B_SPLINE_CURVE_WITH_KNOTS ( 'NONE', 3,
 ( #2595, #36548, #2200, #24411 ),
 .UNSPECIFIED., .F., .F.,
 ( 4, 4 ),
 ( 0.000000000000000000, 0.001825717054875163796 ),
 .UNSPECIFIED. ) ;
#29245 = VERTEX_POINT ( 'NONE', #35866 ) ;
#29244 = ORIENTED_EDGE ( 'NONE', *, *, #27646, .F. ) ;
#29246 = CARTESIAN_POINT ( 'NONE',  ( 0.5981247542016078222, -1.393184347378918719, 0.8655563894600949437 ) ) ;
#29247 = AXIS2_PLACEMENT_3D ( 'NONE', #31963, #38728, #9945 ) ;
#29248 = ORIENTED_EDGE ( 'NONE', *, *, #7728, .T. ) ;
#29249 = CARTESIAN_POINT ( 'NONE',  ( -0.01381286397089885078, -0.5423028182772705597, 0.2346020896048880977 ) ) ;
#29250 = APPROVAL_PERSON_ORGANIZATION ( #11358, #7104, #32558 ) ;
#29251 = FACE_OUTER_BOUND ( 'NONE', #37783, .T. ) ;
#29252 = APPROVAL_DATE_TIME ( #29860, #37929 ) ;
#29253 = CARTESIAN_POINT ( 'NONE',  ( 0.5264113014007612001, -1.640729993778266893, -0.5166151207188711680 ) ) ;
#29254 = ORIENTED_EDGE ( 'NONE', *, *, #14263, .T. ) ;
#29255 = CARTESIAN_POINT ( 'NONE',  ( 0.1053302763654986457, -0.8311093529158266602, 0.3669983993270940492 ) ) ;
#29256 = APPLICATION_CONTEXT ( 'configuration controlled 3d designs of mechanical parts and assemblies' ) ;
#29257 = AXIS2_PLACEMENT_3D ( 'NONE', #5736, #9036, #34120 ) ;
#29258 = CARTESIAN_POINT ( 'NONE',  ( 0.1989976604547370465, -2.047409678865564686, -0.7132172901365274598 ) ) ;
#29259 = CARTESIAN_POINT ( 'NONE',  ( 0.5403123773656385298, -1.518157346897373472, 0.6083719484155812873 ) ) ;
#29260 = ORIENTED_EDGE ( 'NONE', *, *, #19478, .F. ) ;
#29261 = FACE_OUTER_BOUND ( 'NONE', #37701, .T. ) ;
#29262 = DIRECTION ( 'NONE',  ( 0.4999551463232373427, -0.8660512985181134660, 0.000000000000000000 ) ) ;
#29263 = CARTESIAN_POINT ( 'NONE',  ( 0.7154111682914670034, -1.479334727086170531, 0.5070875326645477577 ) ) ;
#29264 = B_SPLINE_CURVE_WITH_KNOTS ( 'NONE', 3,
 ( #32501, #39287, #38676, #7391, #35999, #17278, #19756, #10494 ),
 .UNSPECIFIED., .F., .F.,
 ( 4, 2, 2, 4 ),
 ( 0.000000000000000000, 0.0002979885802634735085, 0.0005959771605269470170, 0.001191954321053893167 ),
 .UNSPECIFIED. ) ;
#29265 = DIRECTION ( 'NONE',  ( 0.9998941247116546194, -0.01455087607601020412, 0.0001066420868422379633 ) ) ;
#29266 = CARTESIAN_POINT ( 'NONE',  ( 0.05999999999999990757, -9.785038312124664947E-34, 0.5614999999999926716 ) ) ;
#29267 = FACE_OUTER_BOUND ( 'NONE', #5509, .T. ) ;
#29268 = EDGE_CURVE ( 'NONE', #25716, #8811, #13669, .T. ) ;
#29269 = CARTESIAN_POINT ( 'NONE',  ( -0.08000000000000000167, -2.070343076906777213, -0.2454056712452573896 ) ) ;
#29270 = CARTESIAN_POINT ( 'NONE',  ( 0.6077303093371694276, -1.473904537801408399, 0.6398553165839666601 ) ) ;
#29271 = CARTESIAN_POINT ( 'NONE',  ( 0.01162314945304296701, -0.7953763623839829044, -0.08968356552621570277 ) ) ;
#29272 = CARTESIAN_POINT ( 'NONE',  ( 0.1335939600180593712, -0.7447735389487355473, 0.5690569422650127995 ) ) ;
#29273 = B_SPLINE_CURVE_WITH_KNOTS ( 'NONE', 3,
 ( #31072, #2492, #27582, #39713, #2685, #8853, #15443, #37435, #15227, #11741 ),
 .UNSPECIFIED., .F., .F.,
 ( 4, 2, 2, 2, 4 ),
 ( 0.002284120846990289264, 0.002652607256290875643, 0.003021093665591462023, 0.003389580074892048402, 0.003758066484192634782 ),
 .UNSPECIFIED. ) ;
#29274 =( NAMED_UNIT ( * ) PLANE_ANGLE_UNIT ( ) SI_UNIT ( $, .RADIAN. ) );
#29275 = VECTOR ( 'NONE', #6780, 39.37007874015747433 ) ;
#29276 = EDGE_CURVE ( 'NONE', #13608, #15882, #24702, .T. ) ;
#29277 = CARTESIAN_POINT ( 'NONE',  ( 0.4089992519647981384, -1.131314579718122992, 0.3157417262808777658 ) ) ;
#29278 = CIRCLE ( 'NONE', #34526, 0.1000000000000000194 ) ;
#29279 = CARTESIAN_POINT ( 'NONE',  ( 0.03159140494779963393, -0.4819881711443563810, -0.09921162977303815689 ) ) ;
#29280 = ADVANCED_FACE ( 'NONE', ( #31668 ), #15431, .T. ) ;
#29281 = CARTESIAN_POINT ( 'NONE',  ( -0.002783323111321702164, -0.8122190247268278318, 0.2436509486217987297 ) ) ;
#29282 = CARTESIAN_POINT ( 'NONE',  ( 0.3243638931714790674, -0.9652511992726795498, 0.5977393664509621507 ) ) ;
#29283 = APPROVAL_STATUS ( 'not_yet_approved' ) ;
#29284 = SECURITY_CLASSIFICATION ( '', '', #16388 ) ;
#29285 = CARTESIAN_POINT ( 'NONE',  ( 0.3817504269947758488, -1.726033828776070367, 0.4251703030630866742 ) ) ;
#29286 = CIRCLE ( 'NONE', #29257, 0.1600000000000016409 ) ;
#29287 = FACE_OUTER_BOUND ( 'NONE', #35445, .T. ) ;
#29288 = EDGE_CURVE ( 'NONE', #37556, #6802, #4806, .T. ) ;
#29289 = VERTEX_POINT ( 'NONE', #34136 ) ;
#29290 = CARTESIAN_POINT ( 'NONE',  ( 0.3666666666666451024, -1.962130349776132210, -0.6793646662227855737 ) ) ;
#29291 = APPLIED_PERSON_AND_ORGANIZATION_ASSIGNMENT ( #11807, #30738, ( #27234 ) ) ;
#29292 = CARTESIAN_POINT ( 'NONE',  ( 0.002326877264082053299, -0.5233753183007167076, 0.1831555727087032792 ) ) ;
#29293 = CARTESIAN_POINT ( 'NONE',  ( 0.1840595033465176056, -0.8547675690073376353, 0.1457166466292989515 ) ) ;
#29294 = EDGE_LOOP ( 'NONE', ( #12864, #4442, #23141 ) ) ;
#29295 = DIRECTION ( 'NONE',  ( 0.000000000000000000, 0.000000000000000000, 1.000000000000000000 ) ) ;
#29296 = CARTESIAN_POINT ( 'NONE',  ( 0.6622529324379804461, -1.370658042826599310, 0.7087354899337895420 ) ) ;
#29298 = EDGE_LOOP ( 'NONE', ( #24945, #33416, #11700, #37365 ) ) ;
#29297 = ORIENTED_EDGE ( 'NONE', *, *, #20595, .F. ) ;
#29299 = DIRECTION ( 'NONE',  ( -1.000000000000000000, 0.000000000000000000, -7.886895865933756492E-16 ) ) ;
#29300 = ORIENTED_EDGE ( 'NONE', *, *, #25513, .T. ) ;
#29301 = FACE_OUTER_BOUND ( 'NONE', #16048, .T. ) ;
#29302 = CARTESIAN_POINT ( 'NONE',  ( 0.6059691746655119227, -1.480133143157562170, 0.5526975506195443977 ) ) ;
#29303 = CIRCLE ( 'NONE', #22103, 0.6143128707267527799 ) ;
#29304 = CARTESIAN_POINT ( 'NONE',  ( -0.03170752374382806299, 0.4816921673044415875, -0.09938322573837012064 ) ) ;
#29305 = ORIENTED_EDGE ( 'NONE', *, *, #5635, .F. ) ;
#29306 = CARTESIAN_POINT ( 'NONE',  ( 0.5118594077320766100, -1.202344868804445133, 1.007689851825548599 ) ) ;
#29307 = AXIS2_PLACEMENT_3D ( 'NONE', #15513, #17767, #36504 ) ;
#29308 = CARTESIAN_POINT ( 'NONE',  ( 0.09436846326521548811, -0.6977451578140484445, 0.2870226784748305393 ) ) ;
#29309 = CARTESIAN_POINT ( 'NONE',  ( 0.001484853620285140697, -0.4699967301967150068, 0.2916140860605750951 ) ) ;
#29310 = CARTESIAN_POINT ( 'NONE',  ( 0.4566189328666658831, -1.463090425276903250, 0.7988651862389967162 ) ) ;
#29312 = FACE_OUTER_BOUND ( 'NONE', #38203, .T. ) ;
#29311 = CARTESIAN_POINT ( 'NONE',  ( 0.1136081630506033391, -0.6096919713534713070, -0.08294989974448961634 ) ) ;
#29313 = CARTESIAN_POINT ( 'NONE',  ( 0.3801146823547868481, -1.145807599758760897, 0.5916166056748334290 ) ) ;
#29314 = LOCAL_TIME ( 0, 53, 7.000000000000000000, #33194 ) ;
#29315 = ORIENTED_EDGE ( 'NONE', *, *, #33368, .T. ) ;
#29316 = ORIENTED_EDGE ( 'NONE', *, *, #19356, .F. ) ;
#29317 = CARTESIAN_POINT ( 'NONE',  ( 0.3218915951663034458, -1.643224469256787446, 0.5371356550339121405 ) ) ;
#29318 = CARTESIAN_POINT ( 'NONE',  ( 0.1271493835291065966, -0.5197209161013818246, 0.3904091046342937910 ) ) ;
#29319 = AXIS2_PLACEMENT_3D ( 'NONE', #10442, #25684, #19316 ) ;
#29320 = CARTESIAN_POINT ( 'NONE',  ( -0.04762200653274661216, 0.2475542241873639471, -0.4137947767340805494 ) ) ;
#29321 = EDGE_CURVE ( 'NONE', #5083, #37512, #37219, .T. ) ;
#29322 =( BOUNDED_SURFACE ( )  B_SPLINE_SURFACE ( 3, 2, ( 
 ( #29104, #37536, #22155 ),
 ( #12451, #19044, #6672 ),
 ( #31791, #575, #25433 ),
 ( #13070, #25622, #38155 ),
 ( #22547, #28497, #35077 ),
 ( #6880, #18852, #19458 ),
 ( #35284, #38353, #31993 ),
 ( #31395, #15739, #28288 ),
 ( #10191, #28897, #759 ),
 ( #25834, #12875, #7079 ),
 ( #31576, #25003, #12649 ),
 ( #9578, #3395, #15951 ),
 ( #7269, #26431, #35684 ),
 ( #29711, #32990, #36275 ),
 ( #20457, #33208, #10579 ),
 ( #23153, #1556, #38968 ),
 ( #26045, #4588, #23370 ),
 ( #7484, #29510, #35468 ),
 ( #17372, #5013, #39184 ),
 ( #20064, #22951, #32788 ),
 ( #10797, #8097, #17160 ),
 ( #1770, #10387, #20674 ),
 ( #14076, #17580, #966 ),
 ( #29318, #20266, #36084 ),
 ( #7700, #35892, #11193 ),
 ( #39373, #19847, #14281 ),
 ( #26653, #11010, #32379 ),
 ( #26231, #1349, #38752 ),
 ( #4797, #13476, #23566 ),
 ( #7886, #29928, #26846 ),
 ( #4206, #32595, #13857 ),
 ( #4408, #38564, #23756 ),
 ( #13665, #16967, #16770 ),
 ( #1165, #34206, #30122 ),
 ( #14894, #6017, #23968 ),
 ( #2745, #2144, #30922 ),
 ( #24569, #20881, #24173 ),
 ( #21068, #36497, #33403 ),
 ( #21277, #27849, #5210 ),
 ( #5620, #1953, #24357 ),
 ( #18176, #2352, #39781 ),
 ( #24774, #14468, #15294 ),
 ( #27452, #39977, #8311 ),
 ( #33814, #8701, #12214 ),
 ( #30729, #2550, #17764 ),
 ( #30316, #14682, #40389 ),
 ( #36890, #39564, #37099 ),
 ( #15087, #9110, #11612 ),
 ( #18374, #8914, #27251 ),
 ( #5404, #21492, #36697 ),
 ( #5815, #27035, #11396 ),
 ( #37297, #21676, #34011 ),
 ( #8504, #33595, #17967 ),
 ( #11798, #12004, #30528 ),
 ( #27643, #40173, #3554 ),
 ( #19195, #34416, #37917 ),
 ( #22493, #318, #6232 ),
 ( #9727, #22296, #3340 ),
 ( #34811, #40585, #9924 ),
 ( #6616, #9310, #28061 ),
 ( #15900, #15508, #25783 ),
 ( #13027, #3766, #25383 ),
 ( #28856, #12823, #16319 ),
 ( #19412, #35018, #31735 ),
 ( #3153, #24959, #22709 ),
 ( #34624, #10135, #2956 ),
 ( #16123, #25575, #12604 ),
 ( #12407, #15693, #6830 ),
 ( #28661, #37489, #37703 ),
 ( #530, #38105, #28445 ),
 ( #31946, #21889, #715 ),
 ( #18800, #31351, #35240 ),
 ( #28243, #38303, #108 ),
 ( #13216, #18582, #31140 ),
 ( #6425, #25164, #9526 ),
 ( #22104, #18993, #31526 ),
 ( #32332, #13815, #11145 ),
 ( #20217, #32542, #23704 ),
 ( #17115, #20410, #19795 ),
 ( #26189, #1507, #38519 ) ),
 .UNSPECIFIED., .F., .F., .T. ) 
 B_SPLINE_SURFACE_WITH_KNOTS ( ( 4, 2, 2, 2, 2, 2, 2, 2, 2, 2, 2, 2, 2, 2, 2, 2, 2, 2, 2, 2, 2, 2, 2, 2, 2, 2, 2, 2, 2, 2, 2, 2, 2, 2, 2, 2, 2, 2, 2, 4 ),
 ( 3, 3 ),
 ( 0.006927710299821351891, 0.007080480144256291047, 0.007156865066473760625, 0.007175961297028127586, 0.007195057527582495414, 0.007233249988691230203, 0.007538789677561109383, 0.008149869055300866874, 0.009372027810780381857, 0.009983107188520138481, 0.01059418656625989684, 0.01181634532173941182, 0.01426066283269844179, 0.01548282158817795677, 0.01670498034365747175, 0.01914929785461650172, 0.02037145661009601844, 0.02159361536557553168, 0.02403793287653456165, 0.02526009163201407837, 0.02648225038749359161, 0.02892656789845262158, 0.03137088540941165155, 0.03381520292037068498, 0.03625952043132971148, 0.03748167918680922472, 0.03870383794228873797, 0.03992599669776825122, 0.04114815545324777141, 0.04175923483098753497, 0.04237031420872729159, 0.04298139358646704822, 0.04359247296420680484, 0.04481463171968631809, 0.04542571109742607471, 0.04573125078629595303, 0.04580763570851342781, 0.04584582816962216173, 0.04588402063073089565, 0.04603679047516583134 ),
 ( 0.000000000000000000, 1.000000000000000000 ),
 .UNSPECIFIED. ) 
 GEOMETRIC_REPRESENTATION_ITEM ( )  RATIONAL_B_SPLINE_SURFACE ( (
 ( 1.000000000000000000, 0.7702110884164732330, 1.000000000000000000),
 ( 1.000000000000000000, 0.7702110884164732330, 1.000000000000000000),
 ( 1.000000000000000000, 0.7702110884164714566, 1.000000000000000000),
 ( 1.000000000000000000, 0.7702110884164714566, 1.000000000000000000),
 ( 1.000000000000000000, 0.7702110884164720117, 1.000000000000000000),
 ( 1.000000000000000000, 0.7702110884164720117, 1.000000000000000000),
 ( 1.000000000000000000, 0.7702110011759223385, 1.000000000000000000),
 ( 1.000000000000000000, 0.7702104367782812711, 1.000000000000000000),
 ( 1.000000000000000000, 0.7702099955263094211, 1.000000000000000000),
 ( 1.000000000000000000, 0.7702082218146070192, 1.000000000000000000),
 ( 1.000000000000000000, 0.7702064393915036833, 1.000000000000000000),
 ( 1.000000000000000000, 0.7701856336384715895, 1.000000000000000000),
 ( 1.000000000000000000, 0.7701341339086081872, 1.000000000000000000),
 ( 1.000000000000000000, 0.7699716772124094444, 1.000000000000000000),
 ( 1.000000000000000000, 0.7698275467342896583, 1.000000000000000000),
 ( 1.000000000000000000, 0.7695145108938888923, 1.000000000000000000),
 ( 1.000000000000000000, 0.7694543563866118596, 1.000000000000000000),
 ( 1.000000000000000000, 0.7690885663133745220, 1.000000000000000000),
 ( 1.000000000000000000, 0.7689098704262390394, 1.000000000000000000),
 ( 1.000000000000000000, 0.7684714123184787082, 1.000000000000000000),
 ( 1.000000000000000000, 0.7682081441206239925, 1.000000000000000000),
 ( 1.000000000000000000, 0.7673848213495205739, 1.000000000000000000),
 ( 1.000000000000000000, 0.7667110773309444571, 1.000000000000000000),
 ( 1.000000000000000000, 0.7644349880097887073, 1.000000000000000000),
 ( 1.000000000000000000, 0.7629103163539596721, 1.000000000000000000),
 ( 1.000000000000000000, 0.7602566924737247378, 1.000000000000000000),
 ( 1.000000000000000000, 0.7593162002605474692, 1.000000000000000000),
 ( 1.000000000000000000, 0.7573931270347130651, 1.000000000000000000),
 ( 1.000000000000000000, 0.7564157440002493571, 1.000000000000000000),
 ( 1.000000000000000000, 0.7534999497245773448, 1.000000000000000000),
 ( 1.000000000000000000, 0.7515885138869485838, 1.000000000000000000),
 ( 1.000000000000000000, 0.7495871733758280309, 1.000000000000000000),
 ( 1.000000000000000000, 0.7490774071070243068, 1.000000000000000000),
 ( 1.000000000000000000, 0.7486382088202092611, 1.000000000000000000),
 ( 1.000000000000000000, 0.7486976975356955943, 1.000000000000000000),
 ( 1.000000000000000000, 0.7501897554486547381, 1.000000000000000000),
 ( 1.000000000000000000, 0.7529466885742388538, 1.000000000000000000),
 ( 1.000000000000000000, 0.7614317847769825898, 1.000000000000000000),
 ( 1.000000000000000000, 0.7649793793770901518, 1.000000000000000000),
 ( 1.000000000000000000, 0.7733644470982655728, 1.000000000000000000),
 ( 1.000000000000000000, 0.7782111082216958131, 1.000000000000000000),
 ( 1.000000000000000000, 0.7935801609140271662, 1.000000000000000000),
 ( 1.000000000000000000, 0.8047319212507089148, 1.000000000000000000),
 ( 1.000000000000000000, 0.8229932177232615054, 1.000000000000000000),
 ( 1.000000000000000000, 0.8301201759576161132, 1.000000000000000000),
 ( 1.000000000000000000, 0.8391316605326407663, 1.000000000000000000),
 ( 1.000000000000000000, 0.8411418536465049556, 1.000000000000000000),
 ( 1.000000000000000000, 0.8403510782710301719, 1.000000000000000000),
 ( 1.000000000000000000, 0.8376700127300911181, 1.000000000000000000),
 ( 1.000000000000000000, 0.8302417975051545884, 1.000000000000000000),
 ( 1.000000000000000000, 0.8271837635025202085, 1.000000000000000000),
 ( 1.000000000000000000, 0.8196313788825587698, 1.000000000000000000),
 ( 1.000000000000000000, 0.8151231434854736557, 1.000000000000000000),
 ( 1.000000000000000000, 0.8044346982436086924, 1.000000000000000000),
 ( 1.000000000000000000, 0.7981958681030024705, 1.000000000000000000),
 ( 1.000000000000000000, 0.7834537592509257520, 1.000000000000000000),
 ( 1.000000000000000000, 0.7750610009823194479, 1.000000000000000000),
 ( 1.000000000000000000, 0.7615137475724482741, 1.000000000000000000),
 ( 1.000000000000000000, 0.7568191938289150489, 1.000000000000000000),
 ( 1.000000000000000000, 0.7477386341990411855, 1.000000000000000000),
 ( 1.000000000000000000, 0.7433521509119807025, 1.000000000000000000),
 ( 1.000000000000000000, 0.7352470023408808064, 1.000000000000000000),
 ( 1.000000000000000000, 0.7315263130049088902, 1.000000000000000000),
 ( 1.000000000000000000, 0.7249624713081709304, 1.000000000000000000),
 ( 1.000000000000000000, 0.7221161546641846618, 1.000000000000000000),
 ( 1.000000000000000000, 0.7150846530265827505, 1.000000000000000000),
 ( 1.000000000000000000, 0.7122753070958832700, 1.000000000000000000),
 ( 1.000000000000000000, 0.7098586832190030282, 1.000000000000000000),
 ( 1.000000000000000000, 0.7093529624755150476, 1.000000000000000000),
 ( 1.000000000000000000, 0.7089420370521081205, 1.000000000000000000),
 ( 1.000000000000000000, 0.7088634414763608227, 1.000000000000000000),
 ( 1.000000000000000000, 0.7088270497185857888, 1.000000000000000000),
 ( 1.000000000000000000, 0.7088245591381706623, 1.000000000000000000),
 ( 1.000000000000000000, 0.7088184571567831549, 1.000000000000000000),
 ( 1.000000000000000000, 0.7087890813305628424, 1.000000000000000000),
 ( 1.000000000000000000, 0.7087532025278564518, 1.000000000000000000),
 ( 1.000000000000000000, 0.7087352638298917151, 1.000000000000000000),
 ( 1.000000000000000000, 0.7086455738595582865, 1.000000000000000000),
 ( 1.000000000000000000, 0.7085738331447311023, 1.000000000000000000),
 ( 1.000000000000000000, 0.7085021037179024539, 1.000000000000000000) ) ) 
 REPRESENTATION_ITEM ( '' )  SURFACE ( )  );
#29323 = CARTESIAN_POINT ( 'NONE',  ( -0.04947837552028493818, -0.4635165785490879542, -0.1137267105574193415 ) ) ;
#29324 = ADVANCED_FACE ( 'NONE', ( #31275 ), #29797, .F. ) ;
#29325 = CARTESIAN_POINT ( 'NONE',  ( 0.2574750998419692571, -1.178235494106686154, -0.5155029497116575543 ) ) ;
#29326 = EDGE_CURVE ( 'NONE', #25550, #26020, #6790, .T. ) ;
#29327 = CYLINDRICAL_SURFACE ( 'NONE', #13271, 0.03749999999977557397 ) ;
#29328 = CARTESIAN_POINT ( 'NONE',  ( 0.4763737863547038431, -1.078928959615589100, 0.8012595312036666639 ) ) ;
#29329 = CARTESIAN_POINT ( 'NONE',  ( 0.5161351604351521738, -1.173682792831946653, 0.4572090867639507783 ) ) ;
#29330 = DIRECTION ( 'NONE',  ( 0.000000000000000000, -0.5877852522924736922, -0.8090169943749470072 ) ) ;
#29331 = FACE_OUTER_BOUND ( 'NONE', #19827, .T. ) ;
#29332 = CIRCLE ( 'NONE', #39841, 0.1600000000000006140 ) ;
#29333 = CARTESIAN_POINT ( 'NONE',  ( 0.3303154085096511317, -1.292090888104762136, 0.5056921649335895941 ) ) ;
#29334 = CARTESIAN_POINT ( 'NONE',  ( 0.3836975776547298378, -1.127091824346511784, 0.7305314326323552043 ) ) ;
#29335 = CARTESIAN_POINT ( 'NONE',  ( 0.04230188431063450216, -0.2683773510969773013, 0.3842417364743009323 ) ) ;
#29336 = CARTESIAN_POINT ( 'NONE',  ( -0.03170752374382824340, -0.2433701302032818536, -0.4274053688542764351 ) ) ;
#29337 = ADVANCED_FACE ( 'NONE', ( #16044 ), #20620, .F. ) ;
#29338 = LOCAL_TIME ( 0, 53, 7.000000000000000000, #10729 ) ;
#29339 = ORIENTED_EDGE ( 'NONE', *, *, #32903, .F. ) ;
#29340 = PLANE ( 'NONE',  #24650 ) ;
#29341 = CARTESIAN_POINT ( 'NONE',  ( 0.5382307432915078849, -1.161159458769174257, 0.5682417262808779901 ) ) ;
#29342 = CARTESIAN_POINT ( 'NONE',  ( -0.02953079040095680369, -0.09152108205201929525, 0.5223162075576431862 ) ) ;
#29343 = DIRECTION ( 'NONE',  ( 0.000000000000000000, 0.000000000000000000, -1.000000000000000000 ) ) ;
#29344 = AXIS2_PLACEMENT_3D ( 'NONE', #13225, #13439, #37927 ) ;
#29345 = CARTESIAN_POINT ( 'NONE',  ( 0.05555397280954740835, -0.8368505189396914234, 0.1457185332388726828 ) ) ;
#29346 = ORIENTED_EDGE ( 'NONE', *, *, #21057, .F. ) ;
#29347 = CARTESIAN_POINT ( 'NONE',  ( -0.1524914371963946857, 0.4722463545162148280, 0.3472338286530670115 ) ) ;
#29348 = FACE_OUTER_BOUND ( 'NONE', #4432, .T. ) ;
#29349 = CARTESIAN_POINT ( 'NONE',  ( -0.3000000000000000999, -2.183180860297908144, -0.4937760292030871079 ) ) ;
#29350 = B_SPLINE_CURVE_WITH_KNOTS ( 'NONE', 3,
 ( #30193, #2023, #11685, #24053, #36160, #36579, #39864, #30610, #36762, #4888, #5277, #14552, #26917, #17455, #20950, #27121, #17842, #21150 ),
 .UNSPECIFIED., .F., .F.,
 ( 4, 2, 2, 2, 2, 2, 2, 2, 4 ),
 ( 0.000000000000000000, 0.0007746617437634293734, 0.001549323487526858747, 0.002323985231290287903, 0.003098646975053717494, 0.003873308718817147084, 0.004647970462580575807, 0.005422632206344005397, 0.006197293950107434987 ),
 .UNSPECIFIED. ) ;
#29351 = DIRECTION ( 'NONE',  ( -0.000000000000000000, 0.8090169943749540016, 0.5877852522924639223 ) ) ;
#29352 = CARTESIAN_POINT ( 'NONE',  ( 0.4906695346912424704, -1.277893297672507034, 0.5826988468483825789 ) ) ;
#29354 = DIRECTION ( 'NONE',  ( 0.000000000000000000, 0.7185945389473167300, -0.6954292836767037578 ) ) ;
#29353 = CARTESIAN_POINT ( 'NONE',  ( 0.01173648626945268322, -0.6872203660140956405, -0.1131804859792006068 ) ) ;
#29355 = CYLINDRICAL_SURFACE ( 'NONE', #37540, 0.03000000000000022787 ) ;
#29356 = EDGE_LOOP ( 'NONE', ( #8124, #27467, #20263, #31128 ) ) ;
#29357 = CARTESIAN_POINT ( 'NONE',  ( -0.1522836376793813007, 0.4715211068759145308, 0.3601997132473412355 ) ) ;
#29358 = EDGE_LOOP ( 'NONE', ( #33874, #35414, #30227, #4043, #1965, #3895 ) ) ;
#29359 = CARTESIAN_POINT ( 'NONE',  ( 0.4129595026082335529, -1.589300418172787666, 0.5636185827902593370 ) ) ;
#29361 = DIRECTION ( 'NONE',  ( 0.8185200378235019114, 0.4725162423735941863, -0.3267313091433876049 ) ) ;
#29360 = CARTESIAN_POINT ( 'NONE',  ( 0.08589675992784878700, -0.7862823833295263798, 0.07193548024800379415 ) ) ;
#29362 = CARTESIAN_POINT ( 'NONE',  ( 0.1242151342619402660, -1.295214500222888532, 0.4951799652504541571 ) ) ;
#29363 = ORIENTED_EDGE ( 'NONE', *, *, #3164, .T. ) ;
#29364 = ORIENTED_EDGE ( 'NONE', *, *, #39589, .F. ) ;
#29365 = CIRCLE ( 'NONE', #33975, 0.04249999999999994754 ) ;
#29366 = FACE_OUTER_BOUND ( 'NONE', #16293, .T. ) ;
#29367 = CARTESIAN_POINT ( 'NONE',  ( 0.5619293104143906481, -1.477014897282695527, 0.7041609149778610410 ) ) ;
#29368 = VERTEX_POINT ( 'NONE', #24901 ) ;
#29369 = CARTESIAN_POINT ( 'NONE',  ( 0.5442403261713570917, -1.629017118762910110, -0.4460973077508758600 ) ) ;
#29370 = CARTESIAN_POINT ( 'NONE',  ( 0.03875523708677968554, -0.4416911308383527079, 0.1785246905291560660 ) ) ;
#29371 = LOCAL_TIME ( 0, 53, 7.000000000000000000, #15841 ) ;
#29372 = CARTESIAN_POINT ( 'NONE',  ( 0.1852724517579373009, -0.8388905295248703098, 0.1482875376949696067 ) ) ;
#29373 = FACE_OUTER_BOUND ( 'NONE', #37230, .T. ) ;
#29374 = ADVANCED_FACE ( 'NONE', ( #37424 ), #38328, .T. ) ;
#29375 = CARTESIAN_POINT ( 'NONE',  ( 0.4520951681308373327, -1.683581237827290522, 0.6019770548139172783 ) ) ;
#29376 = CARTESIAN_POINT ( 'NONE',  ( 0.3853411735684887929, -1.756807109041803150, -0.4499573014716107822 ) ) ;
#29377 = CARTESIAN_POINT ( 'NONE',  ( 0.7308477326836637644, -1.487300591783543124, 0.7156276807793737760 ) ) ;
#29378 = DIRECTION ( 'NONE',  ( 1.000000000000000000, -2.099003099963423122E-12, 1.419325098918972248E-12 ) ) ;
#29379 = CARTESIAN_POINT ( 'NONE',  ( -0.01548846960707517956, -0.09061086148575756005, -0.5171215251571035232 ) ) ;
#29380 = CALENDAR_DATE ( 2026, 13, 10 ) ;
#29381 = DIRECTION ( 'NONE',  ( 0.4999551463232373427, -0.8660512985181134660, 0.000000000000000000 ) ) ;
#29382 = CARTESIAN_POINT ( 'NONE',  ( 0.04946288932099754398, 0.3082365379450883736, 0.3644333945507121642 ) ) ;
#29383 = CARTESIAN_POINT ( 'NONE',  ( 0.1849973320602424365, -0.7741433581987759993, -0.0006474567843166786907 ) ) ;
#29384 = DIRECTION ( 'NONE',  ( 0.000000000000000000, 0.7071067811865475727, -0.7071067811865474617 ) ) ;
#29385 = CARTESIAN_POINT ( 'NONE',  ( 0.08222542156928025481, -1.327483614382551247, 0.4683366274853974498 ) ) ;
#29386 = CARTESIAN_POINT ( 'NONE',  ( 0.1287314663193102893, -1.150224043500909454, 0.9169127589950010204 ) ) ;
#29387 = CARTESIAN_POINT ( 'NONE',  ( 0.5623653675682384057, -1.585032882041435665, -0.5293222829744327340 ) ) ;
#29388 = EDGE_CURVE ( 'NONE', #35103, #24257, #31324, .T. ) ;
#29389 = CARTESIAN_POINT ( 'NONE',  ( 0.03113248654051816583, 0.1428018198284763673, -0.2638325989215043466 ) ) ;
#29390 = APPLIED_PERSON_AND_ORGANIZATION_ASSIGNMENT ( #22900, #1492, ( #3089 ) ) ;
#29391 = CARTESIAN_POINT ( 'NONE',  ( 0.5461026827453100418, -1.628340864554156164, -0.5817929004078826738 ) ) ;
#29392 = CARTESIAN_POINT ( 'NONE',  ( -0.03170752374382538458, -0.3312811549923266874, 0.3635342706644953403 ) ) ;
#29393 = EDGE_CURVE ( 'NONE', #37794, #23886, #32455, .T. ) ;
#29394 = ORIENTED_EDGE ( 'NONE', *, *, #11681, .T. ) ;
#29395 = VERTEX_POINT ( 'NONE', #6969 ) ;
#29396 = CARTESIAN_POINT ( 'NONE',  ( 0.2316917763911649497, -1.232208891764917880, 0.5707417262808780478 ) ) ;
#29397 = ORIENTED_EDGE ( 'NONE', *, *, #33932, .F. ) ;
#29398 = CARTESIAN_POINT ( 'NONE',  ( -0.02000000000000000042, -2.542046649843399564, -0.2305290188067205537 ) ) ;
#29399 = DIRECTION ( 'NONE',  ( 0.9998941247116546194, -0.01455087607601020239, 0.0001066420868422379362 ) ) ;
#29400 = CARTESIAN_POINT ( 'NONE',  ( 0.3473220467592102456, -1.065780441090952380, 0.7836742237912034392 ) ) ;
#29402 = EDGE_LOOP ( 'NONE', ( #664, #10712, #21011, #38351, #8698, #36939 ) ) ;
#29401 = CARTESIAN_POINT ( 'NONE',  ( -0.1552002433785849012, 0.4812687096812816590, 0.09697487758652631462 ) ) ;
#29403 = CARTESIAN_POINT ( 'NONE',  ( 0.5291583206849711507, -1.148825028536799131, 0.6606389499358795714 ) ) ;
#29404 = CARTESIAN_POINT ( 'NONE',  ( 0.1153471662232078698, -0.4465907064269051263, 0.1457432652200511269 ) ) ;
#29405 = ORIENTED_EDGE ( 'NONE', *, *, #3469, .F. ) ;
#29406 = CARTESIAN_POINT ( 'NONE',  ( 0.4378213252392034738, -1.692012427937505281, -0.4124588244304266405 ) ) ;
#29407 = CARTESIAN_POINT ( 'NONE',  ( 0.3282947148789615577, -1.639384686062084873, 0.5920012551663509370 ) ) ;
#29409 = CARTESIAN_POINT ( 'NONE',  ( -0.01548846960712831414, -0.5203207976466733831, 0.08861466064782504148 ) ) ;
#29408 = CARTESIAN_POINT ( 'NONE',  ( 0.5431858176847103037, -1.654083725324065002, -0.4764654179353626229 ) ) ;
#29410 = CARTESIAN_POINT ( 'NONE',  ( 0.1436225252650951412, -1.283668529478381393, 0.4687417262808780127 ) ) ;
#29411 = CARTESIAN_POINT ( 'NONE',  ( 0.03398077991772324724, -1.810320368642273303, -0.3262651145211540871 ) ) ;
#29412 = ORIENTED_EDGE ( 'NONE', *, *, #22495, .F. ) ;
#29413 = PLANE ( 'NONE',  #5992 ) ;
#29414 = CARTESIAN_POINT ( 'NONE',  ( 0.2325478330093098400, -0.9400742174009236729, 0.4405423773235361273 ) ) ;
#29415 = CARTESIAN_POINT ( 'NONE',  ( 0.1876095839365603535, -1.270310460104811856, 0.4182417262808778013 ) ) ;
#29416 = LINE ( 'NONE', #1263, #38461 ) ;
#29417 = CARTESIAN_POINT ( 'NONE',  ( 0.2325139813020924151, -1.016947346993363421, 0.7211346862436321947 ) ) ;
#29418 = DIRECTION ( 'NONE',  ( 0.000000000000000000, 0.000000000000000000, 1.000000000000000000 ) ) ;
#29419 = EDGE_CURVE ( 'NONE', #30280, #15898, #19328, .T. ) ;
#29420 = CARTESIAN_POINT ( 'NONE',  ( 0.4753071910876713324, -1.208389221472485398, 0.5182417262812494263 ) ) ;
#29421 = CARTESIAN_POINT ( 'NONE',  ( -0.1167294259372894244, -0.5331983348239526244, 0.1528658435936947613 ) ) ;
#29422 = CARTESIAN_POINT ( 'NONE',  ( 0.04582713223189478768, 0.4790191777205491386, 0.08746099429787712598 ) ) ;
#29423 = CARTESIAN_POINT ( 'NONE',  ( 0.2923286432308245808, -1.660243258845594649, -0.3370932271639339728 ) ) ;
#29424 = DIRECTION ( 'NONE',  ( -0.4999551463232372872, 0.8660512985181134660, 0.000000000000000000 ) ) ;
#29425 = PERSON_AND_ORGANIZATION ( #28500, #32463 ) ;
#29426 = B_SPLINE_CURVE_WITH_KNOTS ( 'NONE', 3,
 ( #6339, #22003, #37600, #25278, #5733, #24683 ),
 .UNSPECIFIED., .F., .F.,
 ( 4, 2, 4 ),
 ( 0.007131418280723266293, 0.008047662360606964993, 0.008963906440490661959 ),
 .UNSPECIFIED. ) ;
#29427 = CARTESIAN_POINT ( 'NONE',  ( 0.06484759698365868963, -1.340577315853712870, 0.5772880505119728500 ) ) ;
#29428 = CARTESIAN_POINT ( 'NONE',  ( -0.2746410161513779258, -3.985676108854518507, -0.7623095129438225426 ) ) ;
#29429 = TOROIDAL_SURFACE ( 'NONE', #32682, 0.04999999999999998196, 0.2000000000000000111 ) ;
#29430 = PRODUCT_DEFINITION_CONTEXT ( 'detailed design', #23728, 'design' ) ;
#29431 = CARTESIAN_POINT ( 'NONE',  ( 0.1048700943662639051, -1.410537776362986273, 0.5685515072117806046 ) ) ;
#29432 = LINE ( 'NONE', #7612, #25169 ) ;
#29433 = CARTESIAN_POINT ( 'NONE',  ( 0.3938990593055637368, -1.751866802361104369, -0.5730325442411768888 ) ) ;
#29434 = CARTESIAN_POINT ( 'NONE',  ( -0.1205998369024041117, -0.5041491367644056476, 0.3197686713205454834 ) ) ;
#29435 = CARTESIAN_POINT ( 'NONE',  ( 0.3484677573834720765, -1.177852168535794330, 0.4282417262808829173 ) ) ;
#29436 = ORIENTED_EDGE ( 'NONE', *, *, #10360, .F. ) ;
#29437 = CARTESIAN_POINT ( 'NONE',  ( 0.1793623188593787554, -0.5490816427375126985, 0.2524024542104499891 ) ) ;
#29438 = ORIENTED_EDGE ( 'NONE', *, *, #17975, .F. ) ;
#29439 = CARTESIAN_POINT ( 'NONE',  ( 0.2691042938161366527, -1.674173831038697102, 0.5802809422378258919 ) ) ;
#29440 = CARTESIAN_POINT ( 'NONE',  ( 0.6019083329451311304, -1.483125660342571983, 0.5719604998333318591 ) ) ;
#29441 = ADVANCED_FACE ( 'NONE', ( #38836 ), #1243, .T. ) ;
#29443 = ORIENTED_EDGE ( 'NONE', *, *, #19009, .F. ) ;
#29442 = CARTESIAN_POINT ( 'NONE',  ( 0.5486165725604377208, -1.177731164730050351, 0.6033567833160039529 ) ) ;
#29445 = VERTEX_POINT ( 'NONE', #16252 ) ;
#29444 = VERTEX_POINT ( 'NONE', #7575 ) ;
#29446 = PERSON ( 'NAUO-PER3', 'UNSPECIFIED', 'UNSPECIFIED', ('UNSPECIFIED'), ('UNSPECIFIED'), ('UNSPECIFIED') ) ;
#29447 = CARTESIAN_POINT ( 'NONE',  ( 0.3292770240519934943, -1.177399294473852054, 0.4537878020085868713 ) ) ;
#29448 = ORIENTED_EDGE ( 'NONE', *, *, #18734, .F. ) ;
#29449 = VERTEX_POINT ( 'NONE', #23028 ) ;
#29450 = CARTESIAN_POINT ( 'NONE',  ( -0.01399985835776451290, -0.5261623171122247200, 0.1652506798037701730 ) ) ;
#29451 = DIRECTION ( 'NONE',  ( -0.4999551463232377313, 0.8660512985181132439, -0.000000000000000000 ) ) ;
#29452 = CARTESIAN_POINT ( 'NONE',  ( 0.6265145376157257306, -1.617582256290212017, -0.4718557182044338383 ) ) ;
#29453 = COORDINATED_UNIVERSAL_TIME_OFFSET ( 0, 0, .AHEAD. ) ;
#29454 = PLANE ( 'NONE',  #12588 ) ;
#29456 = ORIENTED_EDGE ( 'NONE', *, *, #2096, .T. ) ;
#29455 = VERTEX_POINT ( 'NONE', #23236 ) ;
#29457 = CARTESIAN_POINT ( 'NONE',  ( 0.2889289658470847177, -1.018197464890844062, 0.6953121150017608221 ) ) ;
#29458 = AXIS2_PLACEMENT_3D ( 'NONE', #570, #31570, #364 ) ;
#29459 = CARTESIAN_POINT ( 'NONE',  ( 0.1097081844868753736, -0.6901120672167371239, 0.4988169094206756915 ) ) ;
#29460 = CARTESIAN_POINT ( 'NONE',  ( 0.1100478739389431637, -0.5471989581415684922, 0.1536785690647612113 ) ) ;
#29461 = CARTESIAN_POINT ( 'NONE',  ( 0.03152558948873496192, -1.070130582242933892, 0.6176914086455537189 ) ) ;
#29462 = DIRECTION ( 'NONE',  ( 0.8660512985181132439, 0.4999551463232376758, 0.000000000000000000 ) ) ;
#29463 = CARTESIAN_POINT ( 'NONE',  ( -0.2399999999999999079, -2.183180860297908144, -0.4937760292030871079 ) ) ;
#29464 = DIRECTION ( 'NONE',  ( 1.000000000000000000, 0.000000000000000000, 7.588466649067360358E-16 ) ) ;
#29465 = CARTESIAN_POINT ( 'NONE',  ( 0.4134082608409563320, -1.687121258993206308, -0.4232165953256796231 ) ) ;
#29466 = CARTESIAN_POINT ( 'NONE',  ( 0.06086249397362281099, -1.332142734742522538, 0.5449151288494182843 ) ) ;
#29467 = FACE_OUTER_BOUND ( 'NONE', #5948, .T. ) ;
#29468 = CARTESIAN_POINT ( 'NONE',  ( 0.1994740068363788088, -2.042640899752901529, -0.2765909798240095974 ) ) ;
#29469 = CARTESIAN_POINT ( 'NONE',  ( 0.01155337267041268469, -0.8469566264145796941, -0.05879553897425002923 ) ) ;
#29470 = CARTESIAN_POINT ( 'NONE',  ( 0.5630304050329183463, -1.440913006158521359, 0.7429145406160999610 ) ) ;
#29471 = CARTESIAN_POINT ( 'NONE',  ( 0.6409058204046232943, -1.459016202299332710, -0.5155029497116575543 ) ) ;
#29472 = DIRECTION ( 'NONE',  ( 0.000000000000000000, 0.000000000000000000, 1.000000000000000000 ) ) ;
#29473 = CARTESIAN_POINT ( 'NONE',  ( 0.0002700364102348538193, -0.8386493658592084621, 0.3780876778669690075 ) ) ;
#29474 = CARTESIAN_POINT ( 'NONE',  ( 0.1892170003689550017, -0.8723299121346327345, 0.2416867767302488257 ) ) ;
#29475 = DATE_AND_TIME ( #26396, #37786 ) ;
#29476 = CARTESIAN_POINT ( 'NONE',  ( 0.6396239940202712582, -1.336901993116134779, 0.8551876651762376769 ) ) ;
#29477 = CARTESIAN_POINT ( 'NONE',  ( 0.5058599984363495450, -1.583313914148366752, -0.4933326546058600659 ) ) ;
#29478 = CARTESIAN_POINT ( 'NONE',  ( 0.4884077276296390213, -1.184991248043463452, 0.4182417262808778013 ) ) ;
#29479 = ORIENTED_EDGE ( 'NONE', *, *, #5444, .F. ) ;
#29480 = CARTESIAN_POINT ( 'NONE',  ( 0.1999999999999759193, -1.905617227352954135, -0.6587955718153066798 ) ) ;
#29481 = CARTESIAN_POINT ( 'NONE',  ( 0.07216878364870311924, 0.05141091571461162829, 0.1249999999999999029 ) ) ;
#29482 = CARTESIAN_POINT ( 'NONE',  ( 0.09041522251730070570, -1.303513460825282078, 0.4577461224782632954 ) ) ;
#29483 = VERTEX_POINT ( 'NONE', #13743 ) ;
#29484 = CARTESIAN_POINT ( 'NONE',  ( 0.5473076987003111515, -1.651760216406904513, -0.4929644493450987541 ) ) ;
#29485 = EDGE_CURVE ( 'NONE', #27531, #37987, #40335, .T. ) ;
#29486 = CARTESIAN_POINT ( 'NONE',  ( 0.4845724100169539472, -1.091512197975673670, 0.8037230719241761356 ) ) ;
#29488 = ORIENTED_EDGE ( 'NONE', *, *, #16129, .T. ) ;
#29487 = ORIENTED_EDGE ( 'NONE', *, *, #33818, .F. ) ;
#29489 = DIRECTION ( 'NONE',  ( 0.000000000000000000, 0.5877852522924961187, 0.8090169943749307979 ) ) ;
#29490 = EDGE_LOOP ( 'NONE', ( #22236, #20238, #1596, #34741, #23411, #5768 ) ) ;
#29491 = CARTESIAN_POINT ( 'NONE',  ( 0.3566968277947379362, -1.787709349577662810, -0.5192541119936813221 ) ) ;
#29492 = B_SPLINE_CURVE_WITH_KNOTS ( 'NONE', 3,
 ( #36577, #10664, #39051, #17454 ),
 .UNSPECIFIED., .F., .F.,
 ( 4, 4 ),
 ( 2.100114060352324785E-15, 0.0003951776346070152404 ),
 .UNSPECIFIED. ) ;
#29493 = PRODUCT ( 'Parallelogram front_REAR', 'Parallelogram front_REAR', '', ( #27210 ) ) ;
#29494 = B_SPLINE_CURVE_WITH_KNOTS ( 'NONE', 3,
 ( #39276, #30029, #5298, #14574 ),
 .UNSPECIFIED., .F., .F.,
 ( 4, 4 ),
 ( -1.150894640811756038E-05, 0.0005747792170237640656 ),
 .UNSPECIFIED. ) ;
#29495 = DIRECTION ( 'NONE',  ( -1.000000000000000000, 0.000000000000000000, 0.000000000000000000 ) ) ;
#29496 = EDGE_CURVE ( 'NONE', #38085, #25046, #26550, .T. ) ;
#29497 = CARTESIAN_POINT ( 'NONE',  ( -0.05489899477340622752, 0.4472784955204432422, -0.1186631084353777094 ) ) ;
#29498 = ORIENTED_EDGE ( 'NONE', *, *, #29276, .T. ) ;
#29499 = CARTESIAN_POINT ( 'NONE',  ( 0.5394930253215350913, -1.186018807470103908, 0.9907910187352456655 ) ) ;
#29500 = ADVANCED_FACE ( 'NONE', ( #7352 ), #10665, .F. ) ;
#29501 = CARTESIAN_POINT ( 'NONE',  ( 0.09120750288997202249, -0.6506232390852273451, 0.2347779848227966037 ) ) ;
#29502 = CYLINDRICAL_SURFACE ( 'NONE', #397, 0.07999999999999996003 ) ;
#29503 = CARTESIAN_POINT ( 'NONE',  ( 0.4289323656347681646, -1.412113752792893751, 0.8314756505790452668 ) ) ;
#29505 = CARTESIAN_POINT ( 'NONE',  ( -0.1137534828624003069, -0.5201328034396339728, 0.1183403147931640503 ) ) ;
#29504 = CARTESIAN_POINT ( 'NONE',  ( 0.1135111366450400200, -0.6246916037217551398, -0.08750969994112312023 ) ) ;
#29506 = CARTESIAN_POINT ( 'NONE',  ( 0.1591190474269453259, -0.9387514653284979582, 0.3780444062633597224 ) ) ;
#29507 = ORIENTED_EDGE ( 'NONE', *, *, #38152, .T. ) ;
#29508 = ORIENTED_EDGE ( 'NONE', *, *, #6627, .T. ) ;
#29509 = DIRECTION ( 'NONE',  ( 1.000000000000000000, 2.403560570595280416E-31, 1.417484439069005150E-31 ) ) ;
#29510 = CARTESIAN_POINT ( 'NONE',  ( 0.1909569983300636875, -0.4822605344198281907, 0.2607227880177884760 ) ) ;
#29511 = DIRECTION ( 'NONE',  ( -0.9848077530122080203, 0.000000000000000000, -0.1736481776669303589 ) ) ;
#29512 = EDGE_CURVE ( 'NONE', #14911, #21211, #35724, .T. ) ;
#29513 = APPROVAL ( #2318, 'UNSPECIFIED' ) ;
#29514 = DIRECTION ( 'NONE',  ( -0.4999999999999991118, 0.000000000000000000, 0.8660254037844391517 ) ) ;
#29515 = CARTESIAN_POINT ( 'NONE',  ( 0.002079598126425303162, -0.4942866788504220454, 0.1457185332388685473 ) ) ;
#29516 = CARTESIAN_POINT ( 'NONE',  ( 0.1169689867097839509, -1.415244282406541210, 0.5045617156522553826 ) ) ;
#29517 = CARTESIAN_POINT ( 'NONE',  ( 0.5308880977089266429, -1.160028955924689242, 0.7442320808281387423 ) ) ;
#29518 = CARTESIAN_POINT ( 'NONE',  ( -0.05464101615137761936, -1.851224977018630868, -0.7958870385335592434 ) ) ;
#29519 = CARTESIAN_POINT ( 'NONE',  ( 0.02304082380077634995, -0.9164601304410119331, 0.5704413390923104288 ) ) ;
#29520 = CARTESIAN_POINT ( 'NONE',  ( 0.03819165667510639878, -1.740319606980962996, -0.3346916167941055842 ) ) ;
#29521 = CARTESIAN_POINT ( 'NONE',  ( 0.2815322486459076456, -1.024220253226221011, 0.7266672233242934542 ) ) ;
#29522 = CARTESIAN_POINT ( 'NONE',  ( 0.02231181081520604292, -0.2417894035777214679, 0.4519954025055065716 ) ) ;
#29523 = CARTESIAN_POINT ( 'NONE',  ( -0.02881302694829455252, -0.2420344415834868312, -0.4354517411081167966 ) ) ;
#29524 = ORIENTED_EDGE ( 'NONE', *, *, #38086, .T. ) ;
#29525 = DIRECTION ( 'NONE',  ( 0.000000000000000000, -0.8585432690668222122, 0.5127411190260187102 ) ) ;
#29526 = EDGE_LOOP ( 'NONE', ( #10432, #16791, #23893, #7348 ) ) ;
#29527 = CARTESIAN_POINT ( 'NONE',  ( 0.08991878951126530684, -0.5648332908254826146, 0.1536871759036723961 ) ) ;
#29528 = CARTESIAN_POINT ( 'NONE',  ( 0.02999999938246960748, -2.094414908375987761, -0.7275123218652694845 ) ) ;
#29529 = CARTESIAN_POINT ( 'NONE',  ( 0.3922483900791164935, -1.141226917602951474, 0.4803897171336208860 ) ) ;
#29530 = CARTESIAN_POINT ( 'NONE',  ( 0.08221648783320979759, -0.8838808657549234171, 0.5149684988968940003 ) ) ;
#29531 = ORIENTED_EDGE ( 'NONE', *, *, #3448, .T. ) ;
#29532 = ADVANCED_FACE ( 'NONE', ( #29587 ), #6758, .T. ) ;
#29533 = CARTESIAN_POINT ( 'NONE',  ( -0.1603938765018607104, 0.4636889572247930857, 0.3382895567580836982 ) ) ;
#29534 = CARTESIAN_POINT ( 'NONE',  ( 0.1499999999999996336, 0.07651041855119851409, 0.5222379212568192264 ) ) ;
#29535 = CARTESIAN_POINT ( 'NONE',  ( 0.1733459996405724013, -1.382560672001245772, 0.4245314550594288527 ) ) ;
#29536 = FACE_OUTER_BOUND ( 'NONE', #11235, .T. ) ;
#29537 = EDGE_CURVE ( 'NONE', #8017, #13521, #14611, .T. ) ;
#29538 = CARTESIAN_POINT ( 'NONE',  ( 0.3375807384838437897, -1.070557502036374897, 0.7199277723466692702 ) ) ;
#29540 = DIRECTION ( 'NONE',  ( 0.2213665493037340615, -0.07887541654787479095, -0.9719956376001678278 ) ) ;
#29539 = DIRECTION ( 'NONE',  ( 0.000000000000000000, 0.000000000000000000, -1.000000000000000000 ) ) ;
#29541 = EDGE_CURVE ( 'NONE', #5190, #33568, #12090, .T. ) ;
#29542 = CARTESIAN_POINT ( 'NONE',  ( 0.2615876942762666579, -0.9557769062746830357, 0.5027841231788432452 ) ) ;
#29543 = VERTEX_POINT ( 'NONE', #28975 ) ;
#29544 = EDGE_CURVE ( 'NONE', #2027, #35001, #38666, .T. ) ;
#29545 = CARTESIAN_POINT ( 'NONE',  ( -0.2399999999999999079, -2.231697337611688425, -0.6193912371520073901 ) ) ;
#29546 = EDGE_LOOP ( 'NONE', ( #35456, #12143, #14204, #29143, #14324, #11679, #7258 ) ) ;
#29547 =( BOUNDED_SURFACE ( )  B_SPLINE_SURFACE ( 3, 2, ( 
 ( #16193, #7095, #15762 ),
 ( #28521, #28732, #18873 ),
 ( #12672, #25859, #6302 ),
 ( #22175, #181, #593 ),
 ( #22781, #19664, #6902 ),
 ( #37776, #31602, #9598 ),
 ( #12895, #9998, #32009 ),
 ( #16375, #28311, #13087 ) ),
 .UNSPECIFIED., .F., .F., .T. ) 
 B_SPLINE_SURFACE_WITH_KNOTS ( ( 4, 2, 2, 4 ),
 ( 3, 3 ),
 ( 0.001521769427996497474, 0.002374549442172081172, 0.002800939449259872913, 0.003227329456347664653 ),
 ( 0.000000000000000000, 1.000000000000000000 ),
 .UNSPECIFIED. ) 
 GEOMETRIC_REPRESENTATION_ITEM ( )  RATIONAL_B_SPLINE_SURFACE ( (
 ( 1.000000000000000000, 0.4512702095618630893, 1.000000000000000000),
 ( 1.000000000000000000, 0.4832373129657441813, 1.000000000000000000),
 ( 1.000000000000000000, 0.5089024703303249852, 1.000000000000000000),
 ( 1.000000000000000000, 0.5356172533981554684, 1.000000000000000000),
 ( 1.000000000000000000, 0.5425363809967062023, 1.000000000000000000),
 ( 1.000000000000000000, 0.5510866447777388322, 1.000000000000000000),
 ( 1.000000000000000000, 0.5527681761118921067, 1.000000000000000000),
 ( 1.000000000000000000, 0.5517613080878603915, 1.000000000000000000) ) ) 
 REPRESENTATION_ITEM ( '' )  SURFACE ( )  );
#29548 = CARTESIAN_POINT ( 'NONE',  ( 0.4155094897012233113, -1.589296793549693776, 0.6069686941225849175 ) ) ;
#29550 = CARTESIAN_POINT ( 'NONE',  ( 0.4666806433631038864, -1.098312294252236532, -0.6371104447086228806 ) ) ;
#29549 = CARTESIAN_POINT ( 'NONE',  ( 0.06808939212415124342, -0.5886288129379394496, 0.03568275504429443967 ) ) ;
#29551 = CARTESIAN_POINT ( 'NONE',  ( 5.543712964093851419E-16, -0.3059742766594579222, 0.06173076923076769446 ) ) ;
#29552 = EDGE_LOOP ( 'NONE', ( #15721, #8938, #39707, #32125, #1093 ) ) ;
#29553 = EDGE_LOOP ( 'NONE', ( #24048, #28183 ) ) ;
#29554 = CARTESIAN_POINT ( 'NONE',  ( 2.048885995248197414E-16, 0.2900000000000004796, -5.122214988120493288E-16 ) ) ;
#29555 = CARTESIAN_POINT ( 'NONE',  ( 0.5672008999325364176, -1.484259169383562726, 0.6868322779169411252 ) ) ;
#29556 = VERTEX_POINT ( 'NONE', #18059 ) ;
#29557 = CARTESIAN_POINT ( 'NONE',  ( 0.05999999999999990757, 0.2954784694557334168, 0.05188905557145093855 ) ) ;
#29558 = DIRECTION ( 'NONE',  ( -1.000000000000000000, -0.000000000000000000, -0.000000000000000000 ) ) ;
#29559 = EDGE_CURVE ( 'NONE', #28660, #19775, #8382, .T. ) ;
#29560 = CARTESIAN_POINT ( 'NONE',  ( -0.3000000000000000999, -3.747168848490688209, -0.4747258284076885104 ) ) ;
#29561 = CARTESIAN_POINT ( 'NONE',  ( 0.09263126791059923815, -1.302225538099672564, 0.4543134729207104483 ) ) ;
#29562 = CIRCLE ( 'NONE', #17081, 0.06250000000000000000 ) ;
#29563 = FACE_OUTER_BOUND ( 'NONE', #36615, .T. ) ;
#29564 = FACE_OUTER_BOUND ( 'NONE', #19726, .T. ) ;
#29565 = CARTESIAN_POINT ( 'NONE',  ( 0.7188893830798498419, -1.468416639873279861, 0.6609592937859087858 ) ) ;
#29566 = CIRCLE ( 'NONE', #6641, 0.9087847906030128708 ) ;
#29567 = DIRECTION ( 'NONE',  ( 0.000000000000000000, 0.000000000000000000, -1.000000000000000000 ) ) ;
#29568 = CARTESIAN_POINT ( 'NONE',  ( 0.1734973056165642902, -1.209394307038482497, -0.5155029497116575543 ) ) ;
#29569 = DATE_AND_TIME ( #19521, #38402 ) ;
#29570 = B_SPLINE_CURVE_WITH_KNOTS ( 'NONE', 3,
 ( #6651, #19439, #37516, #2987, #37737, #6453, #3586, #9558 ),
 .UNSPECIFIED., .F., .F.,
 ( 4, 2, 2, 4 ),
 ( 0.000000000000000000, 0.0006248974353471740181, 0.001249794870694348036, 0.002499589741388694771 ),
 .UNSPECIFIED. ) ;
#29571 = CARTESIAN_POINT ( 'NONE',  ( 0.6626494750595320893, -1.486816775434632865, -0.6188922402621547247 ) ) ;
#29572 = CARTESIAN_POINT ( 'NONE',  ( 0.05201840200954800653, 0.2909588945328520637, 0.3697186091640849437 ) ) ;
#29573 = CARTESIAN_POINT ( 'NONE',  ( 0.1843345887713713493, -0.8498185637792359248, 0.1049832382102776629 ) ) ;
#29574 = CARTESIAN_POINT ( 'NONE',  ( 0.6962239684629863978, -1.427522162457817601, 0.6057417262800831592 ) ) ;
#29575 = CARTESIAN_POINT ( 'NONE',  ( 0.1504531896226799503, -1.289993790327085499, 0.4182417262808776903 ) ) ;
#29576 = CARTESIAN_POINT ( 'NONE',  ( 0.1172021019593823543, -1.233981478044366087, 0.8520562743190572830 ) ) ;
#29577 = CARTESIAN_POINT ( 'NONE',  ( 0.5818810567066877715, -1.520385204644366439, -0.5792601642121770755 ) ) ;
#29578 = DIRECTION ( 'NONE',  ( 0.000000000000000000, 0.000000000000000000, -1.000000000000000000 ) ) ;
#29579 = CARTESIAN_POINT ( 'NONE',  ( 0.1876053338355621880, -0.6785855078148245179, 0.1477569985384105666 ) ) ;
#29580 = CARTESIAN_POINT ( 'NONE',  ( -0.03877220711930361857, -0.2524486846094400883, 0.4039751870151983559 ) ) ;
#29581 = ORIENTED_EDGE ( 'NONE', *, *, #19111, .T. ) ;
#29582 = VERTEX_POINT ( 'NONE', #23841 ) ;
#29583 = ADVANCED_FACE ( 'NONE', ( #11487 ), #38357, .T. ) ;
#29584 = FACE_OUTER_BOUND ( 'NONE', #37679, .T. ) ;
#29585 = ORIENTED_EDGE ( 'NONE', *, *, #32637, .F. ) ;
#29586 = CARTESIAN_POINT ( 'NONE',  ( -19685.04449858789303, 285.6128717395195622, -1.951739244310253252 ) ) ;
#29587 = FACE_OUTER_BOUND ( 'NONE', #34505, .T. ) ;
#29588 = EDGE_CURVE ( 'NONE', #5909, #26696, #29178, .T. ) ;
#29589 = CARTESIAN_POINT ( 'NONE',  ( 0.5680601962060586319, -1.407955926830466442, 0.6709332758665339513 ) ) ;
#29590 = CIRCLE ( 'NONE', #15137, 0.01500000000000004455 ) ;
#29592 = VERTEX_POINT ( 'NONE', #33280 ) ;
#29591 = CARTESIAN_POINT ( 'NONE',  ( -0.1508021419688959364, 0.4665171419162750799, 0.1089215716837025061 ) ) ;
#29593 = CARTESIAN_POINT ( 'NONE',  ( 0.2389902554220701691, -0.8445547280628969977, 0.4765619450694277281 ) ) ;
#29594 = EDGE_CURVE ( 'NONE', #13090, #11795, #29350, .T. ) ;
#29595 = CARTESIAN_POINT ( 'NONE',  ( -2.112273405726188513E-14, -2.097675824466503691, -0.2907077406111384099 ) ) ;
#29596 = ORIENTED_EDGE ( 'NONE', *, *, #25341, .F. ) ;
#29597 = DIRECTION ( 'NONE',  ( -1.000000000000000000, -6.779273404243070203E-32, -4.314083075427408311E-32 ) ) ;
#29598 = ORIENTED_EDGE ( 'NONE', *, *, #28300, .F. ) ;
#29599 = AXIS2_PLACEMENT_3D ( 'NONE', #25090, #27770, #9448 ) ;
#29600 = CARTESIAN_POINT ( 'NONE',  ( 0.03921977259664061882, -0.6520487650187948292, 0.4637041238408874944 ) ) ;
#29602 = CARTESIAN_POINT ( 'NONE',  ( 0.1122840140760263117, -0.8147850859242622423, -0.05910278775682942243 ) ) ;
#29601 = CARTESIAN_POINT ( 'NONE',  ( 0.6805229833934419714, -1.519090101737586629, 0.4475704587218782837 ) ) ;
#29603 = CARTESIAN_POINT ( 'NONE',  ( 0.3206535937437295369, -1.182295409031864697, 0.3157417262808777658 ) ) ;
#29604 = CARTESIAN_POINT ( 'NONE',  ( 0.1465864560099491842, -1.332653898859956332, -0.3147756667838505495 ) ) ;
#29605 = EDGE_LOOP ( 'NONE', ( #13107, #30617, #21653 ) ) ;
#29606 = DIRECTION ( 'NONE',  ( -8.881784197001246407E-16, 2.361472542561082612E-16, -1.000000000000000000 ) ) ;
#29607 = CARTESIAN_POINT ( 'NONE',  ( 0.05361885722424606510, -1.467584822755955143, -0.6509794481950387235 ) ) ;
#29608 = CARTESIAN_POINT ( 'NONE',  ( 0.02235124290213184178, 0.4612278572487581441, 0.2234747101372496769 ) ) ;
#29609 = EDGE_CURVE ( 'NONE', #39909, #20959, #7970, .T. ) ;
#29610 = CARTESIAN_POINT ( 'NONE',  ( 0.3139280916366145591, -1.155011946012813429, 0.7357575621586726067 ) ) ;
#29611 = CARTESIAN_POINT ( 'NONE',  ( -0.2399999999999999079, -2.425196952834860920, -0.6298687015330038941 ) ) ;
#29612 = ADVANCED_FACE ( 'NONE', ( #40048 ), #30004, .F. ) ;
#29613 = FACE_OUTER_BOUND ( 'NONE', #1476, .T. ) ;
#29614 = EDGE_CURVE ( 'NONE', #16113, #29483, #14972, .T. ) ;
#29615 = CARTESIAN_POINT ( 'NONE',  ( 0.4264404822470678758, -1.236583032262235982, 0.5509909139845965420 ) ) ;
#29616 = DIRECTION ( 'NONE',  ( 0.000000000000000000, 0.000000000000000000, -1.000000000000000000 ) ) ;
#29617 = FACE_OUTER_BOUND ( 'NONE', #27380, .T. ) ;
#29618 = CARTESIAN_POINT ( 'NONE',  ( 0.4460585320772065820, -1.103542852913448558, -0.6309016134502297701 ) ) ;
#29619 = CARTESIAN_POINT ( 'NONE',  ( 0.1780079192261909971, -1.275848360495260847, 0.4182417262808778013 ) ) ;
#29620 = PERSON_AND_ORGANIZATION_ROLE ( 'design_supplier' ) ;
#29621 = AXIS2_PLACEMENT_3D ( 'NONE', #14878, #18160, #33576 ) ;
#29622 = CARTESIAN_POINT ( 'NONE',  ( 0.3860850745295709152, -1.140406926820327183, 0.4308008161134124214 ) ) ;
#29623 = CARTESIAN_POINT ( 'NONE',  ( 0.3320003377790358146, -1.522026588550927428, -0.7092149976984114534 ) ) ;
#29624 = DIRECTION ( 'NONE',  ( -0.7723395547766002123, 0.000000000000000000, 0.6352098961189780457 ) ) ;
#29625 = AXIS2_PLACEMENT_3D ( 'NONE', #5488, #31004, #21755 ) ;
#29626 = VECTOR ( 'NONE', #34179, 39.37007874015748854 ) ;
#29627 = CARTESIAN_POINT ( 'NONE',  ( -0.1743922129835736579, -0.5166151207188712791, 0.3599999999999997091 ) ) ;
#29628 = CARTESIAN_POINT ( 'NONE',  ( 0.3790501254121775299, -1.751389653868420826, -0.5849892083899181916 ) ) ;
#29629 = AXIS2_PLACEMENT_3D ( 'NONE', #19890, #1202, #3440 ) ;
#29630 = DIRECTION ( 'NONE',  ( 0.4999999999999969469, -0.5122356157878158456, -0.6982941170584784363 ) ) ;
#29631 = CARTESIAN_POINT ( 'NONE',  ( 0.03662792686184383056, -0.04111994379180358705, -0.4792679903722390500 ) ) ;
#29632 = VERTEX_POINT ( 'NONE', #33472 ) ;
#29633 = ORIENTED_EDGE ( 'NONE', *, *, #15748, .T. ) ;
#29634 = CARTESIAN_POINT ( 'NONE',  ( 0.4103422353672772083, -1.716666388523393705, 0.4257348284579867137 ) ) ;
#29635 = EDGE_LOOP ( 'NONE', ( #7089, #8617, #26530 ) ) ;
#29636 = CARTESIAN_POINT ( 'NONE',  ( 1.893270629535517794E-16, 0.3059742766594581997, -0.06173076923076962347 ) ) ;
#29637 = EDGE_CURVE ( 'NONE', #21878, #38042, #21290, .T. ) ;
#29638 = CARTESIAN_POINT ( 'NONE',  ( 0.1786157546805342555, -0.7241356608248309401, 0.5263052784706855336 ) ) ;
#29640 = ORIENTED_EDGE ( 'NONE', *, *, #9314, .F. ) ;
#29639 = CARTESIAN_POINT ( 'NONE',  ( -0.002079317817372410872, -0.8425701894467937381, 0.1068513513423657718 ) ) ;
#29641 = ADVANCED_FACE ( 'NONE', ( #23453 ), #12729, .T. ) ;
#29642 = ORIENTED_EDGE ( 'NONE', *, *, #9029, .T. ) ;
#29643 = CARTESIAN_POINT ( 'NONE',  ( 0.4695634368055122132, -1.162243873490485857, 0.8979758211665889167 ) ) ;
#29644 = ORIENTED_EDGE ( 'NONE', *, *, #25225, .T. ) ;
#29645 = CARTESIAN_POINT ( 'NONE',  ( 0.01047931697485390834, -0.7075287188305212638, 0.5611176339341903407 ) ) ;
#29647 = CARTESIAN_POINT ( 'NONE',  ( -0.02000000000000000042, -1.599201040860868339, 0.1642182323853691728 ) ) ;
#29646 = FACE_OUTER_BOUND ( 'NONE', #28803, .T. ) ;
#29648 = DIRECTION ( 'NONE',  ( -8.881784197001246407E-16, 2.361472542561082612E-16, -1.000000000000000000 ) ) ;
#29649 = DATE_TIME_ROLE ( 'classification_date' ) ;
#29650 = FACE_OUTER_BOUND ( 'NONE', #13280, .T. ) ;
#29652 = ORIENTED_EDGE ( 'NONE', *, *, #39949, .T. ) ;
#29651 = ORIENTED_EDGE ( 'NONE', *, *, #40140, .F. ) ;
#29653 = VECTOR ( 'NONE', #8624, 39.37007874015748143 ) ;
#29654 = CARTESIAN_POINT ( 'NONE',  ( 0.1108980406011375874, -0.8361979591902880538, 0.3952538393652093585 ) ) ;
#29655 = CARTESIAN_POINT ( 'NONE',  ( 0.01903588135871963488, -0.9012985171311311827, 0.5348354971068303154 ) ) ;
#29656 = CARTESIAN_POINT ( 'NONE',  ( 0.1404538855177946133, -0.7360681509722835081, 0.5151525649323883682 ) ) ;
#29657 = AXIS2_PLACEMENT_3D ( 'NONE', #7257, #32977, #3982 ) ;
#29658 = CARTESIAN_POINT ( 'NONE',  ( 0.5528385491747893621, -1.511151847756054156, 0.5706625526926106806 ) ) ;
#29659 = CARTESIAN_POINT ( 'NONE',  ( 0.1883287559378439002, -0.5374260242839021817, 0.2815551403220473148 ) ) ;
#29660 = CARTESIAN_POINT ( 'NONE',  ( 0.4616332724396642329, -1.592054364389571042, -0.4300420834888027954 ) ) ;
#29661 = VECTOR ( 'NONE', #20800, 39.37007874015748143 ) ;
#29662 = CARTESIAN_POINT ( 'NONE',  ( -0.1684323895664684156, 0.5231977504175356897, 0.1528658435937000626 ) ) ;
#29663 = CIRCLE ( 'NONE', #11917, 0.1550424246542357609 ) ;
#29664 = DIRECTION ( 'NONE',  ( -1.000000000000000000, -2.280301054154495132E-31, 1.664003471950577689E-31 ) ) ;
#29665 = PLANE ( 'NONE',  #28572 ) ;
#29666 = CARTESIAN_POINT ( 'NONE',  ( 0.07671776034818365841, -1.321070999986371231, 0.4807624541185260836 ) ) ;
#29667 = DIRECTION ( 'NONE',  ( -3.543711097672501380E-32, -0.8983234858819668656, -0.4393346272636287630 ) ) ;
#29668 = CARTESIAN_POINT ( 'NONE',  ( 1.988800862544524313E-06, -0.6187814307215226961, -0.1067078381776963153 ) ) ;
#29669 = CARTESIAN_POINT ( 'NONE',  ( 0.5016706962953397797, -1.333249415785642489, 0.8067160742835506326 ) ) ;
#29670 = DIRECTION ( 'NONE',  ( 1.000000000000000000, 2.280301054154495132E-31, -1.664003471950577689E-31 ) ) ;
#29671 = CIRCLE ( 'NONE', #3378, 0.08000000000000000167 ) ;
#29672 = DIMENSIONAL_EXPONENTS ( 1.000000000000000000, 0.000000000000000000, 0.000000000000000000, 0.000000000000000000, 0.000000000000000000, 0.000000000000000000, 0.000000000000000000 ) ;
#29673 = LINE ( 'NONE', #11573, #14001 ) ;
#29674 = CARTESIAN_POINT ( 'NONE',  ( 0.1851448419613674068, -1.516587896426844662, 0.7176110508928341680 ) ) ;
#29675 = CARTESIAN_POINT ( 'NONE',  ( 0.2669631944262408907, -0.9256872934665847374, 0.5220607882127416000 ) ) ;
#29676 = APPROVAL_ROLE ( '' ) ;
#29677 = CARTESIAN_POINT ( 'NONE',  ( 0.7032651991748780640, -1.440401145529036642, 0.7869155231269625572 ) ) ;
#29678 = CARTESIAN_POINT ( 'NONE',  ( 0.4078704035844273323, -1.593543170983706236, -0.6183053384820467180 ) ) ;
#29679 = CARTESIAN_POINT ( 'NONE',  ( 0.3110401053545825412, -1.761569117269722540, 0.5684230042337896638 ) ) ;
#29680 = AXIS2_PLACEMENT_3D ( 'NONE', #19402, #31937, #3755 ) ;
#29681 = CIRCLE ( 'NONE', #36247, 0.4615209409081865166 ) ;
#29682 = ORIENTED_EDGE ( 'NONE', *, *, #10982, .F. ) ;
#29683 = CARTESIAN_POINT ( 'NONE',  ( -2.112273405726188513E-14, -1.837418632672298768, -0.6339733133327630776 ) ) ;
#29684 = CARTESIAN_POINT ( 'NONE',  ( 0.002368078414000984559, -0.5283436918108032065, 0.1537378385375844370 ) ) ;
#29685 = AXIS2_PLACEMENT_3D ( 'NONE', #12576, #25137, #22074 ) ;
#29686 = DIRECTION ( 'NONE',  ( -0.4999551463232372317, 0.8660512985181135770, -0.000000000000000000 ) ) ;
#29688 = ORIENTED_EDGE ( 'NONE', *, *, #33140, .T. ) ;
#29687 = FACE_BOUND ( 'NONE', #36777, .T. ) ;
#29689 = CARTESIAN_POINT ( 'NONE',  ( 0.3219857165489924955, -1.758039968903889916, 0.4848815471996642534 ) ) ;
#29690 = B_SPLINE_CURVE_WITH_KNOTS ( 'NONE', 3,
 ( #22909, #1504, #32739, #11142, #4357, #10348, #1712, #26593 ),
 .UNSPECIFIED., .F., .F.,
 ( 4, 2, 2, 4 ),
 ( 0.000000000000000000, 0.001004989706391617261, 0.001507484559587425133, 0.002009979412783232788 ),
 .UNSPECIFIED. ) ;
#29691 = CARTESIAN_POINT ( 'NONE',  ( 0.3857344834571298509, -0.9392921734164567660, 0.7474990102649032853 ) ) ;
#29693 = EDGE_LOOP ( 'NONE', ( #28682, #18897, #37315, #13352, #34283 ) ) ;
#29692 = ORIENTED_EDGE ( 'NONE', *, *, #36555, .F. ) ;
#29694 = CARTESIAN_POINT ( 'NONE',  ( 0.03022635123008331204, -1.916038177046143876, -0.6843378419889921682 ) ) ;
#29695 = ORIENTED_EDGE ( 'NONE', *, *, #12982, .T. ) ;
#29696 = CARTESIAN_POINT ( 'NONE',  ( 0.3595056509374958686, -1.929564378396709357, -0.4933486092489832719 ) ) ;
#29697 = CARTESIAN_POINT ( 'NONE',  ( 0.3434711319545033503, -1.169169302084718254, 0.4182417262808778013 ) ) ;
#29698 = CARTESIAN_POINT ( 'NONE',  ( -0.05544444631433655818, 0.4320262549500590299, -0.1617187101067759925 ) ) ;
#29699 = ORIENTED_EDGE ( 'NONE', *, *, #14816, .T. ) ;
#29700 = CARTESIAN_POINT ( 'NONE',  ( 0.2209260011871197193, -1.309027873449325918, -0.4125659523519145666 ) ) ;
#29701 = CARTESIAN_POINT ( 'NONE',  ( 0.09601930021752928812, -0.7007513381161541988, 0.3017055919335016601 ) ) ;
#29702 = CARTESIAN_POINT ( 'NONE',  ( 0.2635877808603924177, -1.476486208343732676, 1.014510316672303514 ) ) ;
#29703 = CARTESIAN_POINT ( 'NONE',  ( 0.4388336691297091141, -1.430740155459193641, 0.8217701134134310914 ) ) ;
#29705 = CARTESIAN_POINT ( 'NONE',  ( -0.1104192559602709262, -0.5043764815743676522, 0.1033498972402041999 ) ) ;
#29704 = CARTESIAN_POINT ( 'NONE',  ( 0.1621828556419718514, -1.266751494790363086, 0.9433689391485273745 ) ) ;
#29706 = CARTESIAN_POINT ( 'NONE',  ( 0.05219137279552537451, -0.9515688809449991403, 0.3440008263018651813 ) ) ;
#29707 = ORIENTED_EDGE ( 'NONE', *, *, #26768, .F. ) ;
#29708 = ORIENTED_EDGE ( 'NONE', *, *, #27291, .T. ) ;
#29709 = AXIS2_PLACEMENT_3D ( 'NONE', #9420, #8816, #37399 ) ;
#29710 = FACE_OUTER_BOUND ( 'NONE', #5950, .T. ) ;
#29711 = CARTESIAN_POINT ( 'NONE',  ( 0.1154393097213636810, -0.4486880550576102245, 0.1802714202231547602 ) ) ;
#29712 = DIRECTION ( 'NONE',  ( -0.4999551463232372317, 0.8660512985181135770, -0.000000000000000000 ) ) ;
#29713 = VECTOR ( 'NONE', #17911, 39.37007874015748143 ) ;
#29714 = CARTESIAN_POINT ( 'NONE',  ( -0.04230258372739828521, -0.4469760454808830441, -0.1407869694282971595 ) ) ;
#29715 = CIRCLE ( 'NONE', #1493, 0.5400000000000007017 ) ;
#29716 = DIRECTION ( 'NONE',  ( 0.000000000000000000, 0.000000000000000000, -1.000000000000000000 ) ) ;
#29717 = CARTESIAN_POINT ( 'NONE',  ( 0.6136594321969363053, -1.288375518029639233, 0.6368171400845314967 ) ) ;
#29718 = CARTESIAN_POINT ( 'NONE',  ( 0.3699999999999786793, -2.097675824466503691, -0.4688691127277797022 ) ) ;
#29720 = AXIS2_PLACEMENT_3D ( 'NONE', #24723, #62, #15041 ) ;
#29719 = DIRECTION ( 'NONE',  ( 1.188678714063518227E-15, -1.000000000000000000, -3.263080277421930985E-16 ) ) ;
#29721 = CARTESIAN_POINT ( 'NONE',  ( 0.5337902897905772992, -1.637138699848535328, -0.5488759256308870516 ) ) ;
#29722 = ORIENTED_EDGE ( 'NONE', *, *, #10296, .T. ) ;
#29723 = CARTESIAN_POINT ( 'NONE',  ( 0.3702276848513395002, -1.105716412504990087, 0.7603571629394799691 ) ) ;
#29724 = CARTESIAN_POINT ( 'NONE',  ( -0.02000000000000000042, -2.049319608666233528, -0.3639547633631710633 ) ) ;
#29725 = CARTESIAN_POINT ( 'NONE',  ( -0.04085667396267326362, -0.2598928711944282766, -0.3937292009461462738 ) ) ;
#29726 = ORIENTED_EDGE ( 'NONE', *, *, #20784, .F. ) ;
#29727 = CARTESIAN_POINT ( 'NONE',  ( 0.5385803422324542122, -1.160485748998025368, 0.5861681292462268544 ) ) ;
#29728 = CARTESIAN_POINT ( 'NONE',  ( 0.1154601380735851140, -0.6757610506600419953, 0.4323217926036908021 ) ) ;
#29729 = AXIS2_PLACEMENT_3D ( 'NONE', #18855, #40229, #39836 ) ;
#29730 = CARTESIAN_POINT ( 'NONE',  ( 0.4156154940873745818, -1.130749427098165283, 0.4798916445188330382 ) ) ;
#29731 = CARTESIAN_POINT ( 'NONE',  ( 0.2502467635401044999, -1.267705161434652394, 0.6988155349366990121 ) ) ;
#29732 = EDGE_LOOP ( 'NONE', ( #25418, #23065, #4772, #26241 ) ) ;
#29733 = CARTESIAN_POINT ( 'NONE',  ( 0.05283710938261058226, 0.2421875768565610598, 0.4008269984734613711 ) ) ;
#29734 = CIRCLE ( 'NONE', #23181, 0.03999999999999930000 ) ;
#29735 = AXIS2_PLACEMENT_3D ( 'NONE', #20586, #25965, #4329 ) ;
#29736 = EDGE_CURVE ( 'NONE', #23137, #18407, #17982, .T. ) ;
#29737 = CARTESIAN_POINT ( 'NONE',  ( 0.03303737228521301528, 0.08827089426066951627, 0.5134066811673415609 ) ) ;
#29738 = CARTESIAN_POINT ( 'NONE',  ( 0.1993974397309283553, -1.367472865666984783, 0.4182417262808786895 ) ) ;
#29739 = APPROVAL ( #31338, 'UNKNOWN' ) ;
#29740 = CARTESIAN_POINT ( 'NONE',  ( -0.2399999999999999079, -3.849534981189179028, -0.1910928155360645808 ) ) ;
#29741 = CARTESIAN_POINT ( 'NONE',  ( 0.4893458284958691618, -1.274452062364263449, 0.6067319554162099449 ) ) ;
#29743 = FACE_OUTER_BOUND ( 'NONE', #26313, .T. ) ;
#29742 = LINE ( 'NONE', #19881, #14743 ) ;
#29744 = CARTESIAN_POINT ( 'NONE',  ( -0.02953079040095693900, -0.2329676531120485339, -0.4763574306556319637 ) ) ;
#29745 = ORIENTED_EDGE ( 'NONE', *, *, #39296, .F. ) ;
#29746 = CARTESIAN_POINT ( 'NONE',  ( 0.07216878364870175921, 0.05141091571461216952, -0.1249999999999971689 ) ) ;
#29747 = VERTEX_POINT ( 'NONE', #9608 ) ;
#29748 = FACE_OUTER_BOUND ( 'NONE', #38640, .T. ) ;
#29749 = CARTESIAN_POINT ( 'NONE',  ( 0.1689459712188738916, -0.9783659983241776992, 0.7869633328443620401 ) ) ;
#29750 = AXIS2_PLACEMENT_3D ( 'NONE', #38211, #28948, #35520 ) ;
#29752 = CARTESIAN_POINT ( 'NONE',  ( 0.1920071873703447507, -0.8110264159798786787, 0.2735051980380696635 ) ) ;
#29751 = CARTESIAN_POINT ( 'NONE',  ( 0.08874571000602692050, -0.6053243709266833417, 0.05379243744558167423 ) ) ;
#29753 = CARTESIAN_POINT ( 'NONE',  ( 0.1424029337235096226, -1.400533250147911746, -0.6250000000000000000 ) ) ;
#29754 = ORIENTED_EDGE ( 'NONE', *, *, #38600, .T. ) ;
#29755 = ORIENTED_EDGE ( 'NONE', *, *, #37405, .T. ) ;
#29756 = PLANE ( 'NONE',  #5037 ) ;
#29757 = CARTESIAN_POINT ( 'NONE',  ( 0.5566577208962448786, -1.469770625181828549, 0.7214895520387809569 ) ) ;
#29758 = ORIENTED_EDGE ( 'NONE', *, *, #38360, .F. ) ;
#29759 = CARTESIAN_POINT ( 'NONE',  ( 0.6091898566437330409, -1.605611940169644258, 0.5996532284048697869 ) ) ;
#29760 = CARTESIAN_POINT ( 'NONE',  ( 0.04230170315643919099, -0.4483301424763386223, 0.1366247710447600627 ) ) ;
#29761 = ADVANCED_FACE ( 'NONE', ( #25034 ), #24656, .T. ) ;
#29762 = CARTESIAN_POINT ( 'NONE',  ( 0.3756960969702827779, -1.762375030584327984, -0.4374392251508507079 ) ) ;
#29763 = CARTESIAN_POINT ( 'NONE',  ( 0.1761881424425499609, -1.253808687867943084, 0.4381683186903178040 ) ) ;
#29764 = AXIS2_PLACEMENT_3D ( 'NONE', #28619, #22258, #5972 ) ;
#29765 = LINE ( 'NONE', #20122, #37120 ) ;
#29766 = DIRECTION ( 'NONE',  ( 1.000000000000000000, 2.280301054154495132E-31, -1.664003471950577689E-31 ) ) ;
#29767 = ADVANCED_FACE ( 'NONE', ( #15376 ), #16706, .T. ) ;
#29768 = CARTESIAN_POINT ( 'NONE',  ( 0.1907823988372855106, -0.4944553380418882926, 0.2959634315342150046 ) ) ;
#29769 = EDGE_CURVE ( 'NONE', #9616, #6871, #21970, .T. ) ;
#29770 = CIRCLE ( 'NONE', #12036, 0.04500000000000022038 ) ;
#29771 = CONICAL_SURFACE ( 'NONE', #39594, 0.07506498716826678907, 1.103346454748738825 ) ;
#29772 = CARTESIAN_POINT ( 'NONE',  ( -0.1710642718812830643, 0.4986889572247755198, 0.3032895567580806695 ) ) ;
#29773 = DIRECTION ( 'NONE',  ( -2.563099466555618830E-12, -0.9510565162951529761, 0.3090169943749491166 ) ) ;
#29774 = EDGE_CURVE ( 'NONE', #10935, #31618, #10609, .T. ) ;
#29775 = EDGE_CURVE ( 'NONE', #35263, #20307, #4209, .T. ) ;
#29776 = CARTESIAN_POINT ( 'NONE',  ( 0.6050535996821563289, -1.589783510039989967, -0.5530470261699707013 ) ) ;
#29777 = CARTESIAN_POINT ( 'NONE',  ( 0.04157078424165463332, 0.2624491172974852682, 0.3902147976630855331 ) ) ;
#29778 = CARTESIAN_POINT ( 'NONE',  ( 0.1836329606266136616, -0.5161036956692948152, 0.07857586674746268318 ) ) ;
#29779 = ADVANCED_FACE ( 'NONE', ( #38183 ), #409, .T. ) ;
#29780 = CARTESIAN_POINT ( 'NONE',  ( 0.5977626385027750011, -1.597637465087648811, 0.4278768775546197278 ) ) ;
#29781 = AXIS2_PLACEMENT_3D ( 'NONE', #3771, #23924, #1727 ) ;
#29782 = CARTESIAN_POINT ( 'NONE',  ( 0.1429229523316038197, -1.294172713379485584, 0.4193902271515088098 ) ) ;
#29783 = CARTESIAN_POINT ( 'NONE',  ( 0.000000000000000000, -0.4262518876079541830, 0.1457185332388682419 ) ) ;
#29784 = CARTESIAN_POINT ( 'NONE',  ( 0.6144487089066268393, -1.489086973007883730, -0.6152890497467740083 ) ) ;
#29785 = CARTESIAN_POINT ( 'NONE',  ( -1.019575837292303166, -0.04310840302197994911, 0.3749999999999990008 ) ) ;
#29786 = CARTESIAN_POINT ( 'NONE',  ( 0.3048024544079886988, -1.756867927854032674, 0.5684537085834007186 ) ) ;
#29787 = CARTESIAN_POINT ( 'NONE',  ( -0.04230258372739723050, -0.2720195588163292211, 0.3815939145425439327 ) ) ;
#29788 = ORIENTED_EDGE ( 'NONE', *, *, #40311, .F. ) ;
#29789 = EDGE_LOOP ( 'NONE', ( #29726, #36153, #13181, #23292 ) ) ;
#29790 = CARTESIAN_POINT ( 'NONE',  ( -0.2399999999999999079, -3.745280840418592661, 0.04438736989695814261 ) ) ;
#29791 =( BOUNDED_SURFACE ( )  B_SPLINE_SURFACE ( 3, 2, ( 
 ( #15520, #12230, #21688 ),
 ( #34218, #6033, #40602 ),
 ( #12420, #24968, #37500 ),
 ( #9325, #21904, #26013 ),
 ( #26202, #727, #16331 ),
 ( #29285, #6844, #10764 ) ),
 .UNSPECIFIED., .F., .F., .T. ) 
 B_SPLINE_SURFACE_WITH_KNOTS ( ( 4, 2, 4 ),
 ( 3, 3 ),
 ( 3.120333852413281761E-16, 0.0003231562290647264500, 0.0006463124581291408667 ),
 ( 0.000000000000000000, 1.000000000000000000 ),
 .UNSPECIFIED. ) 
 GEOMETRIC_REPRESENTATION_ITEM ( )  RATIONAL_B_SPLINE_SURFACE ( (
 ( 1.000000000000000000, 0.8997265729123280487, 1.000000000000000000),
 ( 1.000000000000000000, 0.9023522654549963606, 1.000000000000000000),
 ( 1.000000000000000000, 0.9048744759709612673, 1.000000000000000000),
 ( 1.000000000000000000, 0.9100851747552831661, 1.000000000000000000),
 ( 1.000000000000000000, 0.9127760422757066339, 1.000000000000000000),
 ( 1.000000000000000000, 0.9157534740967101516, 1.000000000000000000) ) ) 
 REPRESENTATION_ITEM ( '' )  SURFACE ( )  );
#29792 = EDGE_CURVE ( 'NONE', #8811, #3931, #19488, .T. ) ;
#29793 = CARTESIAN_POINT ( 'NONE',  ( 0.3711231209398546671, -1.768532844275155780, -0.5764367090175167574 ) ) ;
#29794 = VERTEX_POINT ( 'NONE', #7518 ) ;
#29795 = LINE ( 'NONE', #29586, #38162 ) ;
#29796 = CARTESIAN_POINT ( 'NONE',  ( 0.02872242845530435101, 0.2464193076120115011, -0.4721747535844857957 ) ) ;
#29797 = CONICAL_SURFACE ( 'NONE', #10095, 0.1400000000000007350, 1.047197551196601184 ) ;
#29798 = CARTESIAN_POINT ( 'NONE',  ( 0.4933479471158314644, -1.287949358479272055, 0.7760119179218301078 ) ) ;
#29800 = ORIENTED_EDGE ( 'NONE', *, *, #25521, .T. ) ;
#29799 = CARTESIAN_POINT ( 'NONE',  ( -0.2399999999999999079, -2.409101312171279208, -0.6551853038253486750 ) ) ;
#29801 = CARTESIAN_POINT ( 'NONE',  ( 0.5179624304041525740, -1.133452979592703302, 0.6716967517830890744 ) ) ;
#29802 = CARTESIAN_POINT ( 'NONE',  ( 0.05283710938261075574, 0.4560492058803797266, -0.1064717188025600253 ) ) ;
#29803 = ORIENTED_EDGE ( 'NONE', *, *, #14401, .F. ) ;
#29804 = B_SPLINE_CURVE_WITH_KNOTS ( 'NONE', 3,
 ( #14635, #24135, #11355, #36657 ),
 .UNSPECIFIED., .F., .F.,
 ( 4, 4 ),
 ( 8.673617379884035472E-19, 0.0003185022396561879823 ),
 .UNSPECIFIED. ) ;
#29805 = CARTESIAN_POINT ( 'NONE',  ( 0.3238143371732789544, -1.179505499532595758, 0.5655564271612124605 ) ) ;
#29806 = ORIENTED_EDGE ( 'NONE', *, *, #15186, .T. ) ;
#29807 = CIRCLE ( 'NONE', #37670, 0.3698489655878011706 ) ;
#29808 = CARTESIAN_POINT ( 'NONE',  ( 0.05169272155612220088, -0.7052237289551500643, 0.5425721195289684440 ) ) ;
#29810 = CARTESIAN_POINT ( 'NONE',  ( -0.03868264068766654601, -0.3066108573455318953, 0.3648330973802367261 ) ) ;
#29809 = CARTESIAN_POINT ( 'NONE',  ( 0.6849528713309417371, -1.506609029741341255, 0.4574981245801082452 ) ) ;
#29811 = CARTESIAN_POINT ( 'NONE',  ( 0.2321526281619643584, -1.233007205928619232, 0.3667417262808778111 ) ) ;
#29812 = CARTESIAN_POINT ( 'NONE',  ( 0.1734973056165642902, -1.209394307038482497, -0.5155029497116575543 ) ) ;
#29813 = ORIENTED_EDGE ( 'NONE', *, *, #975, .F. ) ;
#29814 = EDGE_CURVE ( 'NONE', #20188, #38276, #32429, .T. ) ;
#29815 = DIRECTION ( 'NONE',  ( -1.000000000000000000, -0.000000000000000000, -0.000000000000000000 ) ) ;
#29816 = AXIS2_PLACEMENT_3D ( 'NONE', #4866, #1036, #39433 ) ;
#29817 = EDGE_CURVE ( 'NONE', #38249, #30555, #18477, .T. ) ;
#29818 = CARTESIAN_POINT ( 'NONE',  ( -0.1167294259372883281, -0.5331983348239501819, 0.3032895567580801144 ) ) ;
#29819 = CARTESIAN_POINT ( 'NONE',  ( -0.02000000000000000042, -2.070343076906777213, -0.2454056712452573896 ) ) ;
#29820 = AXIS2_PLACEMENT_3D ( 'NONE', #18617, #31175, #15540 ) ;
#29821 = CARTESIAN_POINT ( 'NONE',  ( 0.4181182131315021033, -1.203184156692840734, 0.6707339718938493123 ) ) ;
#29822 = FACE_OUTER_BOUND ( 'NONE', #27436, .T. ) ;
#29823 = CARTESIAN_POINT ( 'NONE',  ( -0.1684323895665172655, 0.5231977504176978933, 0.3102582297535276257 ) ) ;
#29824 = CARTESIAN_POINT ( 'NONE',  ( 0.1957369265267845937, -0.9763688040310566363, 0.5238895912861436521 ) ) ;
#29825 = EDGE_CURVE ( 'NONE', #34037, #40101, #39684, .T. ) ;
#29826 = LINE ( 'NONE', #38862, #14070 ) ;
#29827 = CARTESIAN_POINT ( 'NONE',  ( 0.05634301242525737580, 0.4332457820339863930, 0.1515812001271573117 ) ) ;
#29828 = DIRECTION ( 'NONE',  ( 0.4999551463232373427, -0.8660512985181134660, 0.000000000000000000 ) ) ;
#29829 = CARTESIAN_POINT ( 'NONE',  ( -0.01999999999999990674, -3.186969272371774853, -0.6488225763796510170 ) ) ;
#29830 = AXIS2_PLACEMENT_3D ( 'NONE', #2232, #1837, #27526 ) ;
#29831 = EDGE_CURVE ( 'NONE', #25265, #29236, #35679, .T. ) ;
#29832 = CARTESIAN_POINT ( 'NONE',  ( 0.3683757878646363726, -1.156357368468860392, 0.4257332135735479861 ) ) ;
#29833 = EDGE_CURVE ( 'NONE', #19999, #1199, #31820, .T. ) ;
#29834 = FACE_OUTER_BOUND ( 'NONE', #13988, .T. ) ;
#29835 = DIRECTION ( 'NONE',  ( -7.771561172376107616E-16, 7.170354002788761615E-17, -1.000000000000000000 ) ) ;
#29836 = CONICAL_SURFACE ( 'NONE', #12100, 0.1600000000000006140, 1.047197551196598075 ) ;
#29837 = CARTESIAN_POINT ( 'NONE',  ( 0.0002547247918985094499, -0.4980400414177595381, -0.01674915368249139946 ) ) ;
#29838 = CARTESIAN_POINT ( 'NONE',  ( 4.898587196589415849E-18, -0.4700000000000001954, -0.04000000000000001471 ) ) ;
#29839 = CARTESIAN_POINT ( 'NONE',  ( -0.1210148435730253880, -0.5061394519557965710, 0.3122829191278980177 ) ) ;
#29840 = DIRECTION ( 'NONE',  ( 0.9378410757839554801, -0.2807814858886596432, -0.2039996905746410405 ) ) ;
#29841 = AXIS2_PLACEMENT_3D ( 'NONE', #15950, #9576, #28104 ) ;
#29842 = EDGE_LOOP ( 'NONE', ( #22297, #38341, #39252, #20165 ) ) ;
#29843 = EDGE_LOOP ( 'NONE', ( #24211, #16533, #23720, #25001 ) ) ;
#29844 = AXIS2_PLACEMENT_3D ( 'NONE', #14374, #16669, #35583 ) ;
#29845 = ADVANCED_FACE ( 'NONE', ( #26262 ), #37991, .T. ) ;
#29846 = CARTESIAN_POINT ( 'NONE',  ( 1.422893940835647384E-17, 0.08000000000000023759, 0.08769881541126035851 ) ) ;
#29847 = VERTEX_POINT ( 'NONE', #16589 ) ;
#29848 = CARTESIAN_POINT ( 'NONE',  ( 0.4738546087217680447, -1.652018268363229181, -0.3975985852014398136 ) ) ;
#29849 = CARTESIAN_POINT ( 'NONE',  ( 0.6026051337862934343, -1.481309381409939618, 0.6176392787056765865 ) ) ;
#29851 = ORIENTED_EDGE ( 'NONE', *, *, #30439, .T. ) ;
#29850 = CARTESIAN_POINT ( 'NONE',  ( 0.007764572479489010963, -0.7391071013572128034, -0.003941584134019470581 ) ) ;
#29852 = EDGE_CURVE ( 'NONE', #23080, #199, #38384, .T. ) ;
#29853 = EDGE_LOOP ( 'NONE', ( #27186, #14152, #25831, #18661 ) ) ;
#29854 = CARTESIAN_POINT ( 'NONE',  ( 0.3140415829244854184, -1.186180626463321230, 0.4809987123389981578 ) ) ;
#29855 = ORIENTED_EDGE ( 'NONE', *, *, #18217, .F. ) ;
#29856 = CARTESIAN_POINT ( 'NONE',  ( 0.2530344669440779404, -1.593468256218861567, 0.8522446305581886650 ) ) ;
#29858 = CARTESIAN_POINT ( 'NONE',  ( 0.2128381955336136888, -1.241281127606408186, 0.5854230766145357423 ) ) ;
#29857 = CARTESIAN_POINT ( 'NONE',  ( 0.5922106362852195272, -1.600826850851058802, 0.4254268223615397804 ) ) ;
#29859 = DIRECTION ( 'NONE',  ( 0.000000000000000000, 3.330669073875470114E-16, 1.000000000000000000 ) ) ;
#29860 = DATE_AND_TIME ( #38509, #26740 ) ;
#29861 = AXIS2_PLACEMENT_3D ( 'NONE', #36683, #8489, #21050 ) ;
#29862 = CARTESIAN_POINT ( 'NONE',  ( 0.08978098643734212791, 1.231844511688112729E-16, 0.3698489655877988391 ) ) ;
#29864 = EDGE_LOOP ( 'NONE', ( #11443, #2743, #38441, #27057, #13747 ) ) ;
#29863 = ORIENTED_EDGE ( 'NONE', *, *, #10636, .F. ) ;
#29865 = CARTESIAN_POINT ( 'NONE',  ( 0.1376160882066851110, -0.8423595946558073422, 0.4896585138266671966 ) ) ;
#29866 = EDGE_CURVE ( 'NONE', #12338, #28931, #27863, .T. ) ;
#29867 = CARTESIAN_POINT ( 'NONE',  ( 0.1119881974088350329, -1.370995722074662693, 0.6752038603878468548 ) ) ;
#29868 = TOROIDAL_SURFACE ( 'NONE', #33829, 0.04749999999977554815, 0.01000000000000000021 ) ;
#29869 = CARTESIAN_POINT ( 'NONE',  ( 0.09245771922927559228, -0.6466466848293074277, 0.4347549917907825856 ) ) ;
#29870 = TOROIDAL_SURFACE ( 'NONE', #22016, 0.05330708661417323663, 0.01000000000000000021 ) ;
#29871 = CARTESIAN_POINT ( 'NONE',  ( 0.5539269415344313385, -1.511025941422516006, 0.5935205164291307289 ) ) ;
#29872 = CARTESIAN_POINT ( 'NONE',  ( 0.06498580141003787447, -1.293606482245585498, 0.6256161605704260165 ) ) ;
#29873 = FACE_OUTER_BOUND ( 'NONE', #31322, .T. ) ;
#29874 = APPROVAL_PERSON_ORGANIZATION ( #28672, #408, #23715 ) ;
#29875 = DIRECTION ( 'NONE',  ( 1.000000000000000000, 0.000000000000000000, 0.000000000000000000 ) ) ;
#29876 = CARTESIAN_POINT ( 'NONE',  ( 0.4134438183949054602, -1.708815802511751025, -0.4210476217684242517 ) ) ;
#29877 = CARTESIAN_POINT ( 'NONE',  ( 0.3827496839977685417, -1.607288045992097070, -0.3194649185273498171 ) ) ;
#29878 = VECTOR ( 'NONE', #7838, 39.37007874015748143 ) ;
#29879 = CARTESIAN_POINT ( 'NONE',  ( -0.2746410161513776482, -3.838583118162426810, -0.3058907208964237734 ) ) ;
#29880 = CARTESIAN_POINT ( 'NONE',  ( -0.01548846960721245516, -0.3688619771570368910, -0.3775276577325204497 ) ) ;
#29881 = CARTESIAN_POINT ( 'NONE',  ( 0.000000000000000000, -0.2276394436010286959, -0.1339480508475833498 ) ) ;
#29882 = CARTESIAN_POINT ( 'NONE',  ( 0.01164198743023061450, -0.7796407181604130265, -0.09629102463154327884 ) ) ;
#29883 = CARTESIAN_POINT ( 'NONE',  ( 0.3656015928468621112, -1.617944161404246906, -0.4193447143115660025 ) ) ;
#29884 =( LENGTH_UNIT ( ) NAMED_UNIT ( * ) SI_UNIT ( $, .METRE. ) );
#29885 = ADVANCED_FACE ( 'NONE', ( #32019 ), #19361, .T. ) ;
#29886 = CARTESIAN_POINT ( 'NONE',  ( 0.007773584319307426035, -0.7382159792943179255, -0.004238343198677651906 ) ) ;
#29887 = CARTESIAN_POINT ( 'NONE',  ( 0.6215918093157997149, -1.606820104549159245, -0.5669819737327814746 ) ) ;
#29888 = CARTESIAN_POINT ( 'NONE',  ( 0.1623712441042921006, -1.412506991498796660, 0.8192480828659791658 ) ) ;
#29889 = CARTESIAN_POINT ( 'NONE',  ( 0.1874346505856443745, -0.8710952576279675785, 0.2160754816401605771 ) ) ;
#29890 = SECURITY_CLASSIFICATION_LEVEL ( 'unclassified' ) ;
#29891 = CARTESIAN_POINT ( 'NONE',  ( 0.5453389350593388363, -1.184144166247469876, 0.8773366473911075047 ) ) ;
#29892 = CIRCLE ( 'NONE', #2294, 0.06173076923076910999 ) ;
#29893 = CIRCLE ( 'NONE', #6881, 0.1500000000000009936 ) ;
#29894 = CARTESIAN_POINT ( 'NONE',  ( 0.4126538731429406082, -1.611929415335916271, -0.6681135029249770652 ) ) ;
#29895 = CARTESIAN_POINT ( 'NONE',  ( 0.3136311368843414105, -1.762219552882195783, 0.5683051179383220575 ) ) ;
#29896 = EDGE_LOOP ( 'NONE', ( #2326, #22521, #21537, #26828 ) ) ;
#29897 = CARTESIAN_POINT ( 'NONE',  ( 0.3463972363130231047, -1.700516749477267053, -0.5547452799823860969 ) ) ;
#29898 = LOCAL_TIME ( 0, 53, 7.000000000000000000, #31649 ) ;
#29899 = CARTESIAN_POINT ( 'NONE',  ( 0.1378941890947338045, -1.196521231248368844, 0.9199180204847504649 ) ) ;
#29900 = EDGE_CURVE ( 'NONE', #37623, #2187, #18999, .T. ) ;
#29901 = CARTESIAN_POINT ( 'NONE',  ( 0.08058916068514494768, -1.309220013881624123, 0.4727703015479320370 ) ) ;
#29903 = VERTEX_POINT ( 'NONE', #38998 ) ;
#29902 = CARTESIAN_POINT ( 'NONE',  ( 0.2813047422443414325, -1.204938683099350705, 0.5682417262808779901 ) ) ;
#29904 = EDGE_CURVE ( 'NONE', #14594, #14778, #23270, .T. ) ;
#29905 = DIRECTION ( 'NONE',  ( 1.571558834619978106E-31, 0.9849933812516250553, 0.1725921171157334399 ) ) ;
#29906 = AXIS2_PLACEMENT_3D ( 'NONE', #39521, #37054, #23710 ) ;
#29907 = CARTESIAN_POINT ( 'NONE',  ( 0.2196261443710258443, -0.6607888217372858142, 0.4354189310569229754 ) ) ;
#29909 = VERTEX_POINT ( 'NONE', #17605 ) ;
#29908 = ORIENTED_EDGE ( 'NONE', *, *, #10242, .F. ) ;
#29910 = CARTESIAN_POINT ( 'NONE',  ( 0.04917380528055519118, -1.483446811033737989, -0.6748800710299313055 ) ) ;
#29911 = CARTESIAN_POINT ( 'NONE',  ( 0.3545247821006056732, -1.838528400036530064, -0.5140887209270352809 ) ) ;
#29912 = CARTESIAN_POINT ( 'NONE',  ( -0.1795773455677817376, 0.4580325878418074481, 0.09550516381870181870 ) ) ;
#29913 = DATE_AND_TIME ( #4781, #14182 ) ;
#29914 = CARTESIAN_POINT ( 'NONE',  ( -0.01899468245560449395, 0.5123206680798557677, -0.08888613072388730496 ) ) ;
#29915 = ORIENTED_EDGE ( 'NONE', *, *, #16057, .T. ) ;
#29916 = CARTESIAN_POINT ( 'NONE',  ( 0.1170761419057074482, -1.261392965458049131, 0.6036835557974136179 ) ) ;
#29917 = CARTESIAN_POINT ( 'NONE',  ( 0.2584190914277442186, -0.9487391774685208778, 0.7036860948817510453 ) ) ;
#29918 = CARTESIAN_POINT ( 'NONE',  ( 0.2995624311403809470, -1.612171325865530136, 0.9470918590109783652 ) ) ;
#29919 = CARTESIAN_POINT ( 'NONE',  ( 0.09887370392402621000, -0.5650284097326406796, 0.2392820984072531743 ) ) ;
#29921 = LINE ( 'NONE', #1763, #18300 ) ;
#29920 = CARTESIAN_POINT ( 'NONE',  ( -0.1399999999999997358, -3.326417233800878524E-17, -0.1250000000000000000 ) ) ;
#29922 = CARTESIAN_POINT ( 'NONE',  ( 0.2792289373433416988, -1.051500623829179526, 0.6297070940450347765 ) ) ;
#29923 = VERTEX_POINT ( 'NONE', #4617 ) ;
#29924 = ORIENTED_EDGE ( 'NONE', *, *, #28289, .F. ) ;
#29925 = CONICAL_SURFACE ( 'NONE', #12179, 0.01999999999999924061, 1.047197551196600962 ) ;
#29926 = CARTESIAN_POINT ( 'NONE',  ( 0.05283710938261045043, -0.4315340639268043232, -0.1819215676045972951 ) ) ;
#29927 = CONICAL_SURFACE ( 'NONE', #35186, 0.1020173459747799466, 1.047197551196601184 ) ;
#29928 = CARTESIAN_POINT ( 'NONE',  ( 0.2407639156934034685, -0.6284568509811103709, 0.5445959906753944368 ) ) ;
#29929 = AXIS2_PLACEMENT_3D ( 'NONE', #17819, #14949, #40232 ) ;
#29930 = CARTESIAN_POINT ( 'NONE',  ( -0.2746410161513770931, -2.945416957892569521, -0.4639726661791638840 ) ) ;
#29931 = APPROVAL_PERSON_ORGANIZATION ( #24364, #22019, #34214 ) ;
#29932 = CARTESIAN_POINT ( 'NONE',  ( -0.04211812644076706746, -0.4486350089847107592, -0.1367863764325146780 ) ) ;
#29933 = EDGE_CURVE ( 'NONE', #39260, #29582, #19963, .T. ) ;
#29934 = ADVANCED_FACE ( 'NONE', ( #29536 ), #30150, .F. ) ;
#29935 = CARTESIAN_POINT ( 'NONE',  ( 0.1909286924077255587, -1.257064795538239022, -0.6485234391946320676 ) ) ;
#29936 = CARTESIAN_POINT ( 'NONE',  ( 0.3944112475498172676, -1.768123242797767558, -0.4830133339744027698 ) ) ;
#29937 = VECTOR ( 'NONE', #3114, 39.37007874015748143 ) ;
#29938 = CARTESIAN_POINT ( 'NONE',  ( 0.000000000000000000, 0.000000000000000000, 0.000000000000000000 ) ) ;
#29939 = CARTESIAN_POINT ( 'NONE',  ( 0.5804192421706322325, -1.234356152197840117, 0.7108377039426548860 ) ) ;
#29940 = DIRECTION ( 'NONE',  ( 0.3468893892380647270, -0.9373665302208729067, 0.03180785525186742568 ) ) ;
#29941 = CARTESIAN_POINT ( 'NONE',  ( 0.1684145848869400830, -1.308153301062764395, -0.3047563416178276641 ) ) ;
#29942 = CARTESIAN_POINT ( 'NONE',  ( 0.5391011117901446381, -1.666771999651815106, -0.5698732322495047020 ) ) ;
#29943 = ORIENTED_EDGE ( 'NONE', *, *, #37295, .F. ) ;
#29944 = FACE_OUTER_BOUND ( 'NONE', #186, .T. ) ;
#29945 = FACE_OUTER_BOUND ( 'NONE', #28753, .T. ) ;
#29946 = CARTESIAN_POINT ( 'NONE',  ( -0.05544444631433736309, -0.2873070878496327141, -0.3609075552494494521 ) ) ;
#29947 = ORIENTED_EDGE ( 'NONE', *, *, #26156, .T. ) ;
#29948 = CARTESIAN_POINT ( 'NONE',  ( 0.4365432303899622890, -1.033643997532201597, 0.7173331770504315363 ) ) ;
#29949 = CARTESIAN_POINT ( 'NONE',  ( 0.5373165049569139651, -1.161628669640105027, 0.5421417554447620635 ) ) ;
#29950 = CARTESIAN_POINT ( 'NONE',  ( 0.3416191607863283686, -1.126820519681605903, 0.5182417262812423209 ) ) ;
#29951 = AXIS2_PLACEMENT_3D ( 'NONE', #36311, #8132, #38783 ) ;
#29952 = CIRCLE ( 'NONE', #28662, 0.2500000000000000000 ) ;
#29953 = CARTESIAN_POINT ( 'NONE',  ( 0.05733805304787521762, -0.8395800731581377629, 0.2495454520759651795 ) ) ;
#29954 = ORIENTED_EDGE ( 'NONE', *, *, #33881, .T. ) ;
#29955 = CARTESIAN_POINT ( 'NONE',  ( 0.05634301242525759784, 0.2614060064472222833, 0.3772872482281158790 ) ) ;
#29956 = CARTESIAN_POINT ( 'NONE',  ( 0.1825980849618502877, -1.261391773294454399, 0.5182417262812422099 ) ) ;
#29957 = APPLIED_SECURITY_CLASSIFICATION_ASSIGNMENT ( #2357, ( #24016 ) ) ;
#29958 = CARTESIAN_POINT ( 'NONE',  ( 0.1402147235662943858, -1.401774878535922975, 0.4497410000889012216 ) ) ;
#29959 = CARTESIAN_POINT ( 'NONE',  ( 0.1968260301802208789, -2.003704694174034628, -0.2869878483811844072 ) ) ;
#29960 = CARTESIAN_POINT ( 'NONE',  ( 0.3900475047517206195, -1.136049760834360711, 0.7018806097820817769 ) ) ;
#29961 = ADVANCED_FACE ( 'NONE', ( #36720 ), #5437, .T. ) ;
#29963 = CARTESIAN_POINT ( 'NONE',  ( 0.3565880379454448579, -1.898203685287057629, -0.4912697616745712592 ) ) ;
#29962 = CARTESIAN_POINT ( 'NONE',  ( 0.4138729472876766513, -1.128955312352843965, 0.5470489658417444501 ) ) ;
#29964 = CARTESIAN_POINT ( 'NONE',  ( 0.2225775331702970761, -0.9343733720331020010, 0.4090965549137709489 ) ) ;
#29965 = ORIENTED_EDGE ( 'NONE', *, *, #19742, .T. ) ;
#29966 = VECTOR ( 'NONE', #15406, 39.37007874015748854 ) ;
#29967 = DIRECTION ( 'NONE',  ( -1.188678714063518227E-15, 1.000000000000000000, 3.263080277421930985E-16 ) ) ;
#29968 = ORIENTED_EDGE ( 'NONE', *, *, #39716, .F. ) ;
#29969 = LINE ( 'NONE', #23799, #21357 ) ;
#29970 = CARTESIAN_POINT ( 'NONE',  ( 0.1087658859722912819, -0.7576187927048527726, 0.5953713316029712876 ) ) ;
#29972 = DIRECTION ( 'NONE',  ( 1.000000000000000000, 2.280301054154495132E-31, -1.664003471950577689E-31 ) ) ;
#29971 = CARTESIAN_POINT ( 'NONE',  ( 0.08964876120596533549, -0.5474965510609541841, 0.1111581565464928867 ) ) ;
#29973 = CARTESIAN_POINT ( 'NONE',  ( 0.2469141422421070875, -1.581573626495411444, -0.3511777555542848206 ) ) ;
#29974 = ORIENTED_EDGE ( 'NONE', *, *, #887, .F. ) ;
#29975 = CARTESIAN_POINT ( 'NONE',  ( 0.2614468074032732514, -0.7584085742687330933, 0.1932256475537141860 ) ) ;
#29976 = CARTESIAN_POINT ( 'NONE',  ( 0.1193505310152234433, -0.5488392675763952289, 0.1535339596633792936 ) ) ;
#29977 = EDGE_LOOP ( 'NONE', ( #8888, #12626, #33131, #36258 ) ) ;
#29978 = CARTESIAN_POINT ( 'NONE',  ( -0.2746410161513779258, -2.154189217240303655, -0.3012881438978375903 ) ) ;
#29979 = CARTESIAN_POINT ( 'NONE',  ( 0.04308611741967688369, -0.4845711164929068504, 0.09763251765260519410 ) ) ;
#29980 = CARTESIAN_POINT ( 'NONE',  ( 0.6095536282444361520, -1.587373553213482280, 0.4182417262808777458 ) ) ;
#29981 = CARTESIAN_POINT ( 'NONE',  ( 0.1094588636161752809, -1.304004861155783068, 0.4319985379268259096 ) ) ;
#29982 = CARTESIAN_POINT ( 'NONE',  ( 0.3955374044963104740, -1.750921016457922086, -0.4909020773731604392 ) ) ;
#29983 = CARTESIAN_POINT ( 'NONE',  ( -0.02000000000000000042, -1.772778095317936620, -0.3120197613628934441 ) ) ;
#29984 = AXIS2_PLACEMENT_3D ( 'NONE', #21385, #2840, #5720 ) ;
#29985 = CARTESIAN_POINT ( 'NONE',  ( 0.2723301224276278298, -0.7044396210649886969, 0.6356112240561296867 ) ) ;
#29986 = CARTESIAN_POINT ( 'NONE',  ( -0.01548846960707416127, 0.2450655194479873511, 0.4674710490749285352 ) ) ;
#29987 = PLANE ( 'NONE',  #11359 ) ;
#29988 = ORGANIZATION ( 'NAUO-ORG3', 'UNSPECIFIED', 'UNSPECIFIED' ) ;
#29989 = CARTESIAN_POINT ( 'NONE',  ( 0.6201936192677818260, -1.619527673991476124, -0.4829864890893342255 ) ) ;
#29990 = DIRECTION ( 'NONE',  ( 5.551115123125788865E-17, -3.676620095425087714E-16, -1.000000000000000000 ) ) ;
#29991 = CARTESIAN_POINT ( 'NONE',  ( 0.6521596339623016991, -1.579655379295860307, 0.6112030275387951850 ) ) ;
#29992 = CARTESIAN_POINT ( 'NONE',  ( 0.3975363061031572665, -1.737107943197741866, -0.4349671603868599523 ) ) ;
#29993 = CARTESIAN_POINT ( 'NONE',  ( -0.05283710938261126921, 0.4315340639268049339, -0.1819215676045952412 ) ) ;
#29994 = CARTESIAN_POINT ( 'NONE',  ( 0.01197363197122058853, -0.5805133742323803636, 0.4689902101802463363 ) ) ;
#29995 = CARTESIAN_POINT ( 'NONE',  ( 0.5934855389617087473, -1.553883175902015967, -0.4613003755920050408 ) ) ;
#29996 = CARTESIAN_POINT ( 'NONE',  ( 0.2923286432308245808, -1.660243258845594649, -0.3370932271639339728 ) ) ;
#29997 = CARTESIAN_POINT ( 'NONE',  ( -0.01736481776669303659, -0.8497080691189130564, 0.1457185332388703236 ) ) ;
#29998 = CARTESIAN_POINT ( 'NONE',  ( -0.05634490452572801095, -0.2656249956367415233, 0.3742168499392072301 ) ) ;
#29999 = ORIENTED_EDGE ( 'NONE', *, *, #36038, .T. ) ;
#30000 = VERTEX_POINT ( 'NONE', #7729 ) ;
#30001 = FACE_OUTER_BOUND ( 'NONE', #14892, .T. ) ;
#30002 = EDGE_LOOP ( 'NONE', ( #22128, #25986 ) ) ;
#30003 = DIRECTION ( 'NONE',  ( 0.9998941247116546194, -0.01455087607601020412, 0.0001066420868422379633 ) ) ;
#30004 = CYLINDRICAL_SURFACE ( 'NONE', #12733, 0.08000000000000000167 ) ;
#30005 = CARTESIAN_POINT ( 'NONE',  ( 0.3954536428817021498, -1.141798559182092943, 0.7526865122305215206 ) ) ;
#30007 = ORIENTED_EDGE ( 'NONE', *, *, #3504, .T. ) ;
#30006 = CARTESIAN_POINT ( 'NONE',  ( -0.1623906354757041204, 0.5045448597005471880, 0.1308137833173686204 ) ) ;
#30008 = CARTESIAN_POINT ( 'NONE',  ( 0.5138184642618360831, -1.118801421376873551, 0.5693865086028936373 ) ) ;
#30009 = CIRCLE ( 'NONE', #16217, 0.2000000000000000111 ) ;
#30010 = EDGE_CURVE ( 'NONE', #12964, #4682, #20643, .T. ) ;
#30011 = CARTESIAN_POINT ( 'NONE',  ( -1.974223891136790438E-05, -2.025566271751752634, -0.3135830156841454830 ) ) ;
#30012 = ORIENTED_EDGE ( 'NONE', *, *, #10188, .T. ) ;
#30013 = CARTESIAN_POINT ( 'NONE',  ( 0.4671438810788549056, -1.683830466669562709, -0.4131679330247047255 ) ) ;
#30014 = ADVANCED_FACE ( 'NONE', ( #26461 ), #36109, .T. ) ;
#30015 = ORIENTED_EDGE ( 'NONE', *, *, #29594, .T. ) ;
#30016 = CARTESIAN_POINT ( 'NONE',  ( 0.3304196671140066099, -1.628641716510011994, 0.7020376695473490303 ) ) ;
#30018 = CARTESIAN_POINT ( 'NONE',  ( 0.1145437834104099661, -0.4941296012437448870, 0.001010760634015512704 ) ) ;
#30017 = CARTESIAN_POINT ( 'NONE',  ( 0.7060640942175693269, -1.498641769205614205, 0.5270363939079757420 ) ) ;
#30019 = CARTESIAN_POINT ( 'NONE',  ( 0.1434010736994648927, -1.283284918233685623, 0.5707417262808780478 ) ) ;
#30020 = SECURITY_CLASSIFICATION ( '', '', #17899 ) ;
#30021 = ADVANCED_FACE ( 'NONE', ( #23786 ), #17375, .F. ) ;
#30022 = FACE_OUTER_BOUND ( 'NONE', #34140, .T. ) ;
#30023 = EDGE_LOOP ( 'NONE', ( #12625, #13416, #5294, #18155 ) ) ;
#30024 = ADVANCED_FACE ( 'NONE', ( #1583 ), #17398, .T. ) ;
#30025 = EDGE_LOOP ( 'NONE', ( #20900, #29788, #22980, #38248, #37862 ) ) ;
#30026 = CARTESIAN_POINT ( 'NONE',  ( 0.03272157658042155332, -1.558775077797650566, -0.6419537545420734848 ) ) ;
#30027 = CARTESIAN_POINT ( 'NONE',  ( 2.804450709937611668E-16, 1.120325691531909986E-16, 0.1700000000000000400 ) ) ;
#30028 = CARTESIAN_POINT ( 'NONE',  ( 0.1181081361290538395, -0.8884863947959633634, 0.5437361635629905932 ) ) ;
#30029 = CARTESIAN_POINT ( 'NONE',  ( -0.1552051794442718957, 0.4812910476514236646, 0.09878871670238409397 ) ) ;
#30030 = CARTESIAN_POINT ( 'NONE',  ( 0.5423560421123170272, -1.654562585178021017, -0.5568277168365926011 ) ) ;
#30031 = DIRECTION ( 'NONE',  ( 0.3515883117872520836, 4.264480453763185162E-16, 0.9361547195921142706 ) ) ;
#30032 = DIRECTION ( 'NONE',  ( 1.000000000000000000, 0.000000000000000000, 0.000000000000000000 ) ) ;
#30033 = CARTESIAN_POINT ( 'NONE',  ( 0.02953079040095700838, 0.2329676531120452587, -0.4763574306556336291 ) ) ;
#30034 = EDGE_CURVE ( 'NONE', #21212, #22522, #21330, .T. ) ;
#30035 = CARTESIAN_POINT ( 'NONE',  ( 0.1852724517579373009, -0.8388905295248703098, 0.1482875376949696067 ) ) ;
#30036 = DIRECTION ( 'NONE',  ( 0.000000000000000000, -0.5877852522924936762, -0.8090169943749325743 ) ) ;
#30037 = PERSON_AND_ORGANIZATION ( #28500, #32463 ) ;
#30038 = APPLIED_PERSON_AND_ORGANIZATION_ASSIGNMENT ( #25490, #9834, ( #3852 ) ) ;
#30039 = TOROIDAL_SURFACE ( 'NONE', #24790, 0.1333070866141734256, 0.02999999999999999889 ) ;
#30040 = CARTESIAN_POINT ( 'NONE',  ( 0.02162899328625018588, -1.067328559141285771, 0.6314244029302625849 ) ) ;
#30041 = CARTESIAN_POINT ( 'NONE',  ( 0.5697138663266668734, -1.615732236462104954, -0.5166151207188711680 ) ) ;
#30042 = APPLICATION_CONTEXT ( 'configuration controlled 3d designs of mechanical parts and assemblies' ) ;
#30043 = CARTESIAN_POINT ( 'NONE',  ( -2.112273405726188513E-14, -2.183180860297921466, -0.4937760292030871079 ) ) ;
#30044 =( BOUNDED_SURFACE ( )  B_SPLINE_SURFACE ( 3, 2, ( 
 ( #17493, #17877, #8420 ),
 ( #4926, #30045, #37009 ),
 ( #24088, #14384, #20583 ),
 ( #11113, #18098, #4714 ),
 ( #30444, #2272, #30652 ),
 ( #26763, #36197, #24476 ),
 ( #8010, #36800, #23880 ),
 ( #20796, #27160, #11721 ),
 ( #1679, #26948, #8611 ),
 ( #21185, #39482, #11311 ),
 ( #14812, #36408, #29837 ),
 ( #27375, #8221, #39693 ),
 ( #11526, #5124, #20987 ),
 ( #33318, #36617, #33503 ),
 ( #5315, #33720, #5536 ),
 ( #2473, #15009, #27563 ),
 ( #40086, #11915, #8833 ),
 ( #17281, #21411, #14028 ),
 ( #23323, #29668, #26803 ),
 ( #22712, #1123, #16514 ),
 ( #23110, #1511, #22916 ),
 ( #38522, #35635, #29054 ),
 ( #16925, #19799, #924 ),
 ( #26193, #13430, #32949 ),
 ( #17120, #13628, #7657 ),
 ( #4366, #26390, #26604 ),
 ( #29882, #35244, #26000 ),
 ( #29271, #3953, #38717 ),
 ( #4551, #4752, #7044 ),
 ( #39138, #20017, #10964 ),
 ( #32336, #10354, #20225 ),
 ( #29469, #32746, #23524 ),
 ( #32546, #35432, #7442 ),
 ( #1313, #7230, #38917 ),
 ( #10749, #32146, #13820 ),
 ( #35845, #19613, #10539 ),
 ( #36041, #7843, #20415 ),
 ( #17326, #4158, #1721 ),
 ( #14238, #10141, #16725 ),
 ( #39520, #24316, #21451 ),
 ( #39736, #2312, #33978 ),
 ( #36237, #17716, #20629 ),
 ( #26989, #30082, #5781 ),
 ( #21228, #36452, #27600 ) ),
 .UNSPECIFIED., .F., .F., .F. ) 
 B_SPLINE_SURFACE_WITH_KNOTS ( ( 4, 2, 2, 2, 2, 2, 2, 2, 2, 2, 2, 2, 2, 2, 2, 2, 2, 2, 2, 2, 2, 4 ),
 ( 3, 3 ),
 ( 0.001346002852697868917, 0.002596997597215204134, 0.003847992341732539567, 0.004473489713991207067, 0.005098987086249874567, 0.006349981830767210435, 0.007600976575284546302, 0.008226473947543213802, 0.008851971319801881302, 0.01010296606431921630, 0.01135396080883655130, 0.01260495555335388804, 0.01323045292561255554, 0.01385595029787122304, 0.01448144767012989054, 0.01510694504238855804, 0.01635793978690589304, 0.01760893453142322804, 0.01885992927594056304, 0.01948542664819923054, 0.02011092402045789804, 0.02136191876497523304 ),
 ( 0.000000000000000000, 1.000000000000000000 ),
 .UNSPECIFIED. ) 
 GEOMETRIC_REPRESENTATION_ITEM ( )  RATIONAL_B_SPLINE_SURFACE ( (
 ( 1.000000000000000000, 0.6289600335726139857, 1.000000000000000000),
 ( 1.000000000000000000, 0.6292818987205170966, 1.000000000000000000),
 ( 1.000000000000000000, 0.6297744943890225544, 1.000000000000000000),
 ( 1.000000000000000000, 0.6308798029848204925, 1.000000000000000000),
 ( 1.000000000000000000, 0.6314937475243069809, 1.000000000000000000),
 ( 1.000000000000000000, 0.6324446813422345270, 1.000000000000000000),
 ( 1.000000000000000000, 0.6327693011710547877, 1.000000000000000000),
 ( 1.000000000000000000, 0.6334165357267688146, 1.000000000000000000),
 ( 1.000000000000000000, 0.6337398306086132749, 1.000000000000000000),
 ( 1.000000000000000000, 0.6347105868218758662, 1.000000000000000000),
 ( 1.000000000000000000, 0.6353603024733837090, 1.000000000000000000),
 ( 1.000000000000000000, 0.6366634021563924994, 1.000000000000000000),
 ( 1.000000000000000000, 0.6372927617045243132, 1.000000000000000000),
 ( 1.000000000000000000, 0.6381953573391411227, 1.000000000000000000),
 ( 1.000000000000000000, 0.6384894769518629776, 1.000000000000000000),
 ( 1.000000000000000000, 0.6390667812190622410, 1.000000000000000000),
 ( 1.000000000000000000, 0.6393504911485946574, 1.000000000000000000),
 ( 1.000000000000000000, 0.6401755864900929849, 1.000000000000000000),
 ( 1.000000000000000000, 0.6406983120072226034, 1.000000000000000000),
 ( 1.000000000000000000, 0.6417455103317676324, 1.000000000000000000),
 ( 1.000000000000000000, 0.6422727239750118944, 1.000000000000000000),
 ( 1.000000000000000000, 0.6433117747521388541, 1.000000000000000000),
 ( 1.000000000000000000, 0.6438273952226162278, 1.000000000000000000),
 ( 1.000000000000000000, 0.6446165130563749068, 1.000000000000000000),
 ( 1.000000000000000000, 0.6448812679222618582, 1.000000000000000000),
 ( 1.000000000000000000, 0.6454115060670834181, 1.000000000000000000),
 ( 1.000000000000000000, 0.6456783656519925474, 1.000000000000000000),
 ( 1.000000000000000000, 0.6462228309538587956, 1.000000000000000000),
 ( 1.000000000000000000, 0.6465004957945182928, 1.000000000000000000),
 ( 1.000000000000000000, 0.6470729932895772363, 1.000000000000000000),
 ( 1.000000000000000000, 0.6473695932598104719, 1.000000000000000000),
 ( 1.000000000000000000, 0.6482737582539809251, 1.000000000000000000),
 ( 1.000000000000000000, 0.6488977369596267142, 1.000000000000000000),
 ( 1.000000000000000000, 0.6501749241777317057, 1.000000000000000000),
 ( 1.000000000000000000, 0.6508319705051489601, 1.000000000000000000),
 ( 1.000000000000000000, 0.6521161713507420687, 1.000000000000000000),
 ( 1.000000000000000000, 0.6527515169048989652, 1.000000000000000000),
 ( 1.000000000000000000, 0.6536932375029560482, 1.000000000000000000),
 ( 1.000000000000000000, 0.6540055346228418331, 1.000000000000000000),
 ( 1.000000000000000000, 0.6546044083911876088, 1.000000000000000000),
 ( 1.000000000000000000, 0.6548926905623442263, 1.000000000000000000),
 ( 1.000000000000000000, 0.6557056282628960231, 1.000000000000000000),
 ( 1.000000000000000000, 0.6561814253999803670, 1.000000000000000000),
 ( 1.000000000000000000, 0.6565078065782231631, 1.000000000000000000) ) ) 
 REPRESENTATION_ITEM ( '' )  SURFACE ( )  );
#30045 = CARTESIAN_POINT ( 'NONE',  ( 1.405866954095903676E-05, -0.4259765552297195557, 0.1334928998232308428 ) ) ;
#30046 = CARTESIAN_POINT ( 'NONE',  ( 0.4621675984227249789, -1.110867290327286261, 0.5635151220948720896 ) ) ;
#30047 = CARTESIAN_POINT ( 'NONE',  ( -2.070754768975509474, -0.09959325338431662678, 0.3750000000000004996 ) ) ;
#30048 = CARTESIAN_POINT ( 'NONE',  ( -0.02000000000000000042, -1.845925619402022155, -0.3444148183989317880 ) ) ;
#30049 = ORIENTED_EDGE ( 'NONE', *, *, #35301, .F. ) ;
#30050 = VERTEX_POINT ( 'NONE', #39401 ) ;
#30051 = CARTESIAN_POINT ( 'NONE',  ( 0.01548846960703768524, 0.5198120922912046193, -0.07362328916749273644 ) ) ;
#30052 = EDGE_LOOP ( 'NONE', ( #14992, #25980, #25502, #5443 ) ) ;
#30053 = CARTESIAN_POINT ( 'NONE',  ( 0.5604557356148186509, -1.426020855739283943, 0.7554199595131929623 ) ) ;
#30055 = EDGE_LOOP ( 'NONE', ( #11024, #14723, #40482 ) ) ;
#30054 = CARTESIAN_POINT ( 'NONE',  ( -0.001702386183366518761, -0.8269161091246169937, 0.06756100155804112273 ) ) ;
#30056 = ORIENTED_EDGE ( 'NONE', *, *, #34263, .F. ) ;
#30057 = CARTESIAN_POINT ( 'NONE',  ( 0.2132426129924576141, -0.7277951702479017460, 0.6835290371355510208 ) ) ;
#30058 = EDGE_CURVE ( 'NONE', #23947, #4285, #20487, .T. ) ;
#30059 = ORIENTED_EDGE ( 'NONE', *, *, #39691, .F. ) ;
#30060 = CARTESIAN_POINT ( 'NONE',  ( 0.2713787642340086403, -1.664625376075213214, 0.7106118310602838051 ) ) ;
#30062 = CARTESIAN_POINT ( 'NONE',  ( 0.1574608366664733972, -1.264793525678033825, 0.6048402482925469004 ) ) ;
#30061 = LINE ( 'NONE', #4946, #6216 ) ;
#30063 = CARTESIAN_POINT ( 'NONE',  ( 0.6470677971351853630, -1.605717245651640646, -0.4588775069418976060 ) ) ;
#30064 = EDGE_CURVE ( 'NONE', #15269, #19021, #31743, .T. ) ;
#30065 = CARTESIAN_POINT ( 'NONE',  ( 0.1959288602264626367, -1.265726376210169812, -0.7137151691975773815 ) ) ;
#30067 = VERTEX_POINT ( 'NONE', #15328 ) ;
#30066 = VERTEX_POINT ( 'NONE', #25196 ) ;
#30068 = ADVANCED_FACE ( 'NONE', ( #14923 ), #23568, .F. ) ;
#30069 = CARTESIAN_POINT ( 'NONE',  ( 0.08531284324210690329, -0.8124773231580394439, 0.1722839607542651641 ) ) ;
#30070 = CARTESIAN_POINT ( 'NONE',  ( 0.1157716883191968194, -1.391468844569133223, 0.6465564330999761244 ) ) ;
#30071 = PRODUCT ( 'MAT-032', 'MAT-032', '', ( #7605 ) ) ;
#30072 = CARTESIAN_POINT ( 'NONE',  ( 0.1673863529439155173, -0.7934200884644354579, 0.5807677822519677902 ) ) ;
#30073 = CARTESIAN_POINT ( 'NONE',  ( 0.06848556979248547616, -1.327615349530146593, 0.5769412031485705583 ) ) ;
#30074 = DIRECTION ( 'NONE',  ( 1.000000000000000000, 0.000000000000000000, 0.000000000000000000 ) ) ;
#30075 = CYLINDRICAL_SURFACE ( 'NONE', #38218, 0.04999999999999998890 ) ;
#30076 = DIRECTION ( 'NONE',  ( 1.000000000000000000, 0.000000000000000000, 7.762739824594491602E-16 ) ) ;
#30077 = CARTESIAN_POINT ( 'NONE',  ( 0.01548846960707528191, -0.4638115001430989648, 0.2459753896937853235 ) ) ;
#30078 = AXIS2_PLACEMENT_3D ( 'NONE', #3375, #7825, #13055 ) ;
#30079 = CARTESIAN_POINT ( 'NONE',  ( 0.3487130776261192500, -1.632007555459813464, -0.6569214161271612618 ) ) ;
#30080 = CARTESIAN_POINT ( 'NONE',  ( -0.1157923916715205420, -0.5295015842444287246, 0.3749999999999992784 ) ) ;
#30081 = DIRECTION ( 'NONE',  ( 0.000000000000000000, -0.1725921171157282497, -0.9849933812516257214 ) ) ;
#30082 = CARTESIAN_POINT ( 'NONE',  ( -1.050216749492551567E-05, -0.9484751009321573667, 0.1331997927868723564 ) ) ;
#30083 = ADVANCED_FACE ( 'NONE', ( #9755 ), #40359, .F. ) ;
#30084 = CARTESIAN_POINT ( 'NONE',  ( 0.3479607464745829715, -1.628127890686773327, -0.4301448196738368313 ) ) ;
#30085 = DIRECTION ( 'NONE',  ( 0.000000000000000000, -0.8090169943749413450, 0.5877852522924816858 ) ) ;
#30086 = CARTESIAN_POINT ( 'NONE',  ( -8.537024980200822558E-17, -0.6872203660140403514, 0.1122922589469583232 ) ) ;
#30087 = CARTESIAN_POINT ( 'NONE',  ( 0.1960870051948097048, -0.8771803234346856604, 0.3014997781122282783 ) ) ;
#30088 = PERSON_AND_ORGANIZATION ( #28500, #32463 ) ;
#30089 = CARTESIAN_POINT ( 'NONE',  ( 0.6710503155864784297, -1.387729643236325083, 0.8301965501372990941 ) ) ;
#30090 = CARTESIAN_POINT ( 'NONE',  ( 0.1316017208954911588, -1.248059642665102942, 0.5182417262812423209 ) ) ;
#30091 = CARTESIAN_POINT ( 'NONE',  ( 0.04762035657658860582, 0.04295292190960727646, -0.4802795956081228335 ) ) ;
#30092 = EDGE_LOOP ( 'NONE', ( #22640, #7355, #34229 ) ) ;
#30093 = CARTESIAN_POINT ( 'NONE',  ( -0.2267371898560520127, -0.4872893062166341327, 0.3749999999999996669 ) ) ;
#30094 = CARTESIAN_POINT ( 'NONE',  ( 0.03214649760163642428, -0.7697735882589110679, 0.6362183684201799805 ) ) ;
#30095 = B_SPLINE_CURVE_WITH_KNOTS ( 'NONE', 3,
 ( #8174, #17445, #1830, #14346, #14546, #36572, #20944, #28129, #14764, #37563, #27927, #12291, #12871, #33900, #24234, #8568, #34492, #15157 ),
 .UNSPECIFIED., .F., .F.,
 ( 4, 2, 2, 2, 2, 2, 2, 2, 4 ),
 ( 0.000000000000000000, 0.0006226388165308821988, 0.001245277633061764398, 0.001867916449592646596, 0.002490555266123528795, 0.003113194082654410777, 0.003735832899185293193, 0.004358471715716175608, 0.004981110532247057590 ),
 .UNSPECIFIED. ) ;
#30096 = DIRECTION ( 'NONE',  ( -3.406373435249024214E-19, -1.000000000000000000, -7.170354002788761615E-17 ) ) ;
#30098 = ORIENTED_EDGE ( 'NONE', *, *, #17284, .F. ) ;
#30097 = DIRECTION ( 'NONE',  ( -2.563099466555627715E-12, 0.000000000000000000, -1.000000000000000000 ) ) ;
#30099 = CARTESIAN_POINT ( 'NONE',  ( -0.2746410161513782033, -1.739646749720735741, -0.3661865639197241507 ) ) ;
#30100 = CARTESIAN_POINT ( 'NONE',  ( 0.5804192421706322325, -1.234356152197840117, 0.7108377039426548860 ) ) ;
#30102 = ORIENTED_EDGE ( 'NONE', *, *, #16494, .F. ) ;
#30101 = ORIENTED_EDGE ( 'NONE', *, *, #1735, .T. ) ;
#30103 = CARTESIAN_POINT ( 'NONE',  ( 0.04759610422507894872, -1.631270183090236747, -0.6680909377639540070 ) ) ;
#30104 = ADVANCED_FACE ( 'NONE', ( #38339 ), #22326, .F. ) ;
#30105 = ORIENTED_EDGE ( 'NONE', *, *, #11200, .F. ) ;
#30106 = DIRECTION ( 'NONE',  ( 0.000000000000000000, 0.000000000000000000, -1.000000000000000000 ) ) ;
#30107 = CARTESIAN_POINT ( 'NONE',  ( 0.2362368525501326866, -1.230736425956878932, 0.4182417262808779679 ) ) ;
#30108 = EDGE_CURVE ( 'NONE', #23547, #5057, #14079, .T. ) ;
#30109 = DIRECTION ( 'NONE',  ( 0.000000000000000000, 3.330669073875470114E-16, 1.000000000000000000 ) ) ;
#30110 = VERTEX_POINT ( 'NONE', #1150 ) ;
#30111 = DIRECTION ( 'NONE',  ( -0.4999551463232377313, 0.8660512985181132439, 0.000000000000000000 ) ) ;
#30112 = CARTESIAN_POINT ( 'NONE',  ( 0.08630836114928065739, -0.7249243428820483226, 0.1457185332388690469 ) ) ;
#30113 = CARTESIAN_POINT ( 'NONE',  ( 0.1792747913679618443, -1.226898500125762181, 1.015033455503321136 ) ) ;
#30114 = CARTESIAN_POINT ( 'NONE',  ( 0.1121846759074304062, -0.6324519228151627148, 0.3961551049443752803 ) ) ;
#30116 = DIRECTION ( 'NONE',  ( -8.881784197001246407E-16, 2.361472542561082612E-16, -1.000000000000000000 ) ) ;
#30115 = CARTESIAN_POINT ( 'NONE',  ( 0.5908959048872449715, -1.601544548465861473, 0.4282886817583849703 ) ) ;
#30117 = CARTESIAN_POINT ( 'NONE',  ( 0.2691739887394375974, -1.194277921376554641, 0.6127582284757946418 ) ) ;
#30118 = ORIENTED_EDGE ( 'NONE', *, *, #25522, .F. ) ;
#30119 = EDGE_CURVE ( 'NONE', #13346, #10719, #31977, .T. ) ;
#30120 = ORIENTED_EDGE ( 'NONE', *, *, #4704, .T. ) ;
#30121 = CARTESIAN_POINT ( 'NONE',  ( 0.05083665881508981493, -0.4330284998000932251, -0.1917934360576678821 ) ) ;
#30122 = CARTESIAN_POINT ( 'NONE',  ( 0.2729734451281876639, -0.7689569267751511505, 0.5866520183762450324 ) ) ;
#30123 = DIRECTION ( 'NONE',  ( 2.465190328815661892E-32, 1.000000000000000000, 6.656013887802287108E-31 ) ) ;
#30124 = ADVANCED_FACE ( 'NONE', ( #19636 ), #32170, .T. ) ;
#30125 = CARTESIAN_POINT ( 'NONE',  ( 0.1905436384893574864, -0.5945559727383912252, 0.3046096357648204189 ) ) ;
#30126 = CARTESIAN_POINT ( 'NONE',  ( -0.04285561529641267187, -0.4878360864744967218, -0.08281661244626055407 ) ) ;
#30127 = ADVANCED_FACE ( 'NONE', ( #742 ), #16756, .T. ) ;
#30128 = CARTESIAN_POINT ( 'NONE',  ( 0.08116418662092184100, -1.318973274706103149, 0.4700956214235573749 ) ) ;
#30129 = EDGE_CURVE ( 'NONE', #28034, #13311, #32362, .T. ) ;
#30130 = B_SPLINE_CURVE_WITH_KNOTS ( 'NONE', 3,
 ( #35145, #13122, #16620, #12941 ),
 .UNSPECIFIED., .F., .F.,
 ( 4, 4 ),
 ( 0.000000000000000000, 0.0003267947208782309579 ),
 .UNSPECIFIED. ) ;
#30131 = CARTESIAN_POINT ( 'NONE',  ( 0.1726287778302593445, -1.825200482553405612, -0.6823101748829619728 ) ) ;
#30132 = DIRECTION ( 'NONE',  ( 0.000000000000000000, 0.000000000000000000, -1.000000000000000000 ) ) ;
#30133 = CARTESIAN_POINT ( 'NONE',  ( 0.3057296174425681579, -0.8572510462883253801, 0.6221769111833096444 ) ) ;
#30134 = DIRECTION ( 'NONE',  ( -1.000000000000000000, -0.000000000000000000, -0.000000000000000000 ) ) ;
#30135 = CARTESIAN_POINT ( 'NONE',  ( 0.03301162916267637998, 0.5156255563253913099, -0.07469829950278911168 ) ) ;
#30136 = DIRECTION ( 'NONE',  ( 0.000000000000000000, 0.000000000000000000, 1.000000000000000000 ) ) ;
#30137 = ORIENTED_EDGE ( 'NONE', *, *, #32187, .F. ) ;
#30138 = LINE ( 'NONE', #26665, #27412 ) ;
#30139 = CARTESIAN_POINT ( 'NONE',  ( -0.01548846960707490547, 0.09061086148575973886, 0.5171215251571029681 ) ) ;
#30140 = CARTESIAN_POINT ( 'NONE',  ( -0.02000000000000000042, -1.584107902207569696, 0.1773406241487738566 ) ) ;
#30141 = VERTEX_POINT ( 'NONE', #22526 ) ;
#30142 = CARTESIAN_POINT ( 'NONE',  ( 0.5296568109260144652, -1.147337575730582371, 0.6371820472447363715 ) ) ;
#30143 = CARTESIAN_POINT ( 'NONE',  ( 0.4337264196245351755, -1.120470219587671457, 0.5446312635246355338 ) ) ;
#30144 = CARTESIAN_POINT ( 'NONE',  ( 0.08200662898914722054, -0.9691756016468595636, 0.6660704738325865515 ) ) ;
#30145 = ORIENTED_EDGE ( 'NONE', *, *, #34387, .T. ) ;
#30146 = CARTESIAN_POINT ( 'NONE',  ( 0.1186103394390872201, -1.414144848331978510, 0.5683298932114988489 ) ) ;
#30147 = SHAPE_REPRESENTATION ( 'pulley screw_short', ( #27819 ), #20008 ) ;
#30148 = CARTESIAN_POINT ( 'NONE',  ( 0.03301162916267982167, -0.08829475514028595207, 0.5134720893088395854 ) ) ;
#30149 = CARTESIAN_POINT ( 'NONE',  ( 0.04047170147977369181, -0.4923646673433203502, -0.09403053665140553852 ) ) ;
#30150 = CYLINDRICAL_SURFACE ( 'NONE', #16033, 0.08000000000000000167 ) ;
#30151 = CARTESIAN_POINT ( 'NONE',  ( 0.4228361166268820304, -1.173637864075360415, 0.6740159186778078571 ) ) ;
#30152 = EDGE_CURVE ( 'NONE', #17350, #31635, #22949, .T. ) ;
#30154 = DIRECTION ( 'NONE',  ( 0.000000000000000000, 0.000000000000000000, -1.000000000000000000 ) ) ;
#30153 = CARTESIAN_POINT ( 'NONE',  ( 0.4099390216524483321, -1.131149867669359654, 0.5235510575314094028 ) ) ;
#30155 = CARTESIAN_POINT ( 'NONE',  ( -0.1142670043590668094, -0.4723146173917492918, 0.3382895567580812557 ) ) ;
#30156 = EDGE_LOOP ( 'NONE', ( #14820, #32480, #5601, #30514, #39542, #32007 ) ) ;
#30157 = EDGE_CURVE ( 'NONE', #35716, #38935, #23952, .T. ) ;
#30158 = DIRECTION ( 'NONE',  ( -0.3468893892380664479, -0.7396492646828669582, 0.5767033179097683648 ) ) ;
#30159 = VERTEX_POINT ( 'NONE', #2128 ) ;
#30160 = CARTESIAN_POINT ( 'NONE',  ( 0.1885786782586174326, -0.5477411782657776174, -0.03797464539687132878 ) ) ;
#30161 = CARTESIAN_POINT ( 'NONE',  ( 0.1608394401585168665, -0.9087424240471937420, 0.7386883132146533359 ) ) ;
#30163 = CARTESIAN_POINT ( 'NONE',  ( 0.4542621314170603442, -1.107174261221695266, -0.6608907272175488234 ) ) ;
#30162 = CARTESIAN_POINT ( 'NONE',  ( 0.7048936116999384716, -1.529749924580348530, 0.5717773534970714833 ) ) ;
#30164 = LINE ( 'NONE', #30574, #8659 ) ;
#30165 = B_SPLINE_CURVE_WITH_KNOTS ( 'NONE', 3,
 ( #27570, #40093, #18504, #37018 ),
 .UNSPECIFIED., .F., .F.,
 ( 4, 4 ),
 ( -2.702335329567562820E-05, 0.0001957598036967008186 ),
 .UNSPECIFIED. ) ;
#30166 = ORIENTED_EDGE ( 'NONE', *, *, #6121, .F. ) ;
#30167 = ORIENTED_EDGE ( 'NONE', *, *, #23489, .T. ) ;
#30168 = CARTESIAN_POINT ( 'NONE',  ( 0.5606097963238384496, -1.505408366410144083, 0.5243742338725653207 ) ) ;
#30169 = CARTESIAN_POINT ( 'NONE',  ( 0.1222183301103683672, -0.5572085505171303632, 0.1987391494479376353 ) ) ;
#30170 = ORIENTED_EDGE ( 'NONE', *, *, #28398, .T. ) ;
#30171 = CARTESIAN_POINT ( 'NONE',  ( 0.3171299009022257032, -1.761203395594564736, 0.5573299461910276031 ) ) ;
#30172 = CARTESIAN_POINT ( 'NONE',  ( 0.03474878377839876742, -0.4640666366555541433, 0.2268437812334336001 ) ) ;
#30173 = CARTESIAN_POINT ( 'NONE',  ( 0.6207080634491849436, -1.571428378261625181, 0.4182417262808776903 ) ) ;
#30174 = CARTESIAN_POINT ( 'NONE',  ( 0.1358326267964612144, -1.288717780320212558, 0.4219958763549262470 ) ) ;
#30175 = CARTESIAN_POINT ( 'NONE',  ( -0.02000000000000000042, -1.751754812988976395, -0.02481321673728002081 ) ) ;
#30176 = DIRECTION ( 'NONE',  ( -0.5000000000000000000, 0.8658613382927408120, -0.01685653730467018968 ) ) ;
#30177 = CARTESIAN_POINT ( 'NONE',  ( 0.3173647091058168779, -0.7919842589448738979, 0.7159411547141941723 ) ) ;
#30178 = CARTESIAN_POINT ( 'NONE',  ( 0.3769271849960352250, -1.703883853206813459, -0.6148311252412128614 ) ) ;
#30179 = CARTESIAN_POINT ( 'NONE',  ( -0.1617138679863671380, 0.4681656832120512646, 0.3382895567580770924 ) ) ;
#30180 = CARTESIAN_POINT ( 'NONE',  ( 0.6499855218573453719, -1.553698270513451440, -0.6113109915954698659 ) ) ;
#30181 = CARTESIAN_POINT ( 'NONE',  ( 0.03999249430411287026, -1.701782669491467948, -0.6675301993621318708 ) ) ;
#30182 = CARTESIAN_POINT ( 'NONE',  ( 0.02999923007304734768, -2.091069160207820410, -0.2612343372939072705 ) ) ;
#30183 = CARTESIAN_POINT ( 'NONE',  ( 0.04155248107635942795, 0.2901916982059709604, -0.3701002694350334910 ) ) ;
#30184 = CARTESIAN_POINT ( 'NONE',  ( 0.08521903690165112677, -1.316213625887622696, 0.4631828244221000701 ) ) ;
#30185 = CARTESIAN_POINT ( 'NONE',  ( 0.0003038568743942667081, -0.4444331504931744448, 0.2553847410507332771 ) ) ;
#30186 = CARTESIAN_POINT ( 'NONE',  ( 0.5803799243415090903, -1.524048604864560286, -0.4565139846630590359 ) ) ;
#30187 = DIRECTION ( 'NONE',  ( -1.000000000000000000, -0.000000000000000000, -0.000000000000000000 ) ) ;
#30188 = CARTESIAN_POINT ( 'NONE',  ( 0.5942223284369342329, -1.599512312265707115, 0.4182417262808810765 ) ) ;
#30189 = ORIENTED_EDGE ( 'NONE', *, *, #16968, .F. ) ;
#30190 = CARTESIAN_POINT ( 'NONE',  ( 0.4435963532280620680, -1.112752012059924134, 0.5972808037033706663 ) ) ;
#30191 = CARTESIAN_POINT ( 'NONE',  ( 0.4090604450045443596, -1.131420581850358653, 0.3667417262808778666 ) ) ;
#30192 = DIRECTION ( 'NONE',  ( 0.000000000000000000, -0.3090169943749502823, -0.9510565162951527540 ) ) ;
#30193 = CARTESIAN_POINT ( 'NONE',  ( -0.02953079040095652960, 0.3810518745593862167, -0.3687679460475775106 ) ) ;
#30194 = CARTESIAN_POINT ( 'NONE',  ( 0.5216898644270308028, -1.329855447211024666, 0.6139483236913935160 ) ) ;
#30196 = ORIENTED_EDGE ( 'NONE', *, *, #644, .T. ) ;
#30195 = CARTESIAN_POINT ( 'NONE',  ( -0.1529829672178498190, 0.4739133692255307895, 0.09550516375514117584 ) ) ;
#30197 = CARTESIAN_POINT ( 'NONE',  ( 0.5138235575674273692, -1.118575097671381080, 0.5744212141803229921 ) ) ;
#30198 = ORIENTED_EDGE ( 'NONE', *, *, #32004, .F. ) ;
#30199 = CARTESIAN_POINT ( 'NONE',  ( 0.6984663268742642428, -1.558725849730709934, -0.5155029497116575543 ) ) ;
#30200 = ORIENTED_EDGE ( 'NONE', *, *, #35301, .T. ) ;
#30201 = CARTESIAN_POINT ( 'NONE',  ( 0.3204479958614548929, -1.182666560659948907, 0.5682417262808776570 ) ) ;
#30202 = CARTESIAN_POINT ( 'NONE',  ( 0.3146425706043863846, -1.494729834945346836, 0.8673829083298324472 ) ) ;
#30204 = CARTESIAN_POINT ( 'NONE',  ( 0.1871331107182152009, -0.5893403707559643490, 0.009665131869706357695 ) ) ;
#30203 = CARTESIAN_POINT ( 'NONE',  ( 0.6964926828203267251, -1.497596446741557452, 0.4801749555793174973 ) ) ;
#30205 = CARTESIAN_POINT ( 'NONE',  ( 0.1499999999999994671, 0.4730347584886748780, -0.2341461249029861691 ) ) ;
#30206 = EDGE_LOOP ( 'NONE', ( #3701, #8911, #2843, #24427, #6259 ) ) ;
#30207 = VERTEX_POINT ( 'NONE', #20441 ) ;
#30208 = CARTESIAN_POINT ( 'NONE',  ( 0.1548063152929342046, -1.283648478974594109, -0.6986461007580347937 ) ) ;
#30209 = CARTESIAN_POINT ( 'NONE',  ( 0.3699999728189415915, -2.086898135891332995, -0.5178658011735879363 ) ) ;
#30210 = CARTESIAN_POINT ( 'NONE',  ( 0.07974598588771943108, -0.8334789133843516495, 0.2137242551589284278 ) ) ;
#30211 = CARTESIAN_POINT ( 'NONE',  ( 0.1551413863202326104, -1.283415300285971172, -0.3361184124323285949 ) ) ;
#30212 = CARTESIAN_POINT ( 'NONE',  ( -0.1684323895664520399, 0.5231977504174887272, 0.3032895567580809471 ) ) ;
#30213 = CARTESIAN_POINT ( 'NONE',  ( -0.1679391139942039701, 0.5216964164669857240, 0.3184569295944739142 ) ) ;
#30214 = DIRECTION ( 'NONE',  ( -1.000000000000000000, -7.857794173099924470E-32, -8.628166150854818811E-32 ) ) ;
#30215 = SPHERICAL_SURFACE ( 'NONE', #15911, 0.01499999999999999944 ) ;
#30216 = CARTESIAN_POINT ( 'NONE',  ( 0.6555154469039060627, -1.476457112320177067, 0.4182417262808776348 ) ) ;
#30217 = DIRECTION ( 'NONE',  ( 0.000000000000000000, 0.000000000000000000, 1.000000000000000000 ) ) ;
#30218 = APPROVAL_ROLE ( '' ) ;
#30219 = CARTESIAN_POINT ( 'NONE',  ( 0.05107123952191217064, -1.249085498977453357, 0.6677375136145999868 ) ) ;
#30220 = CARTESIAN_POINT ( 'NONE',  ( 0.5247102883936010098, -1.203215684353998727, 0.6057417262809794423 ) ) ;
#30221 = FACE_OUTER_BOUND ( 'NONE', #3247, .T. ) ;
#30222 = DIRECTION ( 'NONE',  ( 0.8660512985181134660, 0.4999551463232371762, 0.000000000000000000 ) ) ;
#30223 = CARTESIAN_POINT ( 'NONE',  ( 0.4182650443266206497, -1.104802627502811774, 0.5963647967864725841 ) ) ;
#30224 = CARTESIAN_POINT ( 'NONE',  ( 0.03113248654051816583, -0.3767386922704979990, -0.2665524483967541269 ) ) ;
#30225 = AXIS2_PLACEMENT_3D ( 'NONE', #34892, #34694, #35105 ) ;
#30226 = DIRECTION ( 'NONE',  ( 1.000000000000000000, -1.998486013202569589E-12, -1.557674999835046357E-12 ) ) ;
#30227 = ORIENTED_EDGE ( 'NONE', *, *, #26883, .T. ) ;
#30228 = ORIENTED_EDGE ( 'NONE', *, *, #37400, .F. ) ;
#30229 = CIRCLE ( 'NONE', #32874, 0.07999999999999996003 ) ;
#30230 = DIRECTION ( 'NONE',  ( -0.4999999999999962252, 0.4092454907131379271, -0.7632287522957755810 ) ) ;
#30231 = ORIENTED_EDGE ( 'NONE', *, *, #34083, .F. ) ;
#30232 = CARTESIAN_POINT ( 'NONE',  ( 0.4203826191881493979, -1.700944664958275343, -0.4172566670736510552 ) ) ;
#30234 = ORIENTED_EDGE ( 'NONE', *, *, #11903, .F. ) ;
#30233 = CARTESIAN_POINT ( 'NONE',  ( -0.1142670043590607726, -0.4723146173917092128, 0.1178658435936972976 ) ) ;
#30236 = ORIENTED_EDGE ( 'NONE', *, *, #30843, .F. ) ;
#30235 = CARTESIAN_POINT ( 'NONE',  ( 0.007561979894622030025, -0.7583094115173071303, 0.004127483746527383680 ) ) ;
#30237 = VERTEX_POINT ( 'NONE', #38951 ) ;
#30238 = FACE_OUTER_BOUND ( 'NONE', #16694, .T. ) ;
#30239 = EDGE_LOOP ( 'NONE', ( #25601, #1300, #2632, #6258, #3383 ) ) ;
#30240 = EDGE_CURVE ( 'NONE', #11393, #20672, #8080, .T. ) ;
#30241 = CARTESIAN_POINT ( 'NONE',  ( 0.2664190893233142621, -1.675340114736260766, 0.5742097616013166483 ) ) ;
#30243 = CARTESIAN_POINT ( 'NONE',  ( 0.1404535776246665646, -1.274393186057628746, 0.6056389588256660961 ) ) ;
#30242 = CARTESIAN_POINT ( 'NONE',  ( 0.05999999999999990757, -0.03575622569115821658, -0.2978615321325044363 ) ) ;
#30244 = APPLIED_PERSON_AND_ORGANIZATION_ASSIGNMENT ( #5172, #9082, ( #24016 ) ) ;
#30245 = LINE ( 'NONE', #24113, #25320 ) ;
#30246 = APPROVAL_DATE_TIME ( #8442, #11774 ) ;
#30247 = CARTESIAN_POINT ( 'NONE',  ( 0.5382307432915078849, -1.161159458769174257, 0.5682417262808779901 ) ) ;
#30249 = ORIENTED_EDGE ( 'NONE', *, *, #16976, .F. ) ;
#30248 = VERTEX_POINT ( 'NONE', #10995 ) ;
#30250 = CARTESIAN_POINT ( 'NONE',  ( 0.3772117652181573022, -1.120077681141029124, 0.6236847670215859285 ) ) ;
#30251 = FACE_OUTER_BOUND ( 'NONE', #8437, .T. ) ;
#30252 = CARTESIAN_POINT ( 'NONE',  ( 0.1712609145248183695, -0.8202291507405884419, 0.6467119214775935987 ) ) ;
#30253 = CARTESIAN_POINT ( 'NONE',  ( 0.1870020358722072895, -0.7208919770472870248, 0.03184132201674819834 ) ) ;
#30254 = CARTESIAN_POINT ( 'NONE',  ( -0.02000000000000000042, -2.177105168660885326, -0.2518349584362399862 ) ) ;
#30255 = CARTESIAN_POINT ( 'NONE',  ( 0.5446946726381876047, -1.168318774461527987, 0.4638875385414486519 ) ) ;
#30256 = AXIS2_PLACEMENT_3D ( 'NONE', #9136, #21702, #34236 ) ;
#30257 = CARTESIAN_POINT ( 'NONE',  ( -0.2746410161513782033, -2.377058624452622393, -0.8919706583825134372 ) ) ;
#30258 = DIRECTION ( 'NONE',  ( 0.000000000000000000, -0.8090169943749413450, 0.5877852522924816858 ) ) ;
#30259 = DIRECTION ( 'NONE',  ( 0.4999551463232372317, -0.8660512985181135770, 0.000000000000000000 ) ) ;
#30260 = DIRECTION ( 'NONE',  ( 0.000000000000000000, 0.000000000000000000, -1.000000000000000000 ) ) ;
#30261 = AXIS2_PLACEMENT_3D ( 'NONE', #36159, #39256, #24052 ) ;
#30262 = CARTESIAN_POINT ( 'NONE',  ( 0.5696125550597064269, -1.613556559779221189, 0.4687417262808790674 ) ) ;
#30263 =( BOUNDED_SURFACE ( )  B_SPLINE_SURFACE ( 3, 2, ( 
 ( #32995, #23570, #4801 ),
 ( #36089, #19854, #17376 ),
 ( #14286, #26849, #20678 ),
 ( #39376, #36283, #35471 ),
 ( #8101, #33213, #5020 ),
 ( #30128, #1957, #16775 ) ),
 .UNSPECIFIED., .F., .F., .F. ) 
 B_SPLINE_SURFACE_WITH_KNOTS ( ( 4, 2, 4 ),
 ( 3, 3 ),
 ( 0.001110443675428536905, 0.001652974123862752283, 0.002195504572296967660 ),
 ( 0.3290584448501475134, 1.000000000000000000 ),
 .UNSPECIFIED. ) 
 GEOMETRIC_REPRESENTATION_ITEM ( )  RATIONAL_B_SPLINE_SURFACE ( (
 ( 0.8719303469039287879, 0.8053998383867736477, 1.000000000000000000),
 ( 0.8859245484685469574, 0.8266638444981970757, 1.000000000000000000),
 ( 0.8926552752790239964, 0.8368910957902011560, 1.000000000000000000),
 ( 0.8925234298264548283, 0.8366907583507090518, 1.000000000000000000),
 ( 0.8858040005613148082, 0.8264806735309744301, 1.000000000000000000),
 ( 0.8716885380514636239, 0.8050324130004183898, 1.000000000000000000) ) ) 
 REPRESENTATION_ITEM ( '' )  SURFACE ( )  );
#30264 = CARTESIAN_POINT ( 'NONE',  ( 0.4248662974673952375, -1.105221816243816546, 0.5932897847886877685 ) ) ;
#30265 = CARTESIAN_POINT ( 'NONE',  ( 0.3824787400963481354, -1.656932509623952665, -0.4003585709420097727 ) ) ;
#30266 = AXIS2_PLACEMENT_3D ( 'NONE', #30723, #2544, #24562 ) ;
#30267 = CARTESIAN_POINT ( 'NONE',  ( 0.6189546704162820490, -1.608979253401461085, -0.5612101079336522247 ) ) ;
#30268 = EDGE_CURVE ( 'NONE', #38406, #24406, #23354, .T. ) ;
#30269 = CARTESIAN_POINT ( 'NONE',  ( 0.2520126056674420467, -1.649747432069603059, 0.6712725404530499596 ) ) ;
#30270 = CARTESIAN_POINT ( 'NONE',  ( 0.4709147388527493705, -1.070627459034787954, 0.6206731519243955386 ) ) ;
#30271 = CARTESIAN_POINT ( 'NONE',  ( 0.01720488785744077667, -0.9349428739647406283, 0.5880094435653454576 ) ) ;
#30272 = EDGE_CURVE ( 'NONE', #25464, #5846, #33787, .T. ) ;
#30273 = SHAPE_DEFINITION_REPRESENTATION ( #32772, #17542 ) ;
#30274 = CARTESIAN_POINT ( 'NONE',  ( 0.1875000000000000833, -0.4595382586000822389, 0.1581505021253525878 ) ) ;
#30275 = EDGE_CURVE ( 'NONE', #6266, #31712, #6205, .T. ) ;
#30276 = CARTESIAN_POINT ( 'NONE',  ( 0.4065986444723444504, -1.612206791548977058, -0.6687116998706487125 ) ) ;
#30277 = ADVANCED_FACE ( 'NONE', ( #17147 ), #27235, .F. ) ;
#30278 = CARTESIAN_POINT ( 'NONE',  ( 0.04229974373173313318, -0.008638059335310385375, -0.4686103131113881770 ) ) ;
#30279 = DIRECTION ( 'NONE',  ( -7.771561172376107616E-16, 7.170354002788761615E-17, -1.000000000000000000 ) ) ;
#30280 = VERTEX_POINT ( 'NONE', #39767 ) ;
#30281 = CARTESIAN_POINT ( 'NONE',  ( 0.3566825243712435922, -1.732690581760574444, -0.5248316541739916907 ) ) ;
#30282 = CARTESIAN_POINT ( 'NONE',  ( 0.06685945144431634790, -0.9180018650465318064, 0.7887301370685455559 ) ) ;
#30283 = CIRCLE ( 'NONE', #36859, 0.5400000000000017009 ) ;
#30284 = CARTESIAN_POINT ( 'NONE',  ( 0.5880818911069165544, -1.487943198408785195, 0.6309528828841184378 ) ) ;
#30285 = CARTESIAN_POINT ( 'NONE',  ( 0.2968383989124028233, -1.657645728618910574, 0.4428167958024615269 ) ) ;
#30287 = ORIENTED_EDGE ( 'NONE', *, *, #26399, .T. ) ;
#30286 = CARTESIAN_POINT ( 'NONE',  ( 0.2617247662751732706, -1.216060305431710509, 0.5682417262808779901 ) ) ;
#30288 = CARTESIAN_POINT ( 'NONE',  ( 0.1999999999999789724, -2.183180860297921466, -0.5437760292030870968 ) ) ;
#30289 = CIRCLE ( 'NONE', #12559, 0.04000000000000000777 ) ;
#30290 = CARTESIAN_POINT ( 'NONE',  ( 0.6183701179687098870, -1.298963174629117479, 0.5817474467243960445 ) ) ;
#30292 = ORIENTED_EDGE ( 'NONE', *, *, #13691, .F. ) ;
#30291 = ORIENTED_EDGE ( 'NONE', *, *, #15343, .F. ) ;
#30293 = CARTESIAN_POINT ( 'NONE',  ( 0.03715482636514332027, -1.738411246770970919, -0.6683936992048589154 ) ) ;
#30294 = AXIS2_PLACEMENT_3D ( 'NONE', #599, #3826, #25458 ) ;
#30295 = ORIENTED_EDGE ( 'NONE', *, *, #31088, .F. ) ;
#30296 = CARTESIAN_POINT ( 'NONE',  ( 0.3672875303838357142, -1.616970901354836565, -0.6123576500872176531 ) ) ;
#30297 = EDGE_CURVE ( 'NONE', #26211, #38543, #10782, .T. ) ;
#30298 = CIRCLE ( 'NONE', #17146, 0.1875727115490686270 ) ;
#30299 = APPROVAL ( #5526, 'UNSPECIFIED' ) ;
#30300 = DIRECTION ( 'NONE',  ( 0.000000000000000000, 7.931692224083225994E-17, -1.000000000000000000 ) ) ;
#30301 = COORDINATED_UNIVERSAL_TIME_OFFSET ( 0, 0, .AHEAD. ) ;
#30302 = CIRCLE ( 'NONE', #23739, 0.01499999999999995087 ) ;
#30303 = CARTESIAN_POINT ( 'NONE',  ( -0.03301200226531787046, 0.4610556019031730735, -0.2426442821262900229 ) ) ;
#30304 = VERTEX_POINT ( 'NONE', #39359 ) ;
#30305 = CARTESIAN_POINT ( 'NONE',  ( 0.09670515779886533492, -1.286975611907339001, 0.5906344341303084722 ) ) ;
#30306 = CARTESIAN_POINT ( 'NONE',  ( 0.1064200553386371317, -0.7359704961837734150, 0.3761014276636525655 ) ) ;
#30307 = CARTESIAN_POINT ( 'NONE',  ( 0.1706599417108956573, -1.182744918713773519, 1.015904661483719496 ) ) ;
#30308 = CARTESIAN_POINT ( 'NONE',  ( 0.4932909056524756863, -1.526258372065918412, 0.7003863106307628428 ) ) ;
#30310 = CARTESIAN_POINT ( 'NONE',  ( 0.6984807982178791175, -1.438753897344778432, 0.5682417262808779901 ) ) ;
#30309 = CARTESIAN_POINT ( 'NONE',  ( 0.3203591660471408753, -1.762054173121580858, 0.5022354395982965292 ) ) ;
#30311 = CARTESIAN_POINT ( 'NONE',  ( 0.01762532016806284130, -0.9532778069939448207, 0.3090308271854356192 ) ) ;
#30312 = ORIENTED_EDGE ( 'NONE', *, *, #13551, .F. ) ;
#30313 = ORIENTED_EDGE ( 'NONE', *, *, #26141, .T. ) ;
#30314 = LINE ( 'NONE', #11611, #6193 ) ;
#30315 = VECTOR ( 'NONE', #8542, 39.37007874015748143 ) ;
#30316 = CARTESIAN_POINT ( 'NONE',  ( 0.4339004961413100991, -1.102577184751369455, 0.8888993553986003215 ) ) ;
#30317 = CARTESIAN_POINT ( 'NONE',  ( 0.4092580784887682732, -1.709679816849471568, -0.6081479518787427097 ) ) ;
#30318 = CARTESIAN_POINT ( 'NONE',  ( 0.4686742901286617413, -1.116548677541408185, 0.5688640544436303070 ) ) ;
#30319 = VECTOR ( 'NONE', #29875, 39.37007874015748143 ) ;
#30320 = CARTESIAN_POINT ( 'NONE',  ( 0.3764398274533635180, -1.163784180705809579, 0.4182417262808778013 ) ) ;
#30321 = CARTESIAN_POINT ( 'NONE',  ( 0.1834057154632523778, -1.261407668813178340, -0.7100906059019311822 ) ) ;
#30322 = CARTESIAN_POINT ( 'NONE',  ( 0.3182873482898154749, -1.183781612718975307, 0.5020472072821947629 ) ) ;
#30323 = CARTESIAN_POINT ( 'NONE',  ( 0.3883356530642981808, -0.9654559656950375546, 0.7100763952745350327 ) ) ;
#30324 = ADVANCED_FACE ( 'NONE', ( #1336 ), #23737, .T. ) ;
#30325 = PERSON_AND_ORGANIZATION ( #28500, #32463 ) ;
#30326 = CONICAL_SURFACE ( 'NONE', #7339, 0.1500000000000011324, 1.047197551196599630 ) ;
#30327 = CIRCLE ( 'NONE', #25080, 0.07749999999977547072 ) ;
#30328 = DIRECTION ( 'NONE',  ( 1.000000000000000000, 0.000000000000000000, 0.000000000000000000 ) ) ;
#30329 = VECTOR ( 'NONE', #18875, 39.37007874015748854 ) ;
#30330 = ADVANCED_FACE ( 'NONE', ( #17564 ), #9605, .T. ) ;
#30331 = CARTESIAN_POINT ( 'NONE',  ( 2.099101141760805602E-16, 0.2900000000000004796, 0.07499999999999940048 ) ) ;
#30332 = CARTESIAN_POINT ( 'NONE',  ( 0.1953783392200664493, -2.012295829061851560, -0.6743165020656848307 ) ) ;
#30333 = CARTESIAN_POINT ( 'NONE',  ( -0.01548846960688955027, -0.09061086148592201184, 0.5171215251575769223 ) ) ;
#30334 = DIRECTION ( 'NONE',  ( 0.000000000000000000, -0.9510565162951630791, 0.3090169943749180859 ) ) ;
#30335 = EDGE_CURVE ( 'NONE', #33860, #528, #17029, .T. ) ;
#30336 = CARTESIAN_POINT ( 'NONE',  ( -2.070754768975509474, -0.09959325338431662678, 0.3602693341844405150 ) ) ;
#30337 = ORIENTED_EDGE ( 'NONE', *, *, #440, .F. ) ;
#30338 = LINE ( 'NONE', #17598, #21361 ) ;
#30339 = DIRECTION ( 'NONE',  ( 1.000000000000000000, 0.000000000000000000, 0.000000000000000000 ) ) ;
#30340 = EDGE_CURVE ( 'NONE', #33790, #38637, #33578, .T. ) ;
#30341 = CARTESIAN_POINT ( 'NONE',  ( 0.2042129071158758913, -1.305677593605112152, 0.6884246345324352978 ) ) ;
#30342 = ORIENTED_EDGE ( 'NONE', *, *, #7422, .T. ) ;
#30343 = CARTESIAN_POINT ( 'NONE',  ( 0.05634307799789379373, 0.2780413953411660088, 0.3652007531760546044 ) ) ;
#30344 = EDGE_CURVE ( 'NONE', #17096, #40212, #997, .T. ) ;
#30345 = DIRECTION ( 'NONE',  ( 1.000000000000000000, 0.000000000000000000, 0.000000000000000000 ) ) ;
#30346 = EDGE_CURVE ( 'NONE', #13751, #26649, #7169, .T. ) ;
#30347 = CARTESIAN_POINT ( 'NONE',  ( 0.04946426091937480840, -0.4418466283164439456, -0.1805254228051831888 ) ) ;
#30348 = EDGE_CURVE ( 'NONE', #9095, #9331, #95, .T. ) ;
#30349 = CARTESIAN_POINT ( 'NONE',  ( 0.1957919492576059572, -1.993943356844413817, -0.2893518802698326065 ) ) ;
#30350 = CARTESIAN_POINT ( 'NONE',  ( 0.4687069519024180120, -1.239395243040063654, 0.5932013480186181242 ) ) ;
#30351 = VECTOR ( 'NONE', #35989, 39.37007874015748143 ) ;
#30353 = DIRECTION ( 'NONE',  ( -1.000000000000000000, -0.000000000000000000, -0.000000000000000000 ) ) ;
#30352 = FACE_OUTER_BOUND ( 'NONE', #12500, .T. ) ;
#30354 = CARTESIAN_POINT ( 'NONE',  ( -0.05083665881509014106, -0.3162195626322033548, -0.3525671453250078247 ) ) ;
#30355 = ORIENTED_EDGE ( 'NONE', *, *, #36054, .F. ) ;
#30356 = EDGE_CURVE ( 'NONE', #17560, #11732, #23301, .T. ) ;
#30357 = VERTEX_POINT ( 'NONE', #2733 ) ;
#30358 = CARTESIAN_POINT ( 'NONE',  ( 0.07317269111354535172, -1.324861932786149055, 0.5593322111943830333 ) ) ;
#30359 = ORIENTED_EDGE ( 'NONE', *, *, #16955, .F. ) ;
#30360 = CIRCLE ( 'NONE', #3424, 0.5302738246768107233 ) ;
#30361 = CARTESIAN_POINT ( 'NONE',  ( -0.02000000000000000042, -2.196071624283071788, -0.8624000883860228894 ) ) ;
#30362 = EDGE_CURVE ( 'NONE', #29483, #11737, #18161, .T. ) ;
#30363 = AXIS2_PLACEMENT_3D ( 'NONE', #871, #13378, #25955 ) ;
#30364 = CARTESIAN_POINT ( 'NONE',  ( 0.06225588220789115418, -0.5681044914483278641, 0.2679612960194602822 ) ) ;
#30366 = CARTESIAN_POINT ( 'NONE',  ( 0.000000000000000000, 0.000000000000000000, 0.000000000000000000 ) ) ;
#30365 = CARTESIAN_POINT ( 'NONE',  ( 0.06728514184456915737, -0.6483875930907525564, 0.003017575880453532335 ) ) ;
#30367 = CARTESIAN_POINT ( 'NONE',  ( 0.3048172866937527425, -1.756813269515922205, 0.5623665267386828148 ) ) ;
#30368 = B_SPLINE_CURVE_WITH_KNOTS ( 'NONE', 3,
 ( #29662, #13023, #38101, #31944, #35015, #3764, #26187, #28853, #25781, #10349 ),
 .UNSPECIFIED., .F., .F.,
 ( 4, 2, 2, 2, 4 ),
 ( 6.071532165919065186E-18, 0.0004362256165457094434, 0.0008724512330914128153, 0.001308676849637116241, 0.001744902466182819559 ),
 .UNSPECIFIED. ) ;
#30369 = ORIENTED_EDGE ( 'NONE', *, *, #35580, .T. ) ;
#30370 = CIRCLE ( 'NONE', #23806, 0.1333070866141733701 ) ;
#30371 = CARTESIAN_POINT ( 'NONE',  ( 0.3980241511492424444, -2.025796087852232752, -0.2805662142407182036 ) ) ;
#30372 = CARTESIAN_POINT ( 'NONE',  ( 0.1222449228537752230, -0.5597973469825100468, 0.2087343094629943718 ) ) ;
#30373 = CARTESIAN_POINT ( 'NONE',  ( 0.4773536554779886365, -1.668348979080164884, 0.5692827505350450679 ) ) ;
#30374 = DIRECTION ( 'NONE',  ( 1.000000000000000000, 0.000000000000000000, 0.000000000000000000 ) ) ;
#30375 = CARTESIAN_POINT ( 'NONE',  ( -0.2399999999999999079, -1.804235510932644004, -0.1101860188971505033 ) ) ;
#30376 = CARTESIAN_POINT ( 'NONE',  ( 0.1718769070500368867, -1.267826361270228519, 0.4341930484031654158 ) ) ;
#30377 = CARTESIAN_POINT ( 'NONE',  ( 0.07775718790500896205, -1.310864069790921738, 0.4781538619239825705 ) ) ;
#30378 = CARTESIAN_POINT ( 'NONE',  ( 0.2282946535672089883, -1.235122852095027479, 0.5557842531242198625 ) ) ;
#30379 = CARTESIAN_POINT ( 'NONE',  ( 0.1883801994403443147, -0.4771412664261568959, 0.2456734866192890887 ) ) ;
#30380 = CARTESIAN_POINT ( 'NONE',  ( 0.3632319344357997637, -1.747369632465606282, -0.5982111343698881534 ) ) ;
#30381 = CARTESIAN_POINT ( 'NONE',  ( 0.3740960844805631957, -1.108072201694596526, 0.5182417262812423209 ) ) ;
#30382 = CIRCLE ( 'NONE', #35639, 0.06173076923076910999 ) ;
#30383 = ADVANCED_FACE ( 'NONE', ( #30511 ), #17951, .T. ) ;
#30384 = CARTESIAN_POINT ( 'NONE',  ( 0.6316962058243321687, -1.601278944064980170, -0.5821188199280620257 ) ) ;
#30385 = CARTESIAN_POINT ( 'NONE',  ( 0.1095580259237044773, -1.391696829487717002, -0.6974751144921543800 ) ) ;
#30386 = CARTESIAN_POINT ( 'NONE',  ( 0.5912368146451574269, -1.616255995515891941, 0.5832502196827238361 ) ) ;
#30387 = EDGE_CURVE ( 'NONE', #7319, #22988, #24617, .T. ) ;
#30388 = CARTESIAN_POINT ( 'NONE',  ( 0.3695052819757340123, -1.758428263776099287, -0.4278193900811940176 ) ) ;
#30389 = DIRECTION ( 'NONE',  ( 0.000000000000000000, 0.5365213554527478168, -0.8438867430782083234 ) ) ;
#30390 = SHAPE_REPRESENTATION ( 'Pulley', ( #27819 ), #12683 ) ;
#30391 = VECTOR ( 'NONE', #25960, 39.37007874015748854 ) ;
#30392 = CARTESIAN_POINT ( 'NONE',  ( 0.002089204316143729572, -0.4812299151504488837, 0.2002484561318531031 ) ) ;
#30393 = DIRECTION ( 'NONE',  ( 0.8660512985181133550, 0.4999551463232372317, 0.000000000000000000 ) ) ;
#30394 = AXIS2_PLACEMENT_3D ( 'NONE', #25708, #10068, #848 ) ;
#30395 = DIRECTION ( 'NONE',  ( 0.000000000000000000, 0.000000000000000000, -1.000000000000000000 ) ) ;
#30397 = ORIENTED_EDGE ( 'NONE', *, *, #11458, .T. ) ;
#30396 = B_SPLINE_SURFACE_WITH_KNOTS ( 'NONE', 3, 3, ( 
 ( #37004, #24272, #11519, #12121, #21790, #6135, #5525, #36608, #18091, #8823, #31042, #20980, #2264, #37217, #18485, #30644, #2468, #8412, #33498, #30835, #21401, #27369, #33939, #14803, #24885, #5304, #5737, #21597, #34121, #37407, #18296 ),
 ( #15197, #27755, #40290, #5923, #15407, #27965, #40504, #12327, #9219, #28580, #30841, #21605, #37837, #3080, #9650, #40295, #15418, #12129, #31458, #31050, #18302, #27973, #25081, #22218, #9842, #18709, #27762, #15816, #33944, #34736, #6541 ),
 ( #28171, #19117, #37415, #24693, #12731, #12949, #5930, #37616, #18496, #34127, #2663, #15206, #31656, #37224, #38030, #3476, #9225, #9042, #2867, #40511, #9437, #28369, #12334, #21799, #24891, #25297, #25496, #34331, #22020, #6144, #31266 ),
 ( #16031, #453, #5744, #12526, #15624, #35, #34542, #3265, #235, #6349, #18922, #29576, #22833, #16630, #35750, #20138, #34942, #10053, #38630, #22623, #7145, #35159, #39036, #23017, #32665, #4469, #19528, #22411, #32062, #35354, #1232 ),
 ( #13549, #3870, #19712, #637, #16421, #29176, #28962, #13128, #25692, #38431, #38225, #17037, #29386, #13730, #25911, #19918, #32242, #1043, #10450, #26297, #6747, #1418, #19325, #6958, #38822, #828, #16241, #10271, #4065, #16846, #13933 ),
 ( #10654, #13338, #28779, #26120, #35537, #7341, #31866, #26504, #32453, #4278, #23226, #7564, #3682, #20749, #39246, #36352, #11261, #14542, #14146, #21138, #29994, #5078, #14760, #14343, #4657, #30392, #30601, #23629, #27107, #36146, #11067 ),
 ( #7956, #26906, #33064, #11474, #8169, #17442, #1827, #23831, #24041, #20530, #36569, #33667, #8374, #33272, #39641, #5481, #20941, #17638, #4871, #23442, #2223, #24231, #18044, #27324, #30185, #2015, #27516, #29783, #39438, #33463, #5270 ) ),
 .UNSPECIFIED., .F., .F., .F.,
 ( 4, 1, 1, 1, 4 ),
 ( 4, 1, 1, 1, 1, 1, 1, 1, 1, 1, 1, 1, 1, 1, 1, 1, 1, 1, 1, 1, 1, 1, 1, 1, 1, 3, 4 ),
 ( 0.000000000000000000, 0.2500000000000000000, 0.5000000000000000000, 0.7500000000000000000, 1.000000000000000000 ),
 ( 0.000000000000000000, 0.03051875000000000074, 0.04577812500000000978, 0.06103750000000000148, 0.09155625000000001956, 0.1220750000000000030, 0.1525937500000000002, 0.1831125000000000391, 0.2136312499999999948, 0.2441500000000000059, 0.2993062499999999959, 0.3544624999999999027, 0.4096187500000000314, 0.4647750000000000492, 0.5199312500000002890, 0.5750875000000000847, 0.6302437499999999915, 0.6854000000000000092, 0.7247249999999998415, 0.7640500000000001180, 0.8033749999999999503, 0.8427000000000000046, 0.8820249999999999480, 0.9213500000000000023, 0.9606749999999998346, 1.000000000000000000, 1.037727370758942724 ),
 .UNSPECIFIED. ) ;
#30398 = CARTESIAN_POINT ( 'NONE',  ( 0.4677435473941323751, -1.076338332495886840, -0.6121988916364614619 ) ) ;
#30399 = AXIS2_PLACEMENT_3D ( 'NONE', #28502, #12879, #19652 ) ;
#30400 = CARTESIAN_POINT ( 'NONE',  ( 0.3948127461878784827, -1.136156435014139099, 0.6057297418123517296 ) ) ;
#30401 = DIRECTION ( 'NONE',  ( -8.881784197001245421E-16, 2.361472542561082612E-16, -1.000000000000000000 ) ) ;
#30402 = DIRECTION ( 'NONE',  ( -2.157041537713702240E-32, 0.8709776783778059306, -0.4913225862583635584 ) ) ;
#30403 = CARTESIAN_POINT ( 'NONE',  ( 0.4697754283568603695, -1.248084093760120750, 0.7319325641689681250 ) ) ;
#30405 = EDGE_LOOP ( 'NONE', ( #30678, #32872, #18283, #26866 ) ) ;
#30404 = DIRECTION ( 'NONE',  ( -1.000000000000000000, -0.000000000000000000, -0.000000000000000000 ) ) ;
#30406 = CARTESIAN_POINT ( 'NONE',  ( 0.3472154721327633808, -0.9812419721698063535, 0.6178014265861627718 ) ) ;
#30407 = ORIENTED_EDGE ( 'NONE', *, *, #40466, .F. ) ;
#30408 = EDGE_CURVE ( 'NONE', #28184, #9108, #27256, .T. ) ;
#30409 = CARTESIAN_POINT ( 'NONE',  ( 0.07892189845977243268, -1.399197548210990627, -0.3632275770745012622 ) ) ;
#30410 = ORIENTED_EDGE ( 'NONE', *, *, #9712, .F. ) ;
#30411 = DIRECTION ( 'NONE',  ( -0.4999551463232372317, 0.8660512985181135770, -0.000000000000000000 ) ) ;
#30412 = ORIENTED_EDGE ( 'NONE', *, *, #2960, .T. ) ;
#30413 = ADVANCED_FACE ( 'NONE', ( #40573 ), #2537, .F. ) ;
#30414 = CARTESIAN_POINT ( 'NONE',  ( 0.03562321441245916431, -0.5363712146287933358, 0.1738714753025889515 ) ) ;
#30416 = CARTESIAN_POINT ( 'NONE',  ( 0.1882863373429763676, -0.5192882382158404697, 0.1376832038832177529 ) ) ;
#30415 = CARTESIAN_POINT ( 'NONE',  ( 0.7034871982223843689, -1.518834583483278156, 0.5648842057115460724 ) ) ;
#30417 = DIRECTION ( 'NONE',  ( -0.4999551463232372317, 0.8660512985181135770, -0.000000000000000000 ) ) ;
#30418 = AXIS2_PLACEMENT_3D ( 'NONE', #5919, #18480, #16409 ) ;
#30419 = EDGE_LOOP ( 'NONE', ( #22850, #12752, #27790, #10318 ) ) ;
#30420 = EDGE_LOOP ( 'NONE', ( #11831, #18, #35449, #33374, #3690 ) ) ;
#30421 = CARTESIAN_POINT ( 'NONE',  ( 0.3856095533780636853, -0.9746514165089328330, 0.6873212698995325720 ) ) ;
#30422 = ORIENTED_EDGE ( 'NONE', *, *, #38081, .T. ) ;
#30423 = DIRECTION ( 'NONE',  ( -1.000000000000000000, -0.000000000000000000, -0.000000000000000000 ) ) ;
#30424 = FACE_OUTER_BOUND ( 'NONE', #38139, .T. ) ;
#30425 = AXIS2_PLACEMENT_3D ( 'NONE', #30839, #27761, #24890 ) ;
#30426 = AXIS2_PLACEMENT_3D ( 'NONE', #23627, #33059, #27321 ) ;
#30427 = CARTESIAN_POINT ( 'NONE',  ( 0.1072518627510686412, -0.8713630855471795611, 0.4911467596464663132 ) ) ;
#30428 = CARTESIAN_POINT ( 'NONE',  ( 0.1195693017516585716, -1.324662432614883700, -0.3516852558313144916 ) ) ;
#30429 = CONICAL_SURFACE ( 'NONE', #16622, 0.1400000000000012623, 1.047197551196601850 ) ;
#30430 = DIRECTION ( 'NONE',  ( -1.000000000000000000, -0.000000000000000000, -0.000000000000000000 ) ) ;
#30431 = CONICAL_SURFACE ( 'NONE', #12786, 0.5515209409081859304, 1.047197551196598519 ) ;
#30432 = CARTESIAN_POINT ( 'NONE',  ( 0.3756489996570800405, -1.097449264068310670, 0.6348451176221490133 ) ) ;
#30433 = CARTESIAN_POINT ( 'NONE',  ( 0.02953079040095687308, 0.5250338024619264354, -0.07436286310882528339 ) ) ;
#30434 = CARTESIAN_POINT ( 'NONE',  ( 0.05082303569918638492, 0.2375724430107445106, -0.4097459652473644520 ) ) ;
#30435 =( GEOMETRIC_REPRESENTATION_CONTEXT ( 3 ) GLOBAL_UNCERTAINTY_ASSIGNED_CONTEXT ( ( #19456 ) ) GLOBAL_UNIT_ASSIGNED_CONTEXT ( ( #7660, #32548, #38719 ) ) REPRESENTATION_CONTEXT ( 'NONE', 'WORKASPACE' ) );
#30436 = CARTESIAN_POINT ( 'NONE',  ( 0.1852706725762902906, -0.8388893584440290097, 0.1474376482679014555 ) ) ;
#30437 = CARTESIAN_POINT ( 'NONE',  ( -0.02953079040095639429, 0.4684706630666080063, -0.2484463060367437248 ) ) ;
#30438 = PERSON_AND_ORGANIZATION_ROLE ( 'creator' ) ;
#30439 = EDGE_CURVE ( 'NONE', #21190, #7716, #21497, .T. ) ;
#30440 = CARTESIAN_POINT ( 'NONE',  ( 0.4768631172705831145, -1.133883247812649930, 0.4707179390482816861 ) ) ;
#30441 = CARTESIAN_POINT ( 'NONE',  ( 0.4546337798721356571, -1.243669536373561701, 0.6057417262809813296 ) ) ;
#30442 = CARTESIAN_POINT ( 'NONE',  ( -0.05464101615137796630, -1.750394882718339762, -0.1142373872069606250 ) ) ;
#30443 = B_SPLINE_CURVE_WITH_KNOTS ( 'NONE', 3,
 ( #4155, #17117, #29666, #26601 ),
 .UNSPECIFIED., .F., .F.,
 ( 4, 4 ),
 ( 4.336808689942017736E-19, 0.0004444667336122164083 ),
 .UNSPECIFIED. ) ;
#30444 = CARTESIAN_POINT ( 'NONE',  ( 0.01211358213722261989, -0.4403755143391286375, 0.06599023287002830918 ) ) ;
#30445 = CARTESIAN_POINT ( 'NONE',  ( -0.2399999999999999079, -3.985676108854518507, -0.6623095129438225648 ) ) ;
#30446 = CARTESIAN_POINT ( 'NONE',  ( -0.2746410161513779258, -2.416006048095809877, -1.059240699271965402 ) ) ;
#30447 = CARTESIAN_POINT ( 'NONE',  ( 0.01548846960703826464, 0.4638115001431027951, 0.2459753896937752204 ) ) ;
#30448 = ORIENTED_EDGE ( 'NONE', *, *, #16779, .F. ) ;
#30449 = AXIS2_PLACEMENT_3D ( 'NONE', #25448, #28729, #7092 ) ;
#30450 = VERTEX_POINT ( 'NONE', #3143 ) ;
#30451 = CIRCLE ( 'NONE', #12071, 0.1000000000000000194 ) ;
#30452 = EDGE_LOOP ( 'NONE', ( #7820, #17989, #20045, #21055 ) ) ;
#30453 = DIRECTION ( 'NONE',  ( 0.4999551463241143634, -0.8660512985176070933, 0.000000000000000000 ) ) ;
#30454 = CARTESIAN_POINT ( 'NONE',  ( -0.1208103506584077974, -0.5051587313117239519, 0.1401839043133216722 ) ) ;
#30456 = EDGE_LOOP ( 'NONE', ( #25060, #179, #38011, #28785 ) ) ;
#30455 = CARTESIAN_POINT ( 'NONE',  ( 0.0007308754721319292262, -0.6160987163282929391, 0.002788468881659194980 ) ) ;
#30457 = CIRCLE ( 'NONE', #12078, 0.2200000000000000566 ) ;
#30458 = VERTEX_POINT ( 'NONE', #30715 ) ;
#30459 = DIRECTION ( 'NONE',  ( -1.000000000000000000, -2.341930812374887555E-31, 1.664003471950578127E-31 ) ) ;
#30460 = ORIENTED_EDGE ( 'NONE', *, *, #26772, .F. ) ;
#30461 = AXIS2_PLACEMENT_3D ( 'NONE', #36653, #11757, #8458 ) ;
#30462 = CARTESIAN_POINT ( 'NONE',  ( 0.2562100995515492197, -1.500925799399086102, 0.8984186356539709539 ) ) ;
#30464 = CARTESIAN_POINT ( 'NONE',  ( 0.5150521149620285177, -1.603685588959441466, -0.4158162930565508786 ) ) ;
#30463 = DIRECTION ( 'NONE',  ( -0.4999551463232373427, 0.8660512985181134660, -0.000000000000000000 ) ) ;
#30465 = CARTESIAN_POINT ( 'NONE',  ( 0.1840567930975518796, -0.8547793429265486687, 0.1477568935609660794 ) ) ;
#30466 = DATE_TIME_ROLE ( 'classification_date' ) ;
#30467 = EDGE_CURVE ( 'NONE', #26971, #1802, #24553, .T. ) ;
#30468 = DIRECTION ( 'NONE',  ( 4.930380657631322689E-32, 0.7472307839325097456, 0.6645646360916346307 ) ) ;
#30470 = ORIENTED_EDGE ( 'NONE', *, *, #33570, .T. ) ;
#30469 = ORIENTED_EDGE ( 'NONE', *, *, #33373, .T. ) ;
#30471 = FACE_OUTER_BOUND ( 'NONE', #15281, .T. ) ;
#30472 = DIRECTION ( 'NONE',  ( 0.8660512985181134660, 0.4999551463232373427, 0.000000000000000000 ) ) ;
#30473 = CARTESIAN_POINT ( 'NONE',  ( 0.2805973409072567981, -0.9951498133751814912, 0.7619205245393454451 ) ) ;
#30474 = CARTESIAN_POINT ( 'NONE',  ( 0.02011115336535013176, -1.001108279069293339, 0.5117138269811281059 ) ) ;
#30475 = FACE_OUTER_BOUND ( 'NONE', #28937, .T. ) ;
#30476 = CARTESIAN_POINT ( 'NONE',  ( -0.3000000000000000999, -2.891403747035983240, -0.7012825271972917829 ) ) ;
#30477 = CARTESIAN_POINT ( 'NONE',  ( 0.4114935271034952380, -1.686083435099848593, -0.4173439381843787044 ) ) ;
#30478 = CARTESIAN_POINT ( 'NONE',  ( -0.09579104668929019906, -0.04310840302198021973, 0.3749999999999993894 ) ) ;
#30479 = CARTESIAN_POINT ( 'NONE',  ( 0.3377296246109549038, -1.643986942658042905, -0.6496138543457681269 ) ) ;
#30480 = AXIS2_PLACEMENT_3D ( 'NONE', #16633, #38633, #23020 ) ;
#30481 = DIRECTION ( 'NONE',  ( 0.9591734532964046878, 0.2828184691484092461, 0.000000000000000000 ) ) ;
#30482 = CARTESIAN_POINT ( 'NONE',  ( 0.3067120372624415614, -1.770199942203851240, 0.4177417262808785781 ) ) ;
#30483 = CIRCLE ( 'NONE', #1605, 0.03000000000000002318 ) ;
#30484 = FACE_BOUND ( 'NONE', #34547, .T. ) ;
#30485 = DIRECTION ( 'NONE',  ( 6.162975822039154730E-33, -1.000000000000000000, -2.220446049250313081E-16 ) ) ;
#30486 = CARTESIAN_POINT ( 'NONE',  ( 0.03474878377839887844, -0.2421023663934862569, 0.4562919991932272157 ) ) ;
#30487 = CARTESIAN_POINT ( 'NONE',  ( 0.2491647336858476003, -1.658092311124387708, 0.5917354811442696594 ) ) ;
#30488 = AXIS2_PLACEMENT_3D ( 'NONE', #13962, #26533, #39073 ) ;
#30489 = FACE_OUTER_BOUND ( 'NONE', #32265, .T. ) ;
#30490 = DATE_TIME_ROLE ( 'creation_date' ) ;
#30491 = CARTESIAN_POINT ( 'NONE',  ( 0.6277259471038021399, -1.316916163187945799, 0.8316945246157878557 ) ) ;
#30492 = AXIS2_PLACEMENT_3D ( 'NONE', #14800, #27366, #39891 ) ;
#30493 = CARTESIAN_POINT ( 'NONE',  ( 0.05078310099560752466, 0.04880952477023812325, -0.4712228254505121394 ) ) ;
#30494 = CARTESIAN_POINT ( 'NONE',  ( 0.7824441210996690987, -1.527567036798914035, -0.5155029497116575543 ) ) ;
#30495 = ORIENTED_EDGE ( 'NONE', *, *, #21009, .F. ) ;
#30496 = DIRECTION ( 'NONE',  ( 0.000000000000000000, 0.000000000000000000, -1.000000000000000000 ) ) ;
#30497 = CARTESIAN_POINT ( 'NONE',  ( 0.1072529199298410257, -1.089089271014722859, 0.8806249471138073437 ) ) ;
#30498 = AXIS2_PLACEMENT_3D ( 'NONE', #4395, #35874, #26830 ) ;
#30499 = CARTESIAN_POINT ( 'NONE',  ( 0.1397421702044318870, -0.6236803416123793964, 0.3668591128627327058 ) ) ;
#30500 = CARTESIAN_POINT ( 'NONE',  ( 0.3731358418028291601, -1.763283501847145773, -0.4358462980061182379 ) ) ;
#30502 = ORIENTED_EDGE ( 'NONE', *, *, #26303, .T. ) ;
#30501 = CARTESIAN_POINT ( 'NONE',  ( -0.2399999999999999079, -3.709638442894640509, -0.03148515058508863373 ) ) ;
#30503 = VECTOR ( 'NONE', #29511, 39.37007874015748854 ) ;
#30504 = CARTESIAN_POINT ( 'NONE',  ( 0.5081268369560435483, -1.127385812641128693, 0.7490048996577514107 ) ) ;
#30506 = ORIENTED_EDGE ( 'NONE', *, *, #26651, .T. ) ;
#30505 = ORIENTED_EDGE ( 'NONE', *, *, #37100, .F. ) ;
#30507 = CARTESIAN_POINT ( 'NONE',  ( 0.6383297146155822999, -1.332514953497987653, 0.7863315818369056576 ) ) ;
#30508 = AXIS2_PLACEMENT_3D ( 'NONE', #36059, #32762, #4564 ) ;
#30509 = VECTOR ( 'NONE', #20100, 39.37007874015748143 ) ;
#30510 = DIRECTION ( 'NONE',  ( 1.000000000000000000, 1.119941574063613413E-31, -7.771561172376107616E-16 ) ) ;
#30511 = FACE_OUTER_BOUND ( 'NONE', #22173, .T. ) ;
#30512 = COORDINATED_UNIVERSAL_TIME_OFFSET ( 0, 0, .AHEAD. ) ;
#30513 = FACE_OUTER_BOUND ( 'NONE', #16396, .T. ) ;
#30514 = ORIENTED_EDGE ( 'NONE', *, *, #20539, .T. ) ;
#30515 = EDGE_CURVE ( 'NONE', #17597, #22278, #15682, .T. ) ;
#30516 = CARTESIAN_POINT ( 'NONE',  ( 0.08789146819946426492, -0.7060428058465696433, 0.1983783520454339422 ) ) ;
#30517 = EDGE_CURVE ( 'NONE', #13700, #23240, #31821, .T. ) ;
#30518 = CARTESIAN_POINT ( 'NONE',  ( 0.2001820407311839800, -1.287744702331634850, 1.033572112086078132 ) ) ;
#30519 = CARTESIAN_POINT ( 'NONE',  ( 0.3218516010127101534, -1.144099206277331637, 0.8304979311448332790 ) ) ;
#30520 = AXIS2_PLACEMENT_3D ( 'NONE', #10266, #34537, #37831 ) ;
#30522 = CARTESIAN_POINT ( 'NONE',  ( -0.001418955495163486775, -0.8211291000492192405, 0.04345076978617073982 ) ) ;
#30521 = CARTESIAN_POINT ( 'NONE',  ( 0.3263383112081457149, -1.765042748300605480, 0.4949248276282361969 ) ) ;
#30523 = CARTESIAN_POINT ( 'NONE',  ( 0.06244861065054558430, -1.151270256393961855, 0.6619143190264936694 ) ) ;
#30524 = ORIENTED_EDGE ( 'NONE', *, *, #9484, .F. ) ;
#30525 = ORIENTED_EDGE ( 'NONE', *, *, #4503, .T. ) ;
#30526 = ADVANCED_FACE ( 'NONE', ( #27628 ), #34191, .T. ) ;
#30527 = DIRECTION ( 'NONE',  ( 1.387778780781449225E-15, 0.000000000000000000, 1.000000000000000000 ) ) ;
#30528 = CARTESIAN_POINT ( 'NONE',  ( 0.6324602634195602979, -1.323077396536881611, 0.7914183504951575188 ) ) ;
#30529 = EDGE_CURVE ( 'NONE', #35222, #31881, #6842, .T. ) ;
#30530 = CARTESIAN_POINT ( 'NONE',  ( 0.000000000000000000, -0.4415087982045245996, -0.1343585914930099934 ) ) ;
#30531 = CARTESIAN_POINT ( 'NONE',  ( 0.3699999999999786793, -2.097675824466503691, -0.5199442546161117118 ) ) ;
#30532 = CARTESIAN_POINT ( 'NONE',  ( -0.1499999999999996336, 0.000000000000000000, 0.000000000000000000 ) ) ;
#30533 = AXIS2_PLACEMENT_3D ( 'NONE', #10517, #4534, #32925 ) ;
#30534 = CARTESIAN_POINT ( 'NONE',  ( 0.5536297569049346556, -1.186194075236972179, 0.6057417262809815517 ) ) ;
#30535 = AXIS2_PLACEMENT_3D ( 'NONE', #19302, #29156, #6332 ) ;
#30536 = CARTESIAN_POINT ( 'NONE',  ( 0.3882739051659384599, -1.904129335431319570, -0.4886894917023981155 ) ) ;
#30537 = CARTESIAN_POINT ( 'NONE',  ( 0.3200100717190457189, -1.182867460163126827, 0.5426201052292141114 ) ) ;
#30538 = CARTESIAN_POINT ( 'NONE',  ( 0.1874999999999996669, -0.6872203660140441261, 0.1527381444932270627 ) ) ;
#30539 = AXIS2_PLACEMENT_3D ( 'NONE', #18442, #15366, #37366 ) ;
#30540 = PERSON_AND_ORGANIZATION ( #28500, #32463 ) ;
#30541 = AXIS2_PLACEMENT_3D ( 'NONE', #30242, #17512, #14609 ) ;
#30542 = CARTESIAN_POINT ( 'NONE',  ( 0.4795819664771984736, -1.106247336020415917, -0.4111404562665418871 ) ) ;
#30543 = EDGE_CURVE ( 'NONE', #12799, #4767, #4237, .T. ) ;
#30544 = APPLIED_APPROVAL_ASSIGNMENT ( #31049, ( #2940 ) ) ;
#30545 = APPLIED_DATE_AND_TIME_ASSIGNMENT ( #14902, #6243, ( #7563 ) ) ;
#30546 = FACE_OUTER_BOUND ( 'NONE', #4072, .T. ) ;
#30547 = VERTEX_POINT ( 'NONE', #32316 ) ;
#30548 = DIRECTION ( 'NONE',  ( 0.000000000000000000, 0.000000000000000000, -1.000000000000000000 ) ) ;
#30549 = AXIS2_PLACEMENT_3D ( 'NONE', #20571, #14576, #24076 ) ;
#30550 = CARTESIAN_POINT ( 'NONE',  ( 0.8248651029816849167, -1.296087829716116640E-16, -0.6154198107346400271 ) ) ;
#30551 = ORIENTED_EDGE ( 'NONE', *, *, #16734, .F. ) ;
#30552 = FACE_OUTER_BOUND ( 'NONE', #3888, .T. ) ;
#30553 = DIRECTION ( 'NONE',  ( 0.000000000000000000, 0.000000000000000000, 1.000000000000000000 ) ) ;
#30554 = CARTESIAN_POINT ( 'NONE',  ( 0.2245284881113566167, -1.347762582730240855, 0.6028807914139896473 ) ) ;
#30555 = VERTEX_POINT ( 'NONE', #6817 ) ;
#30556 = CARTESIAN_POINT ( 'NONE',  ( 0.1499999999999994671, -0.5346638663566677385, -0.07572681171513533094 ) ) ;
#30557 = CARTESIAN_POINT ( 'NONE',  ( 0.04308558661660993883, 0.05688326490871552232, 0.4910261092774150793 ) ) ;
#30558 = CARTESIAN_POINT ( 'NONE',  ( 0.04230170315644234819, -0.4430127298718438689, -0.1529900842779738368 ) ) ;
#30559 = CARTESIAN_POINT ( 'NONE',  ( 0.3593227136315140791, -1.801274561898448034, -0.3441312665133884896 ) ) ;
#30560 = TOROIDAL_SURFACE ( 'NONE', #35181, 0.08249999999977555842, 0.01000000000000000021 ) ;
#30561 = CARTESIAN_POINT ( 'NONE',  ( 0.4462378990239732057, -1.204432223294487736, 0.6536530620140627024 ) ) ;
#30563 = CARTESIAN_POINT ( 'NONE',  ( 0.1757500541653520820, -1.230771478115229245, -0.2869361388274796476 ) ) ;
#30562 = CARTESIAN_POINT ( 'NONE',  ( 0.04085667396267503998, 0.4547700361314893081, 0.1255037944140956763 ) ) ;
#30564 = FACE_OUTER_BOUND ( 'NONE', #3443, .T. ) ;
#30565 = ORIENTED_EDGE ( 'NONE', *, *, #14108, .T. ) ;
#30566 = ORIENTED_EDGE ( 'NONE', *, *, #36557, .F. ) ;
#30567 = CARTESIAN_POINT ( 'NONE',  ( 0.1665205398182600938, -0.7441302385869247304, 0.6010756574681124231 ) ) ;
#30568 = ORIENTED_EDGE ( 'NONE', *, *, #14080, .F. ) ;
#30569 = EDGE_CURVE ( 'NONE', #32770, #31436, #12123, .T. ) ;
#30570 = DIRECTION ( 'NONE',  ( 0.000000000000000000, 0.000000000000000000, -1.000000000000000000 ) ) ;
#30571 = CARTESIAN_POINT ( 'NONE',  ( 0.4422158392730773380, -1.563691297916808942, 0.6860588747619075223 ) ) ;
#30573 = DIRECTION ( 'NONE',  ( 1.445848444424219201E-15, -1.000000000000000000, -2.361472542561095431E-16 ) ) ;
#30572 = CARTESIAN_POINT ( 'NONE',  ( 0.3334317865496208011, -1.653093244063527090, -0.6440291702909269889 ) ) ;
#30574 = CARTESIAN_POINT ( 'NONE',  ( 0.1499999999999997724, 0.2372406987223678043, 0.4850946823762586901 ) ) ;
#30575 = PRODUCT_DEFINITION_FORMATION_WITH_SPECIFIED_SOURCE ( 'ANY', '', #27234, .NOT_KNOWN. ) ;
#30576 = ORIENTED_EDGE ( 'NONE', *, *, #21435, .T. ) ;
#30577 = ADVANCED_FACE ( 'NONE', ( #31935 ), #37690, .F. ) ;
#30578 = CARTESIAN_POINT ( 'NONE',  ( -0.2300000000000002043, 0.5182417262804744906, 0.08500000000000018652 ) ) ;
#30579 = CARTESIAN_POINT ( 'NONE',  ( 0.3999999999999789280, -2.097675824466503691, -0.4688691127277795356 ) ) ;
#30580 = ADVANCED_FACE ( 'NONE', ( #29251 ), #22284, .T. ) ;
#30581 = CARTESIAN_POINT ( 'NONE',  ( 0.1224514167073170456, -0.5493860373880040671, 0.1534799437718065152 ) ) ;
#30582 = CIRCLE ( 'NONE', #4955, 0.1346589359789737705 ) ;
#30583 = CARTESIAN_POINT ( 'NONE',  ( 0.4788258031900825551, -1.664885640230176600, 0.5089736068239121280 ) ) ;
#30584 = FACE_BOUND ( 'NONE', #25473, .T. ) ;
#30585 = CARTESIAN_POINT ( 'NONE',  ( 0.07216878364870298046, 0.08000000000000023759, -0.1249999999999999029 ) ) ;
#30586 = FACE_OUTER_BOUND ( 'NONE', #16100, .T. ) ;
#30587 = CARTESIAN_POINT ( 'NONE',  ( 0.6367588599008480177, -1.388265895610014233, -0.6250000000000000000 ) ) ;
#30588 = CARTESIAN_POINT ( 'NONE',  ( 0.1840555659586733950, -0.8547793250687044653, 0.1470778270918790542 ) ) ;
#30589 = CARTESIAN_POINT ( 'NONE',  ( 0.4627885704097156050, -1.051432690887019072, 0.8329284434066291931 ) ) ;
#30590 = CARTESIAN_POINT ( 'NONE',  ( -0.05544444631433702309, 0.2873070878496298830, 0.3609075552494527828 ) ) ;
#30591 = EDGE_CURVE ( 'NONE', #7881, #29289, #18981, .T. ) ;
#30592 = CARTESIAN_POINT ( 'NONE',  ( 0.002591829603766808172, -0.9558483906305602629, 0.3895703071142478380 ) ) ;
#30593 = CARTESIAN_POINT ( 'NONE',  ( 0.6050862293119524393, -1.568338382688775567, -0.6158250207463809023 ) ) ;
#30594 = AXIS2_PLACEMENT_3D ( 'NONE', #38619, #22610, #13118 ) ;
#30595 = CARTESIAN_POINT ( 'NONE',  ( 0.4170115945640069932, -1.702980413955156758, -0.6123808887097255127 ) ) ;
#30596 = CARTESIAN_POINT ( 'NONE',  ( -0.2399999999999999079, -2.139295658456680904, -0.2024034539465678073 ) ) ;
#30597 = CARTESIAN_POINT ( 'NONE',  ( -0.2399999999999999079, -2.183180860297908144, -0.4937760292030871079 ) ) ;
#30598 = DIRECTION ( 'NONE',  ( 2.465190328815661892E-32, 1.000000000000000000, 6.656013887802287108E-31 ) ) ;
#30599 = APPROVAL_PERSON_ORGANIZATION ( #23738, #31503, #13517 ) ;
#30600 = ORIENTED_EDGE ( 'NONE', *, *, #16755, .T. ) ;
#30601 = CARTESIAN_POINT ( 'NONE',  ( 0.002083146443013521830, -0.4777046557262296100, 0.1638349238242636507 ) ) ;
#30602 = DIRECTION ( 'NONE',  ( 1.000000000000000000, -0.000000000000000000, -0.000000000000000000 ) ) ;
#30603 = CARTESIAN_POINT ( 'NONE',  ( 0.1700561810475392510, -1.268507724650295154, 0.5481991909815175923 ) ) ;
#30604 = CARTESIAN_POINT ( 'NONE',  ( 0.3657447301641588155, -2.011766955852946293, -0.4876776895119456778 ) ) ;
#30605 = AXIS2_PLACEMENT_3D ( 'NONE', #17025, #442, #13540 ) ;
#30606 = ORIENTED_EDGE ( 'NONE', *, *, #16326, .F. ) ;
#30607 = DIRECTION ( 'NONE',  ( -0.9378410757839559242, -0.2807814858886551468, 0.2039996905746456479 ) ) ;
#30608 = CARTESIAN_POINT ( 'NONE',  ( 0.3832544727030278708, -1.109930869253659580, 0.6055776681277141860 ) ) ;
#30609 = CARTESIAN_POINT ( 'NONE',  ( 0.05999999999999990757, 0.8492681979939306069, -0.2138253033704803907 ) ) ;
#30610 = CARTESIAN_POINT ( 'NONE',  ( -0.05561176441985835051, 0.2871508736821605789, -0.3605511861568530541 ) ) ;
#30611 = CARTESIAN_POINT ( 'NONE',  ( 0.5229569312828943328, -1.333528584511481263, 0.5864232016723698315 ) ) ;
#30613 = ORIENTED_EDGE ( 'NONE', *, *, #35960, .F. ) ;
#30612 = CARTESIAN_POINT ( 'NONE',  ( -0.2399999999999999079, -3.941790907013290823, 0.08058400322088296597 ) ) ;
#30614 = CARTESIAN_POINT ( 'NONE',  ( 0.3243638931714790674, -0.9652511992726795498, 0.5977393664509621507 ) ) ;
#30615 = ORIENTED_EDGE ( 'NONE', *, *, #37884, .T. ) ;
#30616 = DIRECTION ( 'NONE',  ( 0.000000000000000000, -0.3090169943749502823, -0.9510565162951527540 ) ) ;
#30617 = ORIENTED_EDGE ( 'NONE', *, *, #32808, .F. ) ;
#30618 = CARTESIAN_POINT ( 'NONE',  ( -0.02235124290213130402, 0.2417860359143760851, -0.4518977707513310293 ) ) ;
#30619 = EDGE_CURVE ( 'NONE', #11729, #35903, #25152, .T. ) ;
#30620 = ORIENTED_EDGE ( 'NONE', *, *, #8448, .T. ) ;
#30621 = CARTESIAN_POINT ( 'NONE',  ( 0.1808581208431125631, -1.125631630136205930, 0.8751935381423019411 ) ) ;
#30623 = CARTESIAN_POINT ( 'NONE',  ( 0.1872764685775445970, -0.5763073854982146971, 0.01999799437810716521 ) ) ;
#30622 = CARTESIAN_POINT ( 'NONE',  ( 0.06569956760428707909, -0.7774221683014203022, 0.02818812589258910817 ) ) ;
#30624 = CARTESIAN_POINT ( 'NONE',  ( 0.05999999999999990757, 0.000000000000000000, 0.000000000000000000 ) ) ;
#30625 = EDGE_CURVE ( 'NONE', #20043, #10938, #8171, .T. ) ;
#30626 = VERTEX_POINT ( 'NONE', #7028 ) ;
#30627 = VECTOR ( 'NONE', #10142, 39.37007874015748143 ) ;
#30628 = CARTESIAN_POINT ( 'NONE',  ( 0.5261597028464496395, -1.142846293380767264, 0.6481300216459130459 ) ) ;
#30629 = CARTESIAN_POINT ( 'NONE',  ( 0.1162913698539808915, -0.5588670519132078462, 0.2094242198637762120 ) ) ;
#30630 = ORIENTED_EDGE ( 'NONE', *, *, #644, .F. ) ;
#30631 = CARTESIAN_POINT ( 'NONE',  ( 0.1571433491268638127, -1.636854382521477413, -0.3650005568011028823 ) ) ;
#30632 = DIRECTION ( 'NONE',  ( -1.000000000000000000, -7.857794173099924470E-32, -8.628166150854818811E-32 ) ) ;
#30633 = CARTESIAN_POINT ( 'NONE',  ( 0.2262118641390306883, -1.103574613869289234, 0.7477357049086994500 ) ) ;
#30634 = APPROVAL_PERSON_ORGANIZATION ( #6220, #30647, #34192 ) ;
#30635 = CARTESIAN_POINT ( 'NONE',  ( -1.970642109407529655E-05, -2.025638281578344024, -0.3136921261701958730 ) ) ;
#30636 = CARTESIAN_POINT ( 'NONE',  ( -0.1081899703030416854, -0.4934552128794481574, 0.3439540350797968271 ) ) ;
#30637 = B_SPLINE_CURVE_WITH_KNOTS ( 'NONE', 3,
 ( #6826, #13208, #31942, #25779, #3762, #21884, #16315, #10129, #35236, #7037, #37484, #19606, #3942, #16503 ),
 .UNSPECIFIED., .F., .F.,
 ( 4, 2, 2, 2, 2, 2, 4 ),
 ( 0.000000000000000000, 0.0004381064775536402511, 0.0008762129551072805021, 0.001752425910214561004, 0.002190532387768201472, 0.002628638865321841506, 0.003504851820429122009 ),
 .UNSPECIFIED. ) ;
#30638 = CONICAL_SURFACE ( 'NONE', #12899, 0.07506498716826678907, 1.103346454748738825 ) ;
#30639 = CARTESIAN_POINT ( 'NONE',  ( -0.1638630105339158594, 0.5092090815894317890, 0.3148090297061104104 ) ) ;
#30640 = CARTESIAN_POINT ( 'NONE',  ( 0.3055995149173200143, -1.768272766478771185, 0.5197417262808792238 ) ) ;
#30641 =( BOUNDED_SURFACE ( )  B_SPLINE_SURFACE ( 3, 2, ( 
 ( #25361, #15068, #33991 ),
 ( #34184, #18154, #37896 ),
 ( #2723, #9707, #27620 ),
 ( #24545, #5596, #31507 ) ),
 .UNSPECIFIED., .F., .F., .F. ) 
 B_SPLINE_SURFACE_WITH_KNOTS ( ( 4, 4 ),
 ( 3, 3 ),
 ( 0.01439476971272923671, 0.01576594042374710250 ),
 ( 0.4842859667072808572, 1.000000000000000000 ),
 .UNSPECIFIED. ) 
 GEOMETRIC_REPRESENTATION_ITEM ( )  RATIONAL_B_SPLINE_SURFACE ( (
 ( 0.8474955426738830511, 0.8425471025280649728, 1.000000000000000000),
 ( 0.8464882319828066493, 0.8415071067814141603, 1.000000000000000000),
 ( 0.8455725881407269995, 0.8405617522749588844, 1.000000000000000000),
 ( 0.8449979516945560487, 0.8399684701176437507, 1.000000000000000000) ) ) 
 REPRESENTATION_ITEM ( '' )  SURFACE ( )  );
#30642 = DIRECTION ( 'NONE',  ( 0.01455087615875037474, 0.9998941303973200023, 0.000000000000000000 ) ) ;
#30643 = CARTESIAN_POINT ( 'NONE',  ( 0.6527381946072837726, -1.527960125060469299, 0.4182417262808776903 ) ) ;
#30644 = CARTESIAN_POINT ( 'NONE',  ( 0.01632176102313256591, -1.052923364454138255, 0.5995154855756178458 ) ) ;
#30645 = DATE_AND_TIME ( #33716, #8866 ) ;
#30646 = EDGE_CURVE ( 'NONE', #16211, #26211, #28833, .T. ) ;
#30647 = APPROVAL ( #34800, 'UNKNOWN' ) ;
#30648 = ADVANCED_FACE ( 'NONE', ( #305 ), #27750, .T. ) ;
#30649 = CARTESIAN_POINT ( 'NONE',  ( 0.4837052721322094295, -1.131465354378136334, 0.4851784429646056052 ) ) ;
#30650 = CARTESIAN_POINT ( 'NONE',  ( 0.3689410297595501764, -1.154863930213027690, 0.5443150188217301677 ) ) ;
#30651 = CARTESIAN_POINT ( 'NONE',  ( -0.2399999999999999079, -2.393162167644017124, -1.003759557197343888 ) ) ;
#30652 = CARTESIAN_POINT ( 'NONE',  ( 0.0003813859085855243985, -0.4500436584032703746, 0.06912418163519741532 ) ) ;
#30653 = CARTESIAN_POINT ( 'NONE',  ( -0.2043922129835732682, -0.5166151207188712791, 0.08499999999999961753 ) ) ;
#30654 = CARTESIAN_POINT ( 'NONE',  ( -0.2399999999999999079, -2.511040369707300268, -0.4948468226404901804 ) ) ;
#30655 = AXIS2_PLACEMENT_3D ( 'NONE', #1228, #25907, #10865 ) ;
#30656 = CARTESIAN_POINT ( 'NONE',  ( 0.4038347882558627200, -1.728811102478955419, -0.5994564538103192008 ) ) ;
#30657 = ORIENTED_EDGE ( 'NONE', *, *, #3848, .F. ) ;
#30658 = VERTEX_POINT ( 'NONE', #16909 ) ;
#30659 = DIRECTION ( 'NONE',  ( 0.000000000000000000, 0.000000000000000000, -1.000000000000000000 ) ) ;
#30660 = ORIENTED_EDGE ( 'NONE', *, *, #31693, .T. ) ;
#30661 = APPLIED_SECURITY_CLASSIFICATION_ASSIGNMENT ( #11608, ( #40662 ) ) ;
#30662 = DIRECTION ( 'NONE',  ( -1.000000000000000000, 0.000000000000000000, 0.000000000000000000 ) ) ;
#30663 = DIRECTION ( 'NONE',  ( -0.5000000000000003331, -0.6415696268731877483, -0.5817116243241130524 ) ) ;
#30665 = ORIENTED_EDGE ( 'NONE', *, *, #31414, .T. ) ;
#30664 = CARTESIAN_POINT ( 'NONE',  ( 0.001740155361229381867, -0.5357720371266511128, 0.07346349438433615042 ) ) ;
#30666 = CIRCLE ( 'NONE', #8988, 0.1599999999999999201 ) ;
#30667 = ORIENTED_EDGE ( 'NONE', *, *, #32769, .T. ) ;
#30668 = CYLINDRICAL_SURFACE ( 'NONE', #33025, 0.5400000000000012568 ) ;
#30669 = ORIENTED_EDGE ( 'NONE', *, *, #3120, .F. ) ;
#30670 = CARTESIAN_POINT ( 'NONE',  ( -0.0004184392737591126517, -0.5575462098935206612, 0.2717930660292434131 ) ) ;
#30672 = CARTESIAN_POINT ( 'NONE',  ( 0.1118412691610174287, -1.266776148485620146, 0.6017280176731151231 ) ) ;
#30671 = CARTESIAN_POINT ( 'NONE',  ( 0.1655461965905788702, -0.9040591713125657458, 0.5924644706352264478 ) ) ;
#30673 = CARTESIAN_POINT ( 'NONE',  ( -0.2746410161513776482, -4.289222312108804225, -0.5708809693675255259 ) ) ;
#30674 = PERSON_AND_ORGANIZATION_ROLE ( 'classification_officer' ) ;
#30675 = EDGE_CURVE ( 'NONE', #11923, #36916, #18700, .T. ) ;
#30676 = CARTESIAN_POINT ( 'NONE',  ( 0.5922249234364754811, -1.371803823430798541, -0.6250000000000000000 ) ) ;
#30678 = ORIENTED_EDGE ( 'NONE', *, *, #26156, .F. ) ;
#30677 = ORIENTED_EDGE ( 'NONE', *, *, #39561, .T. ) ;
#30679 = EDGE_CURVE ( 'NONE', #34841, #30067, #27282, .T. ) ;
#30680 = CARTESIAN_POINT ( 'NONE',  ( 0.3204479958614548929, -1.182666560659948907, 0.5682417262808776570 ) ) ;
#30681 = CARTESIAN_POINT ( 'NONE',  ( 0.4183584374824474428, -1.737746862795950697, -0.4437617475756700514 ) ) ;
#30682 = CARTESIAN_POINT ( 'NONE',  ( -0.04211471441534140464, -0.4486586774158462521, 0.1367340165256737128 ) ) ;
#30683 = CARTESIAN_POINT ( 'NONE',  ( 0.4749030200414927627, -1.260576499757741553, 0.8114222651001881115 ) ) ;
#30684 = CARTESIAN_POINT ( 'NONE',  ( 0.01508763455763984483, -0.9705204025707556692, 0.4143134863502723197 ) ) ;
#30685 = CARTESIAN_POINT ( 'NONE',  ( 0.4751248519516730884, -1.681100737592190031, 0.5628962907142390781 ) ) ;
#30686 = CARTESIAN_POINT ( 'NONE',  ( 0.1696489863018690591, -1.274013792877867646, 0.9327432631391745499 ) ) ;
#30687 = DIRECTION ( 'NONE',  ( 7.771561172376107616E-16, -7.170354002788761615E-17, 1.000000000000000000 ) ) ;
#30688 = CARTESIAN_POINT ( 'NONE',  ( 0.3999835757944618098, -1.598096088517039437, -0.3114834528418581883 ) ) ;
#30689 = AXIS2_PLACEMENT_3D ( 'NONE', #2367, #39989, #11810 ) ;
#30690 = CARTESIAN_POINT ( 'NONE',  ( 0.3419910132069426956, -1.631574105539462360, -0.5957206493232616307 ) ) ;
#30691 = CARTESIAN_POINT ( 'NONE',  ( 1.480025787077754007, -0.6872203660140440151, 0.1457185332388702959 ) ) ;
#30692 = CARTESIAN_POINT ( 'NONE',  ( 0.3912168351225406848, -1.712565751828606153, 0.4687417262808791230 ) ) ;
#30693 = CARTESIAN_POINT ( 'NONE',  ( 0.4643862794852260945, -1.116283308840022803, 0.5648439556958982921 ) ) ;
#30694 = CARTESIAN_POINT ( 'NONE',  ( 0.3841588946375145142, -1.652860766595878772, -0.3962426122320574229 ) ) ;
#30695 = DIRECTION ( 'NONE',  ( -0.5000000000000000000, 3.759415251443887013E-31, 0.8660254037844384856 ) ) ;
#30696 = CARTESIAN_POINT ( 'NONE',  ( 0.2518326032030922534, -1.639413698222365046, 0.7148483533190357342 ) ) ;
#30697 = CARTESIAN_POINT ( 'NONE',  ( 0.07414496827190548978, -1.147132939374254423, 0.7606844393218312739 ) ) ;
#30698 = APPROVAL_DATE_TIME ( #40554, #29513 ) ;
#30699 = CARTESIAN_POINT ( 'NONE',  ( 0.6930531720067659718, -1.422936651082730375, 0.7544454077531311809 ) ) ;
#30700 = ADVANCED_FACE ( 'NONE', ( #26366 ), #36216, .F. ) ;
#30701 = CARTESIAN_POINT ( 'NONE',  ( 0.6653925203977772984, -1.561488534969799113, 0.6071316550003039714 ) ) ;
#30702 = CARTESIAN_POINT ( 'NONE',  ( 0.02872242845530412203, -0.07817994906156924828, -0.5268390348591153183 ) ) ;
#30703 = CARTESIAN_POINT ( 'NONE',  ( 0.3453005398490904820, -1.702161746735940895, -0.4206499346865002487 ) ) ;
#30704 = ORIENTED_EDGE ( 'NONE', *, *, #34778, .T. ) ;
#30705 = LINE ( 'NONE', #33783, #29626 ) ;
#30706 = CARTESIAN_POINT ( 'NONE',  ( 0.03846717227426538904, -0.7578942448716873281, 0.6192360675337290621 ) ) ;
#30707 = CARTESIAN_POINT ( 'NONE',  ( 0.5182826642499327452, -1.390450437559696217, 0.7925567997242233265 ) ) ;
#30709 = VERTEX_POINT ( 'NONE', #10728 ) ;
#30708 = DIRECTION ( 'NONE',  ( 0.9378410757839557021, -0.1072489841977670583, 0.3300784330442384507 ) ) ;
#30710 = CARTESIAN_POINT ( 'NONE',  ( 0.6014934134068773419, -1.267756190114700976, 0.6768762346975223387 ) ) ;
#30712 = ORIENTED_EDGE ( 'NONE', *, *, #34699, .F. ) ;
#30711 = ORIENTED_EDGE ( 'NONE', *, *, #6623, .T. ) ;
#30713 = CARTESIAN_POINT ( 'NONE',  ( 0.2821966830767973500, -0.7863026750338284465, 0.6043004553601608597 ) ) ;
#30714 = FACE_OUTER_BOUND ( 'NONE', #15790, .T. ) ;
#30715 = CARTESIAN_POINT ( 'NONE',  ( 0.2704658693197408703, -1.170736166911837683, -0.5155029497116575543 ) ) ;
#30716 = DATE_AND_TIME ( #39547, #1765 ) ;
#30717 = B_SPLINE_CURVE_WITH_KNOTS ( 'NONE', 3,
 ( #33419, #7902, #14484, #23578, #27054, #36292, #39583, #20473, #36097, #14298 ),
 .UNSPECIFIED., .F., .F.,
 ( 4, 2, 2, 2, 4 ),
 ( 0.003098629625065147525, 0.003873295706325722860, 0.004647961787586298195, 0.005422627868846873964, 0.006197293950107448865 ),
 .UNSPECIFIED. ) ;
#30718 = CARTESIAN_POINT ( 'NONE',  ( -0.01548846960707524721, 0.000000000000000000, 0.000000000000000000 ) ) ;
#30719 = ORIENTED_EDGE ( 'NONE', *, *, #24094, .F. ) ;
#30720 = CARTESIAN_POINT ( 'NONE',  ( 0.08707804302881141933, -0.7047988938172153883, 0.1683407647532852991 ) ) ;
#30721 = CARTESIAN_POINT ( 'NONE',  ( 0.3158115486623674362, -1.764399868795166304, 0.6580999141868399960 ) ) ;
#30722 = CARTESIAN_POINT ( 'NONE',  ( 0.4982596037652018972, -1.542515356531135584, 0.5876215343849920947 ) ) ;
#30724 = CARTESIAN_POINT ( 'NONE',  ( 0.001618903166729741003, -0.5421073043963201554, 0.06143527706437781205 ) ) ;
#30723 = CARTESIAN_POINT ( 'NONE',  ( 0.01548846960707524721, 0.000000000000000000, 0.000000000000000000 ) ) ;
#30725 = CARTESIAN_POINT ( 'NONE',  ( -0.02953079040095693900, -0.3810518745593846068, 0.3687679460475796756 ) ) ;
#30726 = VERTEX_POINT ( 'NONE', #7639 ) ;
#30727 = ORIENTED_EDGE ( 'NONE', *, *, #1364, .T. ) ;
#30728 = CARTESIAN_POINT ( 'NONE',  ( 0.05634307799789356475, -0.4395998308137145094, -0.1320249839696048810 ) ) ;
#30729 = CARTESIAN_POINT ( 'NONE',  ( 0.3967733525505006686, -1.041653198288154725, 0.8729704400460266411 ) ) ;
#30730 = LINE ( 'NONE', #39782, #40395 ) ;
#30731 = CARTESIAN_POINT ( 'NONE',  ( 0.3690018924180193394, -2.059894194155437397, -0.5029151679812257081 ) ) ;
#30732 = DIRECTION ( 'NONE',  ( 0.000000000000000000, 0.5877852522924520429, 0.8090169943749627723 ) ) ;
#30733 = CARTESIAN_POINT ( 'NONE',  ( 0.2923286432308245808, -1.660243258845594649, -0.6250000000000000000 ) ) ;
#30734 = DIRECTION ( 'NONE',  ( -1.000000000000000000, -7.857794173099924470E-32, -8.628166150854818811E-32 ) ) ;
#30735 = CARTESIAN_POINT ( 'NONE',  ( 0.3169982175285875337, -1.184547601087671875, 0.5195431689978142753 ) ) ;
#30736 = CARTESIAN_POINT ( 'NONE',  ( 0.4926052497631904226, -1.101322287461897975, 0.6863075852112333619 ) ) ;
#30737 = B_SPLINE_SURFACE_WITH_KNOTS ( 'NONE', 5, 5, ( 
 ( #28800, #261, #12758, #25319, #16058, #37860 ),
 ( #9674, #22243, #25714, #28603, #38245, #6984 ),
 ( #854, #40012, #11835, #26690, #24395, #7738 ),
 ( #20302, #14117, #36318, #11647, #20919, #33245 ),
 ( #1591, #30160, #33439, #32822, #5247, #26878 ),
 ( #4628, #24206, #39608, #27295, #14319, #17202 ) ),
 .UNSPECIFIED., .F., .F., .F.,
 ( 6, 6 ),
 ( 6, 6 ),
 ( -5.904618948009931145, 5.904618948009923152 ),
 ( -4.007879036389231153, 1.896739911619200303 ),
 .UNSPECIFIED. ) ;
#30738 = PERSON_AND_ORGANIZATION_ROLE ( 'design_owner' ) ;
#30739 = CARTESIAN_POINT ( 'NONE',  ( 0.3546447787406709629, -1.846711228588695075, -0.5131486097874190522 ) ) ;
#30740 = CARTESIAN_POINT ( 'NONE',  ( 0.3699999999999784572, -2.087572556818563907, -0.5179767974037823297 ) ) ;
#30741 = CARTESIAN_POINT ( 'NONE',  ( 0.6077786581711973612, -1.479275016670621667, 0.5594553644565639638 ) ) ;
#30742 = AXIS2_PLACEMENT_3D ( 'NONE', #40015, #25207, #27491 ) ;
#30743 = CARTESIAN_POINT ( 'NONE',  ( -0.01548846960707477016, 0.5198120922912068398, -0.07362328916748536733 ) ) ;
#30744 = ORIENTED_EDGE ( 'NONE', *, *, #10242, .T. ) ;
#30745 = CARTESIAN_POINT ( 'NONE',  ( 0.4215912490580301930, -1.142508127983099309, 0.4283266193199111727 ) ) ;
#30746 = CARTESIAN_POINT ( 'NONE',  ( -0.02881329448201542381, -0.2420398234037506313, 0.4354480552436106322 ) ) ;
#30747 = LINE ( 'NONE', #8523, #17352 ) ;
#30748 = ORIENTED_EDGE ( 'NONE', *, *, #27341, .T. ) ;
#30749 = CARTESIAN_POINT ( 'NONE',  ( -0.05186792262757321942, 0.01796889665935373290, -0.4704835727131216339 ) ) ;
#30750 = EDGE_CURVE ( 'NONE', #8991, #22855, #23507, .T. ) ;
#30751 = CARTESIAN_POINT ( 'NONE',  ( 0.01476761613299030704, -0.8638487819985384286, 0.3976658538871967741 ) ) ;
#30753 = VERTEX_POINT ( 'NONE', #14008 ) ;
#30752 = ORIENTED_EDGE ( 'NONE', *, *, #40586, .T. ) ;
#30754 = DIRECTION ( 'NONE',  ( -1.000000000000000000, -2.280301054154495132E-31, 1.664003471950577689E-31 ) ) ;
#30755 = DIRECTION ( 'NONE',  ( 0.000000000000000000, 3.330669073875470114E-16, 1.000000000000000000 ) ) ;
#30756 = CARTESIAN_POINT ( 'NONE',  ( 0.7412791958894395794, -1.507305061506947430, 0.6536223584324379887 ) ) ;
#30757 = CARTESIAN_POINT ( 'NONE',  ( 0.3690052979743954076, -2.042003302564155298, -0.3074372596445509864 ) ) ;
#30758 = CARTESIAN_POINT ( 'NONE',  ( 0.4591678779736387273, -1.223483637120778011, 0.6328851562681094833 ) ) ;
#30759 = CARTESIAN_POINT ( 'NONE',  ( 0.2085781299520444998, -1.361703007109797525, 0.5547567937505603064 ) ) ;
#30760 = CARTESIAN_POINT ( 'NONE',  ( 0.03474878377840979332, -0.3591457335720762423, -0.3712550153170212641 ) ) ;
#30761 = ORIENTED_EDGE ( 'NONE', *, *, #35859, .F. ) ;
#30762 = ORIENTED_EDGE ( 'NONE', *, *, #10628, .F. ) ;
#30763 = CARTESIAN_POINT ( 'NONE',  ( 0.1266021694322588542, -1.239399129679921829, 0.5182417262812423209 ) ) ;
#30764 = ORIENTED_EDGE ( 'NONE', *, *, #14964, .F. ) ;
#30765 = CARTESIAN_POINT ( 'NONE',  ( 0.1424029337235096226, -1.400533250147911746, -0.6250000000000000000 ) ) ;
#30766 = CARTESIAN_POINT ( 'NONE',  ( 0.3497955937797163073, -1.368691204837882980, 0.8715010437854141534 ) ) ;
#30767 = EDGE_CURVE ( 'NONE', #21571, #7737, #29892, .T. ) ;
#30769 = CARTESIAN_POINT ( 'NONE',  ( 0.5672950941327136176, -1.626571888027773527, 0.5062501768905920407 ) ) ;
#30768 = CARTESIAN_POINT ( 'NONE',  ( 0.3433846349558144495, -1.636536893579917162, -0.6541055532972044340 ) ) ;
#30770 = DIRECTION ( 'NONE',  ( 0.000000000000000000, 0.000000000000000000, -1.000000000000000000 ) ) ;
#30771 = CARTESIAN_POINT ( 'NONE',  ( 0.7059656540691131577, -1.571716619208481935, -0.5155029497116575543 ) ) ;
#30772 = PRODUCT_RELATED_PRODUCT_CATEGORY ( 'detail', '', ( #14383 ) ) ;
#30773 = ORIENTED_EDGE ( 'NONE', *, *, #37884, .F. ) ;
#30774 = CARTESIAN_POINT ( 'NONE',  ( 0.4634712904840415093, -1.711704060178988129, -0.5155029497116575543 ) ) ;
#30775 = CARTESIAN_POINT ( 'NONE',  ( 0.3939041149941049924, -1.772452426391821989, -0.3123449749659221730 ) ) ;
#30776 = CARTESIAN_POINT ( 'NONE',  ( 0.1223607623319934723, -0.5629964153041870922, 0.2193006277981656427 ) ) ;
#30777 = CARTESIAN_POINT ( 'NONE',  ( 0.4226000438817392180, -1.709616762427841996, 0.4282184315516495143 ) ) ;
#30778 = CARTESIAN_POINT ( 'NONE',  ( 1.171686751969803217E-18, -0.2899999999999993694, 0.01749999999999931818 ) ) ;
#30779 = EDGE_LOOP ( 'NONE', ( #26964, #28309, #28420, #12146, #2980 ) ) ;
#30780 = DIRECTION ( 'NONE',  ( -1.000000000000000000, -2.280301054154495132E-31, 1.664003471950577689E-31 ) ) ;
#30781 = CARTESIAN_POINT ( 'NONE',  ( -0.1399999999999997358, 0.000000000000000000, 0.000000000000000000 ) ) ;
#30782 = CARTESIAN_POINT ( 'NONE',  ( 0.05999999999999990757, -0.4415087982045245996, -0.1343585914930097158 ) ) ;
#30783 = CARTESIAN_POINT ( 'NONE',  ( 0.1840595033465176056, -0.8547675690073376353, 0.1457166466292989515 ) ) ;
#30784 = CARTESIAN_POINT ( 'NONE',  ( 0.1900797982425219412, -0.5100199057060679220, 0.2041009711615301980 ) ) ;
#30785 = CARTESIAN_POINT ( 'NONE',  ( -0.04308449196698682648, 0.2425978208598493779, 0.4306872647601522885 ) ) ;
#30786 = CARTESIAN_POINT ( 'NONE',  ( 0.0003691823678324147721, -0.9420571173525413844, 0.2855820445452574852 ) ) ;
#30787 = B_SPLINE_CURVE_WITH_KNOTS ( 'NONE', 3,
 ( #19370, #9691, #24924, #16078, #25124 ),
 .UNSPECIFIED., .F., .F.,
 ( 4, 1, 4 ),
 ( 0.1498428223741591070, 0.2500000000004219403, 0.3316920714935439052 ),
 .UNSPECIFIED. ) ;
#30788 = CARTESIAN_POINT ( 'NONE',  ( 0.6412004512100059062, -1.451677482400071773, -0.3985001959979381780 ) ) ;
#30789 = CARTESIAN_POINT ( 'NONE',  ( 0.02996954754363531648, -2.053999617283090995, -0.7135042156891373555 ) ) ;
#30790 = ADVANCED_FACE ( 'NONE', ( #8031 ), #8243, .F. ) ;
#30791 = CARTESIAN_POINT ( 'NONE',  ( 0.6254352837214305350, -1.595686027468073753, 0.6076023449066322302 ) ) ;
#30792 = CARTESIAN_POINT ( 'NONE',  ( -0.3000000000000000999, -1.804235510932644004, -0.1501860188971498311 ) ) ;
#30793 = DIRECTION ( 'NONE',  ( 0.000000000000000000, 0.000000000000000000, 1.000000000000000000 ) ) ;
#30794 = EDGE_CURVE ( 'NONE', #24301, #28660, #7519, .T. ) ;
#30795 = ORIENTED_EDGE ( 'NONE', *, *, #24012, .F. ) ;
#30796 = CARTESIAN_POINT ( 'NONE',  ( -0.05464101615137761936, -1.984114763688379579, -0.7731012124309359912 ) ) ;
#30797 = CARTESIAN_POINT ( 'NONE',  ( 0.4150350604501116814, -1.704167521295949284, -0.6115272160904526855 ) ) ;
#30798 = ADVANCED_FACE ( 'NONE', ( #14406 ), #26968, .F. ) ;
#30799 = CARTESIAN_POINT ( 'NONE',  ( 0.1825980849618502877, -1.261391773294454399, 0.5182417262812422099 ) ) ;
#30800 = LINE ( 'NONE', #24648, #1604 ) ;
#30801 = ADVANCED_FACE ( 'NONE', ( #39118 ), #39931, .T. ) ;
#30802 = EDGE_LOOP ( 'NONE', ( #34030, #33917 ) ) ;
#30803 = CARTESIAN_POINT ( 'NONE',  ( 0.5008138289901331586, -1.674651764118539443, -0.6059811472733124260 ) ) ;
#30804 = CARTESIAN_POINT ( 'NONE',  ( 0.3713765372429593259, -1.116629982321883041, 0.6056053568277999233 ) ) ;
#30805 = DIRECTION ( 'NONE',  ( 0.000000000000000000, 0.000000000000000000, 1.000000000000000000 ) ) ;
#30806 = CARTESIAN_POINT ( 'NONE',  ( 0.03674078017396244927, 0.3145504785376027068, -0.3636064179578474276 ) ) ;
#30807 = CARTESIAN_POINT ( 'NONE',  ( 0.5305547748358091509, -1.344461649844473694, 0.6320627015115972691 ) ) ;
#30809 = ORIENTED_EDGE ( 'NONE', *, *, #10810, .F. ) ;
#30808 = DIRECTION ( 'NONE',  ( 0.000000000000000000, 9.106159978880816258E-16, -1.000000000000000000 ) ) ;
#30810 = CARTESIAN_POINT ( 'NONE',  ( 0.2803482358567763177, -0.9348470554797825294, 0.5439829518127811125 ) ) ;
#30811 = ORIENTED_EDGE ( 'NONE', *, *, #35622, .T. ) ;
#30812 = SHAPE_DEFINITION_REPRESENTATION ( #22937, #8026 ) ;
#30813 = FACE_OUTER_BOUND ( 'NONE', #30156, .T. ) ;
#30814 = ORIENTED_EDGE ( 'NONE', *, *, #13186, .T. ) ;
#30815 = CARTESIAN_POINT ( 'NONE',  ( 0.009682433437374710072, -0.5618920970707950158, 0.04941970624388019456 ) ) ;
#30816 = ORIENTED_EDGE ( 'NONE', *, *, #35622, .F. ) ;
#30817 = CARTESIAN_POINT ( 'NONE',  ( 0.2894994844286561952, -1.428162831126878141, 0.8955990884091332704 ) ) ;
#30818 = EDGE_CURVE ( 'NONE', #30159, #17702, #15444, .T. ) ;
#30820 = CARTESIAN_POINT ( 'NONE',  ( 0.1126304012248214304, -0.7661081300572403219, -0.08267986882272944371 ) ) ;
#30819 = DIRECTION ( 'NONE',  ( -0.0001066307966867950538, 1.551735798909011778E-06, 0.9999999943137325431 ) ) ;
#30821 = CARTESIAN_POINT ( 'NONE',  ( -0.2746410161513779258, -1.730153431576819445, -0.08301574631829780615 ) ) ;
#30822 = ORIENTED_EDGE ( 'NONE', *, *, #21576, .F. ) ;
#30823 = ORIENTED_EDGE ( 'NONE', *, *, #38890, .F. ) ;
#30824 = CARTESIAN_POINT ( 'NONE',  ( 0.3822464718857132571, -1.102226274216854263, 0.6317401270923076462 ) ) ;
#30825 = CARTESIAN_POINT ( 'NONE',  ( 0.1162134951484129625, -0.5489498940799030224, 0.1618951865093009590 ) ) ;
#30826 = ORIENTED_EDGE ( 'NONE', *, *, #32898, .F. ) ;
#30827 = CARTESIAN_POINT ( 'NONE',  ( 0.4311422992558763267, -1.610538320350847208, -0.3671492683199031881 ) ) ;
#30828 = CARTESIAN_POINT ( 'NONE',  ( -0.1795773455677812658, 0.4580325878418074481, 0.09550516381870167992 ) ) ;
#30829 = CARTESIAN_POINT ( 'NONE',  ( 0.5913314978914147035, -1.514214781277106736, -0.3979390557995906019 ) ) ;
#30830 = CARTESIAN_POINT ( 'NONE',  ( -0.1212602504878774051, -0.5073146173917495450, 0.3032895567580812246 ) ) ;
#30831 = CARTESIAN_POINT ( 'NONE',  ( 0.4257622994621999557, -1.693842739163180289, 0.4182417262808084124 ) ) ;
#30832 = CARTESIAN_POINT ( 'NONE',  ( 0.7471901070607220863, -1.513130089782565468, 0.5197417262808792238 ) ) ;
#30833 = DIRECTION ( 'NONE',  ( 0.4999551463232372317, -0.8660512985181135770, 0.000000000000000000 ) ) ;
#30834 = DIRECTION ( 'NONE',  ( -0.8660254037844390407, 0.4259456949666814429, 0.2618592464270647624 ) ) ;
#30835 = CARTESIAN_POINT ( 'NONE',  ( 0.004725042054567132541, -0.9785087964782590575, 0.4373990939698282343 ) ) ;
#30836 = DATE_AND_TIME ( #15198, #24654 ) ;
#30837 = CARTESIAN_POINT ( 'NONE',  ( 0.4873057611341404805, -1.123973904486345932, 0.5217046469155847133 ) ) ;
#30838 = CARTESIAN_POINT ( 'NONE',  ( 0.4545629988304267788, -1.243546925348286036, 0.6057417262809815517 ) ) ;
#30839 = CARTESIAN_POINT ( 'NONE',  ( -0.02953079040095700838, 0.000000000000000000, 0.000000000000000000 ) ) ;
#30840 = EDGE_CURVE ( 'NONE', #23694, #24904, #30245, .T. ) ;
#30841 = CARTESIAN_POINT ( 'NONE',  ( 0.05825416142610396336, -1.237506905460590723, 0.6972702062804553291 ) ) ;
#30842 = CARTESIAN_POINT ( 'NONE',  ( 0.08978098643734198914, -7.789101598130623152E-17, -0.3698489655878005045 ) ) ;
#30843 = EDGE_CURVE ( 'NONE', #8621, #2786, #35148, .T. ) ;
#30844 = CARTESIAN_POINT ( 'NONE',  ( 0.02309053091563895849, -0.6171704500300686513, 0.5838629695588271051 ) ) ;
#30845 = CARTESIAN_POINT ( 'NONE',  ( 0.1843722651776505406, -1.260849697819215631, -0.2901536752075735692 ) ) ;
#30846 = EDGE_CURVE ( 'NONE', #5340, #5797, #30863, .T. ) ;
#30847 = ORIENTED_EDGE ( 'NONE', *, *, #10741, .T. ) ;
#30848 = EDGE_LOOP ( 'NONE', ( #3921, #34132, #8036 ) ) ;
#30849 = CARTESIAN_POINT ( 'NONE',  ( -0.2343922129835731283, -0.5166151207188712791, 0.3750000000000000555 ) ) ;
#30850 = ORIENTED_EDGE ( 'NONE', *, *, #17808, .T. ) ;
#30851 = ADVANCED_FACE ( 'NONE', ( #37246, #8441 ), #18321, .F. ) ;
#30852 = CARTESIAN_POINT ( 'NONE',  ( -0.3000000000000000999, -3.849534981189179028, -0.1910928155360645808 ) ) ;
#30853 = CARTESIAN_POINT ( 'NONE',  ( -0.01548846960707386464, -0.07651041855118967394, -0.5222379212568238893 ) ) ;
#30855 = ORIENTED_EDGE ( 'NONE', *, *, #3448, .F. ) ;
#30854 = CARTESIAN_POINT ( 'NONE',  ( 0.001701916547476807961, -0.5482314149877699494, 0.06752930009528983202 ) ) ;
#30856 = VERTEX_POINT ( 'NONE', #24501 ) ;
#30857 = FACE_OUTER_BOUND ( 'NONE', #17404, .T. ) ;
#30858 = ORIENTED_EDGE ( 'NONE', *, *, #26256, .F. ) ;
#30859 = EDGE_CURVE ( 'NONE', #6171, #16949, #37642, .T. ) ;
#30860 = CARTESIAN_POINT ( 'NONE',  ( 0.2666310949013298015, -1.675413163925608240, 0.5768915532334314422 ) ) ;
#30862 = CARTESIAN_POINT ( 'NONE',  ( 0.08672459768460706597, -1.302515868427265078, 0.5757131974872962132 ) ) ;
#30861 = CARTESIAN_POINT ( 'NONE',  ( 0.2318711984724983466, -0.9643490876729370331, 0.6839831110571921169 ) ) ;
#30863 = LINE ( 'NONE', #36637, #40393 ) ;
#30864 = EDGE_CURVE ( 'NONE', #5281, #27329, #27316, .T. ) ;
#30865 = ITEM_DEFINED_TRANSFORMATION ( 'NONE', 'NONE', #29189,  #27819 ) ;
#30866 = CARTESIAN_POINT ( 'NONE',  ( -0.2399999999999999079, -1.948886540192243055, -0.2806949125330161499 ) ) ;
#30867 = B_SPLINE_CURVE_WITH_KNOTS ( 'NONE', 3,
 ( #26317, #30013, #32685, #29406, #20765, #20553 ),
 .UNSPECIFIED., .F., .F.,
 ( 4, 2, 4 ),
 ( 0.000000000000000000, 0.0007708994731598440078, 0.001541798946319688016 ),
 .UNSPECIFIED. ) ;
#30869 = ORIENTED_EDGE ( 'NONE', *, *, #37116, .T. ) ;
#30868 = ORIENTED_EDGE ( 'NONE', *, *, #18433, .F. ) ;
#30870 = EDGE_CURVE ( 'NONE', #24980, #14090, #5763, .T. ) ;
#30871 = CARTESIAN_POINT ( 'NONE',  ( 0.01167908229743947097, -0.7459992564288900896, -0.1065741914396502593 ) ) ;
#30872 = DIRECTION ( 'NONE',  ( -1.000000000000000000, -0.000000000000000000, -0.000000000000000000 ) ) ;
#30873 = CARTESIAN_POINT ( 'NONE',  ( -0.05544444631433556592, -0.4320262549500628046, 0.1617187101067735222 ) ) ;
#30874 = CARTESIAN_POINT ( 'NONE',  ( 0.4660932482496507046, -1.246255835518915056, 0.7959364137991218335 ) ) ;
#30875 =( BOUNDED_SURFACE ( )  B_SPLINE_SURFACE ( 3, 2, ( 
 ( #6951, #633, #38625 ),
 ( #28957, #26495, #32659 ),
 ( #39030, #821, #26114 ),
 ( #16839, #13332, #32237 ),
 ( #4057, #4464, #16624 ),
 ( #25905, #38423, #29571 ),
 ( #22407, #29171, #1034 ),
 ( #23010, #13544, #35531 ),
 ( #7333, #19911, #32448 ),
 ( #1225, #39241, #30180 ),
 ( #23436, #5472, #2215 ),
 ( #30593, #2417, #14954 ),
 ( #27508, #10862, #14536 ),
 ( #17224, #39432, #14755 ),
 ( #36748, #8559, #18037 ),
 ( #7949, #23824, #30384 ),
 ( #26901, #21131, #20523 ),
 ( #17825, #33057, #36346 ),
 ( #4865, #26711, #8163 ),
 ( #35952, #29776, #11254 ),
 ( #7759, #27100, #24224 ),
 ( #20740, #33264, #11469 ),
 ( #27317, #5073, #17633 ),
 ( #2010, #39634, #33659 ),
 ( #24033, #17433, #4652 ),
 ( #14139, #1617, #20326 ),
 ( #11063, #36562, #39846 ),
 ( #8367, #32848, #23623 ),
 ( #20936, #33458, #36139 ),
 ( #5265, #11668, #29989 ),
 ( #1822, #14338, #25019 ),
 ( #33887, #9171, #31405 ),
 ( #21736, #27705, #11857 ),
 ( #172, #19056, #15752 ),
 ( #27916, #15570, #12661 ),
 ( #6486, #3409, #3025 ),
 ( #31594, #8772, #40238 ),
 ( #40455, #24422, #34681 ),
 ( #9589, #34270, #37769 ),
 ( #5689, #15965, #25226 ),
 ( #18243, #3208, #37550 ),
 ( #12074, #22168, #40032 ),
 ( #36954, #37168, #12280 ),
 ( #18434, #15358, #21349 ),
 ( #24837, #6293, #8984 ),
 ( #18647, #21552, #15145 ),
 ( #30788, #2609, #24637 ),
 ( #34071, #5872, #28117 ) ),
 .UNSPECIFIED., .F., .F., .T. ) 
 B_SPLINE_SURFACE_WITH_KNOTS ( ( 4, 2, 2, 2, 2, 2, 2, 2, 2, 2, 2, 2, 2, 2, 2, 2, 2, 2, 2, 2, 2, 2, 2, 4 ),
 ( 3, 3 ),
 ( 0.003261766200971520820, 0.004250769295497201089, 0.005239772390022882226, 0.006228775484548562495, 0.007217778579074242765, 0.008206781673599922167, 0.008701283220862762735, 0.009195784768125603303, 0.009690286315388443872, 0.01018478786265128444, 0.01067928940991412501, 0.01117379095717696384, 0.01166829250443980268, 0.01216279405170264324, 0.01265729559896548381, 0.01315179714622832438, 0.01364629869349116495, 0.01414080024075400552, 0.01463530178801684609, 0.01512980333527968665, 0.01611880642980536432, 0.01710780952433104546, 0.01809681261885672660, 0.01908581571338240773 ),
 ( 0.000000000000000000, 1.000000000000000000 ),
 .UNSPECIFIED. ) 
 GEOMETRIC_REPRESENTATION_ITEM ( )  RATIONAL_B_SPLINE_SURFACE ( (
 ( 1.000000000000000000, 0.9336557140612112837, 1.000000000000000000),
 ( 1.000000000000000000, 0.9269669748511076834, 1.000000000000000000),
 ( 1.000000000000000000, 0.9185057473876691025, 1.000000000000000000),
 ( 1.000000000000000000, 0.8983811411394780899, 1.000000000000000000),
 ( 1.000000000000000000, 0.8868705803443834856, 1.000000000000000000),
 ( 1.000000000000000000, 0.8615685732449787082, 1.000000000000000000),
 ( 1.000000000000000000, 0.8476166942854144182, 1.000000000000000000),
 ( 1.000000000000000000, 0.8180751618708101969, 1.000000000000000000),
 ( 1.000000000000000000, 0.8026452689216959646, 1.000000000000000000),
 ( 1.000000000000000000, 0.7711474197545707954, 1.000000000000000000),
 ( 1.000000000000000000, 0.7550167180304484527, 1.000000000000000000),
 ( 1.000000000000000000, 0.7326795836945654283, 1.000000000000000000),
 ( 1.000000000000000000, 0.7254988216173606785, 1.000000000000000000),
 ( 1.000000000000000000, 0.7120213782890315590, 1.000000000000000000),
 ( 1.000000000000000000, 0.7058095999174238688, 1.000000000000000000),
 ( 1.000000000000000000, 0.6951287496146589806, 1.000000000000000000),
 ( 1.000000000000000000, 0.6906111284772815662, 1.000000000000000000),
 ( 1.000000000000000000, 0.6837693063777301461, 1.000000000000000000),
 ( 1.000000000000000000, 0.6814518707835520717, 1.000000000000000000),
 ( 1.000000000000000000, 0.6797285044136155419, 1.000000000000000000),
 ( 1.000000000000000000, 0.6803227108142706481, 1.000000000000000000),
 ( 1.000000000000000000, 0.6840260012167642678, 1.000000000000000000),
 ( 1.000000000000000000, 0.6872325378123951278, 1.000000000000000000),
 ( 1.000000000000000000, 0.6934257698760888378, 1.000000000000000000),
 ( 1.000000000000000000, 0.6961673821949488916, 1.000000000000000000),
 ( 1.000000000000000000, 0.6971230725348070978, 1.000000000000000000),
 ( 1.000000000000000000, 0.6952258568012568141, 1.000000000000000000),
 ( 1.000000000000000000, 0.6895613480052964483, 1.000000000000000000),
 ( 1.000000000000000000, 0.6860771389999574810, 1.000000000000000000),
 ( 1.000000000000000000, 0.6813042296466748082, 1.000000000000000000),
 ( 1.000000000000000000, 0.6800080602364667604, 1.000000000000000000),
 ( 1.000000000000000000, 0.6804313476833027119, 1.000000000000000000),
 ( 1.000000000000000000, 0.6820608860769757920, 1.000000000000000000),
 ( 1.000000000000000000, 0.6877885785809060293, 1.000000000000000000),
 ( 1.000000000000000000, 0.6919289788393708784, 1.000000000000000000),
 ( 1.000000000000000000, 0.7019562628004784033, 1.000000000000000000),
 ( 1.000000000000000000, 0.7078144704192228520, 1.000000000000000000),
 ( 1.000000000000000000, 0.7207186550667057379, 1.000000000000000000),
 ( 1.000000000000000000, 0.7278201325373979680, 1.000000000000000000),
 ( 1.000000000000000000, 0.7499733481817499881, 1.000000000000000000),
 ( 1.000000000000000000, 0.7658307437853975053, 1.000000000000000000),
 ( 1.000000000000000000, 0.7976817372220619262, 1.000000000000000000),
 ( 1.000000000000000000, 0.8132405326115809130, 1.000000000000000000),
 ( 1.000000000000000000, 0.8429607034202760696, 1.000000000000000000),
 ( 1.000000000000000000, 0.8572315153285383627, 1.000000000000000000),
 ( 1.000000000000000000, 0.8831414977311506931, 1.000000000000000000),
 ( 1.000000000000000000, 0.8948694253068246729, 1.000000000000000000),
 ( 1.000000000000000000, 0.9052370393127044945, 1.000000000000000000) ) ) 
 REPRESENTATION_ITEM ( '' )  SURFACE ( )  );
#30876 = DIRECTION ( 'NONE',  ( 0.000000000000000000, 0.000000000000000000, -1.000000000000000000 ) ) ;
#30877 = CARTESIAN_POINT ( 'NONE',  ( 0.2687203115727492264, -1.674044157977605529, 0.5754666865148680976 ) ) ;
#30878 = B_SPLINE_CURVE_WITH_KNOTS ( 'NONE', 3,
 ( #15855, #2908, #9264, #2698, #31303, #6575 ),
 .UNSPECIFIED., .F., .F.,
 ( 4, 2, 4 ),
 ( 1.734723475976807094E-18, 0.0003446483068616760137, 0.0006892966137233502927 ),
 .UNSPECIFIED. ) ;
#30879 = CARTESIAN_POINT ( 'NONE',  ( 0.3186320389496528627, -1.760431904683431359, 0.5682417262808792113 ) ) ;
#30880 = DIRECTION ( 'NONE',  ( 0.4379975771764401671, 0.000000000000000000, -0.8989761522907980806 ) ) ;
#30881 = CARTESIAN_POINT ( 'NONE',  ( 0.03113248654051816583, 0.1428018198284763673, -0.2638325989215043466 ) ) ;
#30882 = CARTESIAN_POINT ( 'NONE',  ( 0.4790130493689879199, -1.660633143797948241, 0.5197417262808792238 ) ) ;
#30883 = CARTESIAN_POINT ( 'NONE',  ( 0.4026494850530986658, -1.127712942440639354, 0.6048530416235159413 ) ) ;
#30884 = DIRECTION ( 'NONE',  ( -0.4999551463232373427, 0.8660512985181134660, -0.000000000000000000 ) ) ;
#30885 = SHAPE_REPRESENTATION_RELATIONSHIP ( 'NONE' , 'NONE' ,  #30147, #22116 ) ;
#30886 = CARTESIAN_POINT ( 'NONE',  ( -0.1210148435730249716, -0.5061394519557976812, 0.3122829191278992389 ) ) ;
#30887 = CARTESIAN_POINT ( 'NONE',  ( 0.04402670621142950463, -0.8156408044542829971, 0.6980404683681784572 ) ) ;
#30888 = CARTESIAN_POINT ( 'NONE',  ( 0.06797834727357382478, -1.112657892433854601, 0.7541383320516555910 ) ) ;
#30889 = PERSON_AND_ORGANIZATION ( #28500, #32463 ) ;
#30890 = CARTESIAN_POINT ( 'NONE',  ( 0.4077406957728484382, -0.9605384586880818532, 0.7982698588713066368 ) ) ;
#30891 = AXIS2_PLACEMENT_3D ( 'NONE', #38437, #7149, #19716 ) ;
#30892 = EDGE_CURVE ( 'NONE', #14547, #38007, #29273, .T. ) ;
#30893 = CARTESIAN_POINT ( 'NONE',  ( -0.02000000000000000042, -1.459219328725982034, -0.1828911325362468643 ) ) ;
#30894 = EDGE_CURVE ( 'NONE', #35903, #8335, #22684, .T. ) ;
#30895 = CARTESIAN_POINT ( 'NONE',  ( 0.03303737228521604757, -0.08827089426067215305, -0.5134066811673330122 ) ) ;
#30896 = CARTESIAN_POINT ( 'NONE',  ( -0.2746410161513779258, -1.874946189051298617, -0.07947534077849521816 ) ) ;
#30897 = VERTEX_POINT ( 'NONE', #2892 ) ;
#30898 = FACE_OUTER_BOUND ( 'NONE', #12253, .T. ) ;
#30899 = CARTESIAN_POINT ( 'NONE',  ( 0.2082049042024939622, -1.421168782641690331, 0.9443853284052463604 ) ) ;
#30900 = CARTESIAN_POINT ( 'NONE',  ( 0.1370985950931609409, -0.6139791525162832109, 0.3469096356793540670 ) ) ;
#30902 = ORIENTED_EDGE ( 'NONE', *, *, #14586, .T. ) ;
#30901 = CARTESIAN_POINT ( 'NONE',  ( -0.01548846960707524721, 0.2306506793134044109, -0.4716198300880319882 ) ) ;
#30903 = CARTESIAN_POINT ( 'NONE',  ( 0.3883356530642981808, -0.9654559656950375546, 0.7100763952745350327 ) ) ;
#30905 = ORIENTED_EDGE ( 'NONE', *, *, #20091, .T. ) ;
#30904 = VERTEX_POINT ( 'NONE', #17898 ) ;
#30906 = CARTESIAN_POINT ( 'NONE',  ( 0.6176316048552610294, -1.299348609076425465, 0.8015369670086561760 ) ) ;
#30907 = DIRECTION ( 'NONE',  ( 7.771561172376107616E-16, -7.170354002788761615E-17, 1.000000000000000000 ) ) ;
#30908 = DIRECTION ( 'NONE',  ( -1.000000000000000000, -2.403560570595279103E-31, 1.725633230170969455E-31 ) ) ;
#30909 = AXIS2_PLACEMENT_3D ( 'NONE', #15018, #24286, #34133 ) ;
#30910 = CARTESIAN_POINT ( 'NONE',  ( -0.02242905165738729237, 0.4611019942560653506, -0.2233384654055181051 ) ) ;
#30911 = VERTEX_POINT ( 'NONE', #40323 ) ;
#30912 = CARTESIAN_POINT ( 'NONE',  ( 0.1188348172803932595, -0.7700990686786346462, 0.4311705954416762410 ) ) ;
#30913 = CARTESIAN_POINT ( 'NONE',  ( 0.3099360783079950776, -1.765723348835396500, 0.5687896325050014745 ) ) ;
#30914 = CIRCLE ( 'NONE', #18429, 0.08000000000000000167 ) ;
#30915 = CARTESIAN_POINT ( 'NONE',  ( 0.1039748750666900368, -0.5515957074706057117, 0.1901347062354882822 ) ) ;
#30917 = CARTESIAN_POINT ( 'NONE',  ( 0.001718405772027072368, -0.5368582204607379449, 0.07123562922874224212 ) ) ;
#30916 = CARTESIAN_POINT ( 'NONE',  ( 0.3247543563050922510, -1.762377147708333869, 0.4950365382291579963 ) ) ;
#30918 = CARTESIAN_POINT ( 'NONE',  ( -0.05082303569918694003, -0.3162776479886612035, 0.3525632866555290512 ) ) ;
#30919 = ORIENTED_EDGE ( 'NONE', *, *, #17708, .F. ) ;
#30920 = AXIS2_PLACEMENT_3D ( 'NONE', #16393, #22383, #19086 ) ;
#30921 = CARTESIAN_POINT ( 'NONE',  ( 0.4551067410287782389, -1.681698096176633017, 0.5857470455520834562 ) ) ;
#30922 = CARTESIAN_POINT ( 'NONE',  ( 0.2952210513486213661, -0.8093524416240758246, 0.6262659740586482560 ) ) ;
#30923 = DIRECTION ( 'NONE',  ( 1.000000000000000000, 6.779273404243070203E-32, 4.314083075427408311E-32 ) ) ;
#30924 = DIRECTION ( 'NONE',  ( 0.4999999999999988898, -0.8529728694000326961, -0.1497908010108632559 ) ) ;
#30925 =( NAMED_UNIT ( * ) SI_UNIT ( $, .STERADIAN. ) SOLID_ANGLE_UNIT ( ) );
#30926 = FACE_BOUND ( 'NONE', #28538, .T. ) ;
#30927 = CYLINDRICAL_SURFACE ( 'NONE', #8815, 0.08000000000000000167 ) ;
#30928 = CARTESIAN_POINT ( 'NONE',  ( 0.3325622382765076046, -1.175505464167819536, 0.4487935994522243566 ) ) ;
#30929 = CARTESIAN_POINT ( 'NONE',  ( 0.2139922239084591227, -0.7322259512090013578, 0.4012976140435131622 ) ) ;
#30930 = SECURITY_CLASSIFICATION_LEVEL ( 'unclassified' ) ;
#30931 = CARTESIAN_POINT ( 'NONE',  ( -0.1112019842995564389, -0.5080904053907916440, 0.3498664773290697805 ) ) ;
#30932 = AXIS2_PLACEMENT_3D ( 'NONE', #9338, #22135, #25412 ) ;
#30933 = B_SPLINE_CURVE_WITH_KNOTS ( 'NONE', 3,
 ( #28316, #12682, #25241, #9604, #34693, #6500, #37988, #19070, #31609, #15983 ),
 .UNSPECIFIED., .F., .F.,
 ( 4, 2, 2, 2, 4 ),
 ( 9.033896246548822940E-17, 0.0004326218239507741495, 0.0008652436479014579849, 0.001297865471852141820, 0.001730487295802825764 ),
 .UNSPECIFIED. ) ;
#30934 = CARTESIAN_POINT ( 'NONE',  ( 0.02953079040095687308, -0.4684706630666107263, -0.2484463060367401721 ) ) ;
#30935 = FACE_OUTER_BOUND ( 'NONE', #31328, .T. ) ;
#30936 = CARTESIAN_POINT ( 'NONE',  ( -0.02238765564325341170, -0.06997643758148942850, 0.5076344429488280907 ) ) ;
#30937 = CIRCLE ( 'NONE', #13841, 0.01499999999999996302 ) ;
#30938 = B_SPLINE_CURVE_WITH_KNOTS ( 'NONE', 3,
 ( #35167, #34951, #6757, #10461, #16251, #7351 ),
 .UNSPECIFIED., .F., .F.,
 ( 4, 2, 4 ),
 ( 0.003112475973527875465, 0.003739261459126928984, 0.004366046944725982502 ),
 .UNSPECIFIED. ) ;
#30939 = VERTEX_POINT ( 'NONE', #11551 ) ;
#30940 = CARTESIAN_POINT ( 'NONE',  ( -2.112273405726188513E-14, -2.183180860297921466, -0.7137760292030871367 ) ) ;
#30941 = AXIS2_PLACEMENT_3D ( 'NONE', #4982, #23126, #27005 ) ;
#30942 = CARTESIAN_POINT ( 'NONE',  ( 0.7071069014570956490, -1.521634513519168452, 0.5617257377400114438 ) ) ;
#30943 = CIRCLE ( 'NONE', #18469, 0.01499999999999999424 ) ;
#30944 = CARTESIAN_POINT ( 'NONE',  ( -2.112273405726188513E-14, -2.101103246702401339, -0.2895067904002890935 ) ) ;
#30945 = EDGE_LOOP ( 'NONE', ( #21627, #1331 ) ) ;
#30946 = CARTESIAN_POINT ( 'NONE',  ( -0.05252049209742370300, 0.009108187116141133396, -0.4689942714594979023 ) ) ;
#30947 = CARTESIAN_POINT ( 'NONE',  ( 0.008832803565516154920, -0.8460330395702395645, 0.2167343075818525255 ) ) ;
#30949 = ORIENTED_EDGE ( 'NONE', *, *, #1364, .F. ) ;
#30948 = EDGE_LOOP ( 'NONE', ( #36254, #33323, #2687, #38770 ) ) ;
#30950 = DIRECTION ( 'NONE',  ( 0.000000000000000000, 0.000000000000000000, -1.000000000000000000 ) ) ;
#30951 = ORIENTED_EDGE ( 'NONE', *, *, #26772, .T. ) ;
#30952 = CARTESIAN_POINT ( 'NONE',  ( -0.06980746140711623082, 0.000000000000000000, 0.000000000000000000 ) ) ;
#30953 = CARTESIAN_POINT ( 'NONE',  ( 0.05279905671745278167, -0.4315505476814280317, -0.1821453894719594346 ) ) ;
#30954 = CARTESIAN_POINT ( 'NONE',  ( 0.3728899637934937061, -1.734176460878569914, -0.3423889237934055751 ) ) ;
#30955 = CARTESIAN_POINT ( 'NONE',  ( 0.3757471142192211344, -1.766731021160330428, -0.5680748514784754732 ) ) ;
#30957 = CARTESIAN_POINT ( 'NONE',  ( 0.2211959769661342168, -1.309495541150525799, -0.4400554600884077350 ) ) ;
#30956 = CARTESIAN_POINT ( 'NONE',  ( 0.03642997641689302291, 0.5061875831641746704, 0.07642488348723125435 ) ) ;
#30958 = DIRECTION ( 'NONE',  ( 0.000000000000000000, 0.3420201433256721546, 0.9396926207859072067 ) ) ;
#30959 = EDGE_LOOP ( 'NONE', ( #16344, #25421 ) ) ;
#30960 = VECTOR ( 'NONE', #16818, 39.37007874015748143 ) ;
#30961 = DIRECTION ( 'NONE',  ( 0.8660512985181139101, 0.4999551463232363990, 0.000000000000000000 ) ) ;
#30962 = VERTEX_POINT ( 'NONE', #27996 ) ;
#30963 = CARTESIAN_POINT ( 'NONE',  ( 0.04293694706340187017, 0.07181688488226882494, 0.4893579783150006635 ) ) ;
#30964 = CARTESIAN_POINT ( 'NONE',  ( 0.1138873904656961394, -0.7287558471037995922, 0.5555362357626123515 ) ) ;
#30966 = CARTESIAN_POINT ( 'NONE',  ( -0.2399999999999999079, -2.811755946567116471, -0.3200729990151718884 ) ) ;
#30965 = CARTESIAN_POINT ( 'NONE',  ( -0.2746410161513770931, -2.768941938641841904, -0.5551618215276493684 ) ) ;
#30967 = DIRECTION ( 'NONE',  ( -7.771561172376107616E-16, 7.170354002788761615E-17, -1.000000000000000000 ) ) ;
#30968 = LINE ( 'NONE', #40631, #16559 ) ;
#30969 = UNCERTAINTY_MEASURE_WITH_UNIT (LENGTH_MEASURE( 1.000000000000000082E-05 ), #14030, 'distance_accuracy_value', 'NONE');
#30970 = CYLINDRICAL_SURFACE ( 'NONE', #28516, 0.2149999999999999967 ) ;
#30971 = CIRCLE ( 'NONE', #11910, 0.04749999999977556897 ) ;
#30972 = CARTESIAN_POINT ( 'NONE',  ( 0.5732843912231511130, -1.499081617108205977, 0.5610695280922421979 ) ) ;
#30973 = CARTESIAN_POINT ( 'NONE',  ( 0.4173100523516673488, -1.700895175538478021, 0.4281662355554799460 ) ) ;
#30974 = FACE_OUTER_BOUND ( 'NONE', #15787, .T. ) ;
#30975 = AXIS2_PLACEMENT_3D ( 'NONE', #5606, #4999, #17954 ) ;
#30976 = VERTEX_POINT ( 'NONE', #40533 ) ;
#30977 = DIRECTION ( 'NONE',  ( 1.664003471950577032E-31, 3.330669073875470114E-16, 1.000000000000000000 ) ) ;
#30978 = CIRCLE ( 'NONE', #13145, 0.1346589359789737705 ) ;
#30979 = FACE_OUTER_BOUND ( 'NONE', #30456, .T. ) ;
#30980 = CIRCLE ( 'NONE', #29011, 0.1946589359789743512 ) ;
#30981 = CARTESIAN_POINT ( 'NONE',  ( 0.000000000000000000, 2.989043273688991467E-32, 0.05000000000000000971 ) ) ;
#30982 = CARTESIAN_POINT ( 'NONE',  ( -0.01548846960707545191, -0.5198120922912051745, -0.07362328916749329155 ) ) ;
#30983 = CARTESIAN_POINT ( 'NONE',  ( 0.2870953417136587471, -0.7492508933039718766, 0.6466144559156578042 ) ) ;
#30984 = CARTESIAN_POINT ( 'NONE',  ( -0.02881302694829528457, 0.2420344415834884688, 0.4354517411081153533 ) ) ;
#30985 = CARTESIAN_POINT ( 'NONE',  ( 0.01347435369769745851, -1.020097873921679943, 0.5726246034863379242 ) ) ;
#30986 = CARTESIAN_POINT ( 'NONE',  ( -0.2300000000000002875, 0.5182417262804733804, 0.1000000000000000194 ) ) ;
#30987 = CARTESIAN_POINT ( 'NONE',  ( 0.1813906338116575978, -1.297206181306920891, -0.7344059994437892591 ) ) ;
#30988 = CARTESIAN_POINT ( 'NONE',  ( 0.08509807008754367852, -0.8316410974449348625, 0.1906738364949772391 ) ) ;
#30989 = CARTESIAN_POINT ( 'NONE',  ( 0.01895884884825208352, 0.2428741539084919021, -0.4598572020609182354 ) ) ;
#30990 = CARTESIAN_POINT ( 'NONE',  ( -0.02000000000000000042, -1.659335422034822205, 0.2169804935274543545 ) ) ;
#30991 = ORIENTED_EDGE ( 'NONE', *, *, #19248, .F. ) ;
#30992 = APPROVAL ( #28326, 'UNSPECIFIED' ) ;
#30993 = CARTESIAN_POINT ( 'NONE',  ( 0.3591498995103403202, -1.737620376665804267, -0.5147966178037288731 ) ) ;
#30994 = CARTESIAN_POINT ( 'NONE',  ( 0.4184753273149498520, -1.633759443312357229, -0.5155029497116575543 ) ) ;
#30995 = CARTESIAN_POINT ( 'NONE',  ( 0.6666468149095314821, -1.488249007687060921, 0.4225787955285728592 ) ) ;
#30996 = AXIS2_PLACEMENT_3D ( 'NONE', #19946, #38851, #28804 ) ;
#30997 = CARTESIAN_POINT ( 'NONE',  ( 0.4721942231302793669, -1.661553490448594683, -0.6136790096869800815 ) ) ;
#30998 = ORIENTED_EDGE ( 'NONE', *, *, #35685, .F. ) ;
#30999 = CARTESIAN_POINT ( 'NONE',  ( 0.5299567604580853741, -1.673323247257030522, -0.5639626154586274698 ) ) ;
#31000 = VECTOR ( 'NONE', #20770, 39.37007874015748143 ) ;
#31001 = CIRCLE ( 'NONE', #13932, 2.001558204291726373 ) ;
#31002 = ORIENTED_EDGE ( 'NONE', *, *, #14497, .F. ) ;
#31003 = CARTESIAN_POINT ( 'NONE',  ( 0.3229310443258136543, -1.169691403921407025, 0.5631135211526986373 ) ) ;
#31004 = DIRECTION ( 'NONE',  ( 0.4999551463232371762, -0.8660512985181134660, 0.000000000000000000 ) ) ;
#31005 = CARTESIAN_POINT ( 'NONE',  ( 0.03478489236951484015, 0.3590487419276194303, -0.3712145292148960607 ) ) ;
#31006 = VECTOR ( 'NONE', #7912, 39.37007874015748143 ) ;
#31007 = CARTESIAN_POINT ( 'NONE',  ( 0.5121945966484598989, -1.314982590827621811, 0.5851977928667088102 ) ) ;
#31009 = CARTESIAN_POINT ( 'NONE',  ( 0.5048660853949354932, -1.606428814459148979, -0.6256849655409983946 ) ) ;
#31008 = DIRECTION ( 'NONE',  ( 0.4999999999999996114, 0.000000000000000000, -0.8660254037844388186 ) ) ;
#31010 = CARTESIAN_POINT ( 'NONE',  ( 0.4045633573398161875, -1.022308794230461171, 0.6485999566564401020 ) ) ;
#31011 = ORIENTED_EDGE ( 'NONE', *, *, #26862, .T. ) ;
#31012 = CALENDAR_DATE ( 2026, 13, 10 ) ;
#31013 = CARTESIAN_POINT ( 'NONE',  ( 0.1051913758597731452, -1.410370913283630623, 0.5802209346841724624 ) ) ;
#31014 = ORIENTED_EDGE ( 'NONE', *, *, #15538, .F. ) ;
#31015 = VERTEX_POINT ( 'NONE', #30465 ) ;
#31016 = EDGE_CURVE ( 'NONE', #16220, #25252, #12151, .T. ) ;
#31017 = CARTESIAN_POINT ( 'NONE',  ( 0.3586591433503226178, -1.621797892226208404, 0.6182109731304538114 ) ) ;
#31019 = CARTESIAN_POINT ( 'NONE',  ( 0.1752196092396576255, -0.8414204078959418576, -0.02572121894636038297 ) ) ;
#31018 = CARTESIAN_POINT ( 'NONE',  ( 0.6409058204046232943, -1.459016202299332710, -0.5155029497116575543 ) ) ;
#31020 = CARTESIAN_POINT ( 'NONE',  ( 0.5965761245944036784, -1.493465029535157029, 0.5182417262812423209 ) ) ;
#31021 = ORIENTED_EDGE ( 'NONE', *, *, #33823, .F. ) ;
#31022 = ORIENTED_EDGE ( 'NONE', *, *, #36557, .T. ) ;
#31023 = CARTESIAN_POINT ( 'NONE',  ( 0.4713681159961597977, -1.077402325356330737, 0.7137236214398411382 ) ) ;
#31024 = CARTESIAN_POINT ( 'NONE',  ( 0.5418845258822191369, -1.488322812234847525, 0.7085126686041083310 ) ) ;
#31025 = VERTEX_POINT ( 'NONE', #27183 ) ;
#31026 = CARTESIAN_POINT ( 'NONE',  ( 0.3504057387187116679, -1.153664717295437070, 0.4422128889498895266 ) ) ;
#31027 = EDGE_CURVE ( 'NONE', #17786, #3745, #5557, .T. ) ;
#31028 = CARTESIAN_POINT ( 'NONE',  ( -0.02000000000000000042, -2.092549851682985018, -0.5406114768595331466 ) ) ;
#31029 = B_SPLINE_CURVE_WITH_KNOTS ( 'NONE', 3,
 ( #30656, #14815, #37418, #2476, #15013, #24283, #25085, #15421, #27379, #40089 ),
 .UNSPECIFIED., .F., .F.,
 ( 4, 2, 2, 2, 4 ),
 ( 1.412501740721826955E-14, 0.0003711039185504978310, 0.0007422078370868705676, 0.001113311755623243304, 0.001484415674159616149 ),
 .UNSPECIFIED. ) ;
#31030 = CARTESIAN_POINT ( 'NONE',  ( 0.01053425445852829503, -1.728867745475969109, -0.3673112671014556185 ) ) ;
#31031 = ADVANCED_FACE ( 'NONE', ( #37034 ), #21824, .T. ) ;
#31032 = AXIS2_PLACEMENT_3D ( 'NONE', #19363, #38258, #38060 ) ;
#31033 = CARTESIAN_POINT ( 'NONE',  ( -0.1093417548588324489, -0.4991680509866276982, 0.3564048400776990699 ) ) ;
#31034 = EDGE_CURVE ( 'NONE', #18976, #5233, #3708, .T. ) ;
#31035 = EDGE_CURVE ( 'NONE', #5011, #35762, #24645, .T. ) ;
#31036 = CARTESIAN_POINT ( 'NONE',  ( 0.3999999999999787059, -2.097675824466503691, -0.5196396315034578217 ) ) ;
#31037 = AXIS2_PLACEMENT_3D ( 'NONE', #25283, #443, #3258 ) ;
#31038 = CARTESIAN_POINT ( 'NONE',  ( 0.7472694261237929902, -1.513267490863592135, 0.4687417262808789009 ) ) ;
#31039 = VECTOR ( 'NONE', #26158, 39.37007874015748854 ) ;
#31040 = CARTESIAN_POINT ( 'NONE',  ( 0.08105144843878842043, -1.319509989509974002, 0.5764475800623926061 ) ) ;
#31041 = CARTESIAN_POINT ( 'NONE',  ( 0.007443814426054808607, -1.701641051468849364, -0.6331095842549401276 ) ) ;
#31042 = CARTESIAN_POINT ( 'NONE',  ( 0.04329528483221436325, -1.226008797194266586, 0.6628706426414217034 ) ) ;
#31043 = PERSON_AND_ORGANIZATION_ROLE ( 'design_supplier' ) ;
#31044 = CARTESIAN_POINT ( 'NONE',  ( 0.2870562969094627714, -0.9697506529368410400, 0.5438065585693926396 ) ) ;
#31045 = CARTESIAN_POINT ( 'NONE',  ( 0.4837706980973027759, -1.122837591129260737, 0.5209615820093888017 ) ) ;
#31046 = CARTESIAN_POINT ( 'NONE',  ( 0.1590992539432692365, -1.295692464083599171, 0.5182417262812423209 ) ) ;
#31047 = CARTESIAN_POINT ( 'NONE',  ( -0.05464101615137786222, -2.196071624283071788, -0.9424000883860228495 ) ) ;
#31048 = EDGE_CURVE ( 'NONE', #3878, #28752, #17399, .T. ) ;
#31049 = APPROVAL ( #7184, 'UNSPECIFIED' ) ;
#31050 = CARTESIAN_POINT ( 'NONE',  ( 0.003677659035771949428, -0.9373694290314303901, 0.4460629830528545781 ) ) ;
#31051 = LINE ( 'NONE', #11722, #7448 ) ;
#31052 = CARTESIAN_POINT ( 'NONE',  ( 0.2027840892200388767, -1.637248379545634958, -0.6903293078929895188 ) ) ;
#31053 = CARTESIAN_POINT ( 'NONE',  ( 0.3827394763927673971, -1.608088298394132254, 0.5182417262812428760 ) ) ;
#31054 = VERTEX_POINT ( 'NONE', #6564 ) ;
#31055 = VERTEX_POINT ( 'NONE', #9864 ) ;
#31056 = LINE ( 'NONE', #9233, #35476 ) ;
#31057 = VERTEX_POINT ( 'NONE', #25939 ) ;
#31058 = CARTESIAN_POINT ( 'NONE',  ( -0.08000000000000000167, -2.589364949149576933, -0.2950346662398796171 ) ) ;
#31059 = CARTESIAN_POINT ( 'NONE',  ( -0.04293701532779534841, -0.4432143466407583721, -0.2195216604697256546 ) ) ;
#31060 = AXIS2_PLACEMENT_3D ( 'NONE', #37968, #32544, #22914 ) ;
#31061 = CARTESIAN_POINT ( 'NONE',  ( -0.02953079040095571081, -0.09152108205201821278, -0.5223162075576460728 ) ) ;
#31063 = ORIENTED_EDGE ( 'NONE', *, *, #1272, .T. ) ;
#31062 = CARTESIAN_POINT ( 'NONE',  ( -0.02000000000000000042, -2.320036485105098301, -0.4341690811493933433 ) ) ;
#31064 = ORIENTED_EDGE ( 'NONE', *, *, #23007, .F. ) ;
#31065 = CARTESIAN_POINT ( 'NONE',  ( 0.03159140494780130620, 0.4482517543799765525, -0.2030416442520428522 ) ) ;
#31066 = AXIS2_PLACEMENT_3D ( 'NONE', #5123, #4712, #35800 ) ;
#31067 = EDGE_LOOP ( 'NONE', ( #21082, #25525, #3975, #37464 ) ) ;
#31068 = CIRCLE ( 'NONE', #19270, 0.1699999999999995404 ) ;
#31069 = CARTESIAN_POINT ( 'NONE',  ( 0.1424451214204122962, -1.140609330361415763, 0.8966624996383008028 ) ) ;
#31071 = CARTESIAN_POINT ( 'NONE',  ( 0.4182170724685722041, -1.587570233393474251, -0.3841720924506121793 ) ) ;
#31070 = CARTESIAN_POINT ( 'NONE',  ( 0.2259872153612249857, -0.9582317320479798450, 0.6774812835207550954 ) ) ;
#31072 = CARTESIAN_POINT ( 'NONE',  ( 0.3605448558321485697, -1.159604706203796631, 0.5182417262812284431 ) ) ;
#31073 = TOROIDAL_SURFACE ( 'NONE', #25115, 0.05330708661417342398, 0.01000000000000000021 ) ;
#31074 = CARTESIAN_POINT ( 'NONE',  ( 0.4092319501327035813, -1.708177749814091761, 0.4221986184566056122 ) ) ;
#31076 = ORIENTED_EDGE ( 'NONE', *, *, #15062, .F. ) ;
#31075 = VERTEX_POINT ( 'NONE', #35930 ) ;
#31077 = CARTESIAN_POINT ( 'NONE',  ( 0.3863936565759469866, -1.896679156257589538, -0.4880250169076069677 ) ) ;
#31078 = CARTESIAN_POINT ( 'NONE',  ( 0.02999999999997886302, -2.183180860297921466, -0.7137760292030871367 ) ) ;
#31079 = CARTESIAN_POINT ( 'NONE',  ( -0.05137569054208774438, -0.4554428576828106201, 0.1244487204292429872 ) ) ;
#31080 = EDGE_CURVE ( 'NONE', #36373, #33391, #34757, .T. ) ;
#31081 = CARTESIAN_POINT ( 'NONE',  ( 0.5293880808009361338, -1.380208753696393842, 0.7890457912007839969 ) ) ;
#31082 = CIRCLE ( 'NONE', #11365, 0.1700000000000001232 ) ;
#31083 = DIRECTION ( 'NONE',  ( 1.000000000000000000, 2.341930812374887555E-31, -1.664003471950578127E-31 ) ) ;
#31084 = CARTESIAN_POINT ( 'NONE',  ( 0.1968545423636366143, -1.364578978885418126, 0.9371999825232737447 ) ) ;
#31085 = EDGE_CURVE ( 'NONE', #22416, #13200, #6138, .T. ) ;
#31086 = EDGE_CURVE ( 'NONE', #34947, #30911, #55, .T. ) ;
#31087 = CARTESIAN_POINT ( 'NONE',  ( 0.3170005508008052475, -1.687968217625634315, 0.8639454125425393149 ) ) ;
#31088 = EDGE_CURVE ( 'NONE', #21667, #34841, #22436, .T. ) ;
#31089 = DIRECTION ( 'NONE',  ( 1.000000000000000000, -8.638708177629702698E-13, 2.382021192243033701E-12 ) ) ;
#31090 = CARTESIAN_POINT ( 'NONE',  ( 0.5705082898449433948, -1.615108203520839947, 0.3157417262808777658 ) ) ;
#31091 = DIRECTION ( 'NONE',  ( 1.188678714063530652E-15, -1.000000000000000000, 0.000000000000000000 ) ) ;
#31092 = CARTESIAN_POINT ( 'NONE',  ( 0.1999999999999789724, -2.097675824466503691, -0.5196396315034578217 ) ) ;
#31093 = VECTOR ( 'NONE', #17067, 39.37007874015748143 ) ;
#31094 = CARTESIAN_POINT ( 'NONE',  ( 0.04047170147977612042, -0.2415774042519004960, 0.4392095914548704294 ) ) ;
#31095 = CARTESIAN_POINT ( 'NONE',  ( 0.1958798485499332886, -1.272568564212325670, 1.036395571016125006 ) ) ;
#31096 = CARTESIAN_POINT ( 'NONE',  ( 0.08877126294492045100, -1.285961541598747981, 0.7406644231755382668 ) ) ;
#31097 = COORDINATED_UNIVERSAL_TIME_OFFSET ( 0, 0, .AHEAD. ) ;
#31098 = VECTOR ( 'NONE', #14759, 39.37007874015748854 ) ;
#31099 = CARTESIAN_POINT ( 'NONE',  ( 0.1875000000000001943, -0.4593131964907913312, 0.1457185332388694909 ) ) ;
#31100 = CIRCLE ( 'NONE', #8089, 0.1620173459747806799 ) ;
#31101 = EDGE_CURVE ( 'NONE', #21274, #8445, #26268, .T. ) ;
#31102 = ADVANCED_FACE ( 'NONE', ( #16263 ), #30737, .T. ) ;
#31103 = CARTESIAN_POINT ( 'NONE',  ( 0.3179616082204479444, -1.253011040271057697, -0.5155029497116575543 ) ) ;
#31104 = CARTESIAN_POINT ( 'NONE',  ( 0.3289444927862943957, -1.212030846925817196, -0.5155029497116575543 ) ) ;
#31105 = DIRECTION ( 'NONE',  ( 0.000000000000000000, -3.885780586188049371E-16, -1.000000000000000000 ) ) ;
#31106 = B_SPLINE_CURVE_WITH_KNOTS ( 'NONE', 3,
 ( #33708, #6336, #9030, #25276, #2650, #34314, #12322, #23, #40283, #34114 ),
 .UNSPECIFIED., .F., .F.,
 ( 4, 2, 2, 2, 4 ),
 ( 1.734723475976807094E-18, 0.0003557584921360815795, 0.0007115169842721614244, 0.001067275476408241323, 0.001423033968544321114 ),
 .UNSPECIFIED. ) ;
#31107 = VECTOR ( 'NONE', #4516, 39.37007874015748854 ) ;
#31108 = VECTOR ( 'NONE', #29514, 39.37007874015748854 ) ;
#31109 = ORIENTED_EDGE ( 'NONE', *, *, #13667, .F. ) ;
#31110 = CARTESIAN_POINT ( 'NONE',  ( -0.3000000000000000999, -2.407646569606659792, -0.8438593182631384249 ) ) ;
#31111 = ORIENTED_EDGE ( 'NONE', *, *, #35593, .F. ) ;
#31112 = DIRECTION ( 'NONE',  ( -0.4492559606623149349, 8.326672684688674053E-17, 0.8934030903289849057 ) ) ;
#31113 = CARTESIAN_POINT ( 'NONE',  ( 0.2728372402267926766, -1.642600808974832072, 0.7657233710704415275 ) ) ;
#31115 = ORIENTED_EDGE ( 'NONE', *, *, #24783, .F. ) ;
#31114 = CARTESIAN_POINT ( 'NONE',  ( 0.1489746679736130563, -0.6542566974029685456, 0.4247869901793544511 ) ) ;
#31117 = ORIENTED_EDGE ( 'NONE', *, *, #20570, .F. ) ;
#31116 = CARTESIAN_POINT ( 'NONE',  ( -0.1499999999999996336, 0.1249999999999999029, 0.000000000000000000 ) ) ;
#31118 = CARTESIAN_POINT ( 'NONE',  ( 0.4104166757648185504, -0.9945572768306742972, 0.7245767828144217271 ) ) ;
#31120 = ORIENTED_EDGE ( 'NONE', *, *, #36897, .F. ) ;
#31119 = EDGE_LOOP ( 'NONE', ( #12388, #36017 ) ) ;
#31121 = CARTESIAN_POINT ( 'NONE',  ( 0.6949781612789637242, -1.427105545965590583, 0.6651444036754494693 ) ) ;
#31122 =( BOUNDED_SURFACE ( )  B_SPLINE_SURFACE ( 3, 2, ( 
 ( #27385, #17685, #30232 ),
 ( #2064, #13995, #14392 ),
 ( #11730, #14598, #27171 ),
 ( #24288, #4722, #11534 ),
 ( #39104, #36010, #11121 ),
 ( #29848, #1687, #23680 ) ),
 .UNSPECIFIED., .F., .F., .F. ) 
 B_SPLINE_SURFACE_WITH_KNOTS ( ( 4, 2, 4 ),
 ( 3, 3 ),
 ( -1.301042606982605321E-17, 0.0009782491413249925528, 0.001956498282649998116 ),
 ( 0.000000000000000000, 1.000000000000000000 ),
 .UNSPECIFIED. ) 
 GEOMETRIC_REPRESENTATION_ITEM ( )  RATIONAL_B_SPLINE_SURFACE ( (
 ( 1.000000000000000000, 0.8660688067376841603, 1.000000000000000000),
 ( 1.000000000000000000, 0.8670375503518229499, 1.000000000000000000),
 ( 1.000000000000000000, 0.8618718521359357565, 1.000000000000000000),
 ( 1.000000000000000000, 0.8415687179548819730, 1.000000000000000000),
 ( 1.000000000000000000, 0.8267810924324421329, 1.000000000000000000),
 ( 1.000000000000000000, 0.8102556146343646848, 1.000000000000000000) ) ) 
 REPRESENTATION_ITEM ( '' )  SURFACE ( )  );
#31123 = CARTESIAN_POINT ( 'NONE',  ( 0.2914323826288400254, -1.233685883474753497, -0.5166151207188711680 ) ) ;
#31124 = CARTESIAN_POINT ( 'NONE',  ( -0.02953079040095700838, 0.000000000000000000, 0.000000000000000000 ) ) ;
#31125 = CONTEXT_DEPENDENT_SHAPE_REPRESENTATION ( #22190, #23951 ) ;
#31126 = AXIS2_PLACEMENT_3D ( 'NONE', #34937, #10264, #13925 ) ;
#31127 = CARTESIAN_POINT ( 'NONE',  ( 0.07216878364870311924, 0.000000000000000000, 0.1249999999999999029 ) ) ;
#31128 = ORIENTED_EDGE ( 'NONE', *, *, #446, .F. ) ;
#31129 = CARTESIAN_POINT ( 'NONE',  ( 0.2811537305380201190, -0.9978850141101639482, 0.7019614375224079161 ) ) ;
#31130 = CIRCLE ( 'NONE', #24558, 0.04500000000000030365 ) ;
#31131 = CARTESIAN_POINT ( 'NONE',  ( 0.3222111719196821267, -1.761649659472191543, 0.6126613877097355498 ) ) ;
#31132 = AXIS2_PLACEMENT_3D ( 'NONE', #9730, #13031, #22300 ) ;
#31133 = CARTESIAN_POINT ( 'NONE',  ( 0.1044438712203083208, -0.5602818493527880195, 0.2215003945582872391 ) ) ;
#31135 = DIRECTION ( 'NONE',  ( 1.000000000000000000, 0.000000000000000000, 0.000000000000000000 ) ) ;
#31134 = CARTESIAN_POINT ( 'NONE',  ( 0.3418696078408812178, -1.748333077232472554, 0.4473164556818181037 ) ) ;
#31136 = CARTESIAN_POINT ( 'NONE',  ( -0.03309057659885157598, -0.2303206601891022998, 0.4671007096900186006 ) ) ;
#31137 = ORIENTED_EDGE ( 'NONE', *, *, #6126, .T. ) ;
#31138 = ADVANCED_FACE ( 'NONE', ( #36730 ), #8855, .F. ) ;
#31139 = CARTESIAN_POINT ( 'NONE',  ( 0.4307568529685167347, -1.695672135311921958, 0.6147001973947316955 ) ) ;
#31140 = CARTESIAN_POINT ( 'NONE',  ( 0.6984873844191630265, -1.438842590160148260, 0.5672913894667556134 ) ) ;
#31141 = CIRCLE ( 'NONE', #17362, 0.1550424246542357609 ) ;
#31142 = DIRECTION ( 'NONE',  ( -0.4999551463232377313, 0.8660512985181132439, -0.000000000000000000 ) ) ;
#31143 = VECTOR ( 'NONE', #19368, 39.37007874015748143 ) ;
#31144 = CARTESIAN_POINT ( 'NONE',  ( -0.002162789170891683647, -0.8547793670402533683, 0.1265725835208540984 ) ) ;
#31145 = DIRECTION ( 'NONE',  ( 0.000000000000000000, 0.9510565162951525320, -0.3090169943749502268 ) ) ;
#31146 = CARTESIAN_POINT ( 'NONE',  ( -0.1508044614562676355, 0.4665164580004940720, 0.3602693336111439382 ) ) ;
#31147 = B_SPLINE_CURVE_WITH_KNOTS ( 'NONE', 3,
 ( #5347, #17707, #31441, #39933, #8645, #8254, #15795, #20826, #27407, #2303, #15043, #24307, #6330, #11749, #36831, #33346, #5568, #33754, #213, #22201, #18129, #21218, #3248, #5156, #36646, #30253, #25061, #11560, #39512, #2501, #40118, #2085, #11342, #37595, #14622, #9416, #14414, #21995, #27191, #34520, #18904, #6523, #39726, #8450, #12707, #19096, #26976, #25270, #37811, #24124, #21017, #33535, #17909, #14844, #7543, #4259, #19508, #35729, #28556, #7124, #25888, #29155, #26281, #4044, #31845, #38408, #16402 ),
 .UNSPECIFIED., .F., .F.,
 ( 4, 2, 2, 2, 2, 2, 2, 2, 2, 2, 2, 2, 2, 2, 1, 1, 2, 2, 1, 2, 2, 2, 2, 2, 2, 2, 2, 2, 1, 1, 2, 2, 1, 2, 2, 1, 4 ),
 ( 0.000000000000000000, 0.04613892571620765992, 0.09227785143241531984, 0.1384167771486229936, 0.1845557028648306397, 0.2768335542972459873, 0.3691114057296612794, 0.4152503314458689254, 0.4613892571620765715, 0.5075281828782842730, 0.5305976457363886789, 0.5421323771654402712, 0.5536671085944919746, 0.5652018400235435669, 0.5767365714525951592, 0.5882713028816467515, 0.5911549857389092333, 0.5940386685961718261, 0.5998060343106970116, 0.6228754971687950892, 0.6257591800260565718, 0.6286428628833180543, 0.6344102285978422406, 0.6459449600268917235, 0.6517123257414164650, 0.6574796914559412064, 0.6690144228849906893, 0.6718981057422531711, 0.6747817885995157638, 0.6805491543140408384, 0.6863165200285659129, 0.6920838857430909874, 0.7151533486011910634, 0.7180370314584534341, 0.7209207143157160269, 0.7266880800302409904, 0.7382228114592909174 ),
 .UNSPECIFIED. ) ;
#31148 = CARTESIAN_POINT ( 'NONE',  ( 0.01384654206388801108, -1.688463842650887781, -0.6347859073314252587 ) ) ;
#31149 = CARTESIAN_POINT ( 'NONE',  ( 0.3101988348943303664, -1.188457521969344954, 0.5390384569713482232 ) ) ;
#31150 = CARTESIAN_POINT ( 'NONE',  ( 0.5520143099787153673, -1.183365530476261585, 0.6129298035784942478 ) ) ;
#31151 = CALENDAR_DATE ( 2026, 13, 10 ) ;
#31152 = CARTESIAN_POINT ( 'NONE',  ( 0.6002284735530656334, -1.599240903479319131, 0.6081811307598909977 ) ) ;
#31153 = EDGE_CURVE ( 'NONE', #36582, #27000, #18733, .T. ) ;
#31154 = APPLIED_DATE_AND_TIME_ASSIGNMENT ( #25372, #40574, ( #9595 ) ) ;
#31155 = CARTESIAN_POINT ( 'NONE',  ( 0.1760056095156050660, -1.754827144506087455, -0.6511199371818791048 ) ) ;
#31156 = ADVANCED_FACE ( 'NONE', ( #29748 ), #2320, .F. ) ;
#31157 = CARTESIAN_POINT ( 'NONE',  ( 0.5610715841008669935, -1.505132754039335552, 0.5357057820217212551 ) ) ;
#31158 = CARTESIAN_POINT ( 'NONE',  ( -0.04230258372739675865, 0.004226829447875481149, 0.4686050468223225129 ) ) ;
#31159 = CIRCLE ( 'NONE', #6183, 0.04249999999999994754 ) ;
#31160 = CIRCLE ( 'NONE', #4214, 0.01499999999999995608 ) ;
#31161 = ORIENTED_EDGE ( 'NONE', *, *, #35682, .F. ) ;
#31162 = CARTESIAN_POINT ( 'NONE',  ( 0.4685502202651029569, -1.116536938686066183, 0.5688043585934901003 ) ) ;
#31163 = AXIS2_PLACEMENT_3D ( 'NONE', #14424, #11760, #36655 ) ;
#31164 = CARTESIAN_POINT ( 'NONE',  ( -0.03171893264487114783, -0.2437375926088059808, 0.4645571062479570412 ) ) ;
#31165 = DIRECTION ( 'NONE',  ( 0.000000000000000000, 0.000000000000000000, -1.000000000000000000 ) ) ;
#31166 = EDGE_LOOP ( 'NONE', ( #25194, #39995, #8348, #31732 ) ) ;
#31167 = CARTESIAN_POINT ( 'NONE',  ( -0.05491348488830673918, -0.02524042857556412292, -0.4620240554957946721 ) ) ;
#31168 = AXIS2_PLACEMENT_3D ( 'NONE', #3266, #38631, #19529 ) ;
#31169 = CARTESIAN_POINT ( 'NONE',  ( 0.07936604219207132882, -1.300224580243717565, 0.7373157962401226673 ) ) ;
#31171 = ORIENTED_EDGE ( 'NONE', *, *, #40640, .T. ) ;
#31170 = ORIENTED_EDGE ( 'NONE', *, *, #15220, .F. ) ;
#31172 = ORIENTED_EDGE ( 'NONE', *, *, #14108, .F. ) ;
#31173 = CARTESIAN_POINT ( 'NONE',  ( 0.1443375672974070711, 0.000000000000000000, 0.000000000000000000 ) ) ;
#31174 = CARTESIAN_POINT ( 'NONE',  ( 0.3699999999999789013, -2.097675824466503691, -0.4688691127277795356 ) ) ;
#31175 = DIRECTION ( 'NONE',  ( -1.000000000000000000, -0.000000000000000000, -0.000000000000000000 ) ) ;
#31177 = CARTESIAN_POINT ( 'NONE',  ( 0.2317288817819283253, -1.348463341396027637, 0.5280675649570982788 ) ) ;
#31176 = CARTESIAN_POINT ( 'NONE',  ( 0.01548846960707409362, 0.5203207976467955076, 0.08861466064782100305 ) ) ;
#31178 = CARTESIAN_POINT ( 'NONE',  ( 0.01548846960706596991, -0.2450655194479906540, -0.4674710490749469649 ) ) ;
#31179 = EDGE_LOOP ( 'NONE', ( #31962, #39654, #7830, #13355 ) ) ;
#31180 = CARTESIAN_POINT ( 'NONE',  ( 0.06909380327002452582, -1.315850677508620281, 0.5176656306823473885 ) ) ;
#31181 = ORIENTED_EDGE ( 'NONE', *, *, #39949, .F. ) ;
#31182 = CARTESIAN_POINT ( 'NONE',  ( 0.05634304521267755744, 1.092739197465705287E-15, 0.4588823192046724841 ) ) ;
#31183 = CARTESIAN_POINT ( 'NONE',  ( 0.4715550156134034054, -1.554656505831566227, 0.6419049491724836409 ) ) ;
#31185 = CARTESIAN_POINT ( 'NONE',  ( 0.5654497241578824163, -1.618822071068416912, 0.5682417262808787672 ) ) ;
#31184 = CYLINDRICAL_SURFACE ( 'NONE', #17148, 0.08000000000000000167 ) ;
#31186 = CARTESIAN_POINT ( 'NONE',  ( 0.06844683568258899675, -1.327643015831073914, 0.5607579029421154715 ) ) ;
#31187 = CARTESIAN_POINT ( 'NONE',  ( 0.3699999999999784017, -2.054734391222358347, -0.6850094247584036511 ) ) ;
#31188 = AXIS2_PLACEMENT_3D ( 'NONE', #16492, #16704, #28843 ) ;
#31189 = EDGE_CURVE ( 'NONE', #34622, #20383, #28570, .T. ) ;
#31190 = CARTESIAN_POINT ( 'NONE',  ( 0.2722331219925429036, -1.671874623808670135, 0.4849083929475441201 ) ) ;
#31191 = VECTOR ( 'NONE', #11455, 39.37007874015748143 ) ;
#31192 = CARTESIAN_POINT ( 'NONE',  ( 0.1253914729212589063, -0.5518637161767581123, 0.1703337146848046546 ) ) ;
#31193 = CARTESIAN_POINT ( 'NONE',  ( 0.4745856284632649080, -1.668843919975977474, 0.5513519273944286203 ) ) ;
#31194 = B_SPLINE_CURVE_WITH_KNOTS ( 'NONE', 3,
 ( #2868, #12130, #15625, #18710 ),
 .UNSPECIFIED., .F., .F.,
 ( 4, 4 ),
 ( 0.001920789045071016584, 0.002034319970777410426 ),
 .UNSPECIFIED. ) ;
#31195 = CARTESIAN_POINT ( 'NONE',  ( -0.08000000000000000167, -1.910390638264138685, -0.7420407338378623985 ) ) ;
#31196 = AXIS2_PLACEMENT_3D ( 'NONE', #1624, #2425, #14961 ) ;
#31197 = AXIS2_PLACEMENT_3D ( 'NONE', #37519, #22528, #34451 ) ;
#31198 = CARTESIAN_POINT ( 'NONE',  ( -0.01548846960688914087, 0.4638115001434989226, 0.2459753896940841955 ) ) ;
#31199 = APPROVAL_PERSON_ORGANIZATION ( #35392, #31049, #13592 ) ;
#31200 = CARTESIAN_POINT ( 'NONE',  ( 0.2233408083240900899, -1.237973100587790976, 0.5437015457833099807 ) ) ;
#31201 = DIRECTION ( 'NONE',  ( 1.000000000000000000, 6.779273404243070203E-32, 4.314083075427408311E-32 ) ) ;
#31202 = CARTESIAN_POINT ( 'NONE',  ( 0.2284408465079907080, -1.235179063166289781, 0.4809151899966361832 ) ) ;
#31203 = AXIS2_PLACEMENT_3D ( 'NONE', #19566, #22872, #32096 ) ;
#31204 = CARTESIAN_POINT ( 'NONE',  ( 0.1898244942508440503, -0.5073357646527311138, 0.1864979583367220028 ) ) ;
#31205 = CARTESIAN_POINT ( 'NONE',  ( -0.04229883635637872452, 0.2719170545448755805, 0.3816769773555939160 ) ) ;
#31206 = CARTESIAN_POINT ( 'NONE',  ( 0.03300239046062679316, -1.160323239369614123, 0.6643093511034796617 ) ) ;
#31207 = DIRECTION ( 'NONE',  ( 8.881784197001246407E-16, -2.361472542561082612E-16, 1.000000000000000000 ) ) ;
#31208 = CARTESIAN_POINT ( 'NONE',  ( 0.1857430203655688061, -0.8056635886342108366, 0.2698372336795828996 ) ) ;
#31209 = CARTESIAN_POINT ( 'NONE',  ( 0.1291546474001438460, -0.8766933867304865791, 0.5184058891243923384 ) ) ;
#31210 = CARTESIAN_POINT ( 'NONE',  ( 0.03159140494780101477, 0.2432984029592191733, -0.4277399113045144419 ) ) ;
#31211 = DIRECTION ( 'NONE',  ( 1.000000000000000000, 2.341930812374887555E-31, -1.664003471950578127E-31 ) ) ;
#31212 = ORIENTED_EDGE ( 'NONE', *, *, #39193, .T. ) ;
#31213 = CYLINDRICAL_SURFACE ( 'NONE', #27262, 0.08139150547213661047 ) ;
#31214 = CARTESIAN_POINT ( 'NONE',  ( 0.3891537709046165583, -1.706611523097125049, -0.5991981645855274374 ) ) ;
#31215 = VECTOR ( 'NONE', #38700, 39.37007874015748143 ) ;
#31216 = CARTESIAN_POINT ( 'NONE',  ( 0.6465835049539359058, -1.539613817736341872, 0.4182417262808776903 ) ) ;
#31217 = DIRECTION ( 'NONE',  ( 0.000000000000000000, 0.000000000000000000, -1.000000000000000000 ) ) ;
#31218 = EDGE_CURVE ( 'NONE', #24904, #26308, #8349, .T. ) ;
#31219 = CARTESIAN_POINT ( 'NONE',  ( 0.4288946199586322061, -1.677151416097353520, -0.6187118249900269706 ) ) ;
#31220 = CIRCLE ( 'NONE', #2965, 0.5400000000000004796 ) ;
#31221 = B_SPLINE_CURVE_WITH_KNOTS ( 'NONE', 3,
 ( #3004, #3389, #25618, #22340, #3602, #9355, #15553, #28707 ),
 .UNSPECIFIED., .F., .F.,
 ( 4, 2, 2, 4 ),
 ( 0.000000000000000000, 0.0009535720482368597890, 0.001430358072355289792, 0.001907144096473719578 ),
 .UNSPECIFIED. ) ;
#31222 = CIRCLE ( 'NONE', #2969, 0.03749999999977557397 ) ;
#31223 = ORIENTED_EDGE ( 'NONE', *, *, #14727, .T. ) ;
#31224 = CARTESIAN_POINT ( 'NONE',  ( 0.4897592102757907795, -1.696528537887749932, -0.5984293649392188330 ) ) ;
#31225 = CARTESIAN_POINT ( 'NONE',  ( 0.3902357488131970031, -1.138878306233123805, 0.6057535050277017552 ) ) ;
#31226 = APPLIED_SECURITY_CLASSIFICATION_ASSIGNMENT ( #9542, ( #39117 ) ) ;
#31227 = CARTESIAN_POINT ( 'NONE',  ( 0.3283149244379453546, -1.763791535429168889, 0.4875464477737077029 ) ) ;
#31228 = DIRECTION ( 'NONE',  ( 8.881784197001246407E-16, -2.361472542561082612E-16, 1.000000000000000000 ) ) ;
#31229 = CARTESIAN_POINT ( 'NONE',  ( 0.5014320656698512124, -1.296437944250064422, 0.5839483198575456946 ) ) ;
#31230 = DIRECTION ( 'NONE',  ( 0.000000000000000000, 0.000000000000000000, 1.000000000000000000 ) ) ;
#31231 = CARTESIAN_POINT ( 'NONE',  ( 0.5135568109339374576, -1.117989077717415292, 0.5796127612779116145 ) ) ;
#31232 = EDGE_LOOP ( 'NONE', ( #36164, #21323, #13247 ) ) ;
#31233 = DATE_TIME_ROLE ( 'classification_date' ) ;
#31234 = AXIS2_PLACEMENT_3D ( 'NONE', #9214, #27959, #5520 ) ;
#31235 = CARTESIAN_POINT ( 'NONE',  ( -0.6247879186461519074, 0.2375666616292472499, 0.3749999999999995559 ) ) ;
#31236 = ORIENTED_EDGE ( 'NONE', *, *, #20318, .F. ) ;
#31237 = EDGE_LOOP ( 'NONE', ( #2389, #17349, #37684, #12963, #16912, #30502, #803, #11316, #37633 ) ) ;
#31238 = CARTESIAN_POINT ( 'NONE',  ( 0.3671697839738085611, -1.545107799971002560, 0.8005747561286837843 ) ) ;
#31240 = CARTESIAN_POINT ( 'NONE',  ( 0.1115501525409109546, -0.8938576055124605180, 0.02086076245356002085 ) ) ;
#31239 = LINE ( 'NONE', #40059, #2037 ) ;
#31241 = CARTESIAN_POINT ( 'NONE',  ( 0.6215940427273412006, -1.611809246851749311, 0.5182417262812423209 ) ) ;
#31242 = ORIENTED_EDGE ( 'NONE', *, *, #29512, .F. ) ;
#31243 = ORIENTED_EDGE ( 'NONE', *, *, #27558, .T. ) ;
#31244 = CARTESIAN_POINT ( 'NONE',  ( 0.3197192075068525097, -1.053170137840971687, 0.6328512510037338501 ) ) ;
#31245 = CARTESIAN_POINT ( 'NONE',  ( 0.4770251848494882485, -1.362019963231613673, 0.8156266216142553649 ) ) ;
#31246 = EDGE_LOOP ( 'NONE', ( #17420, #24550, #26961, #29585 ) ) ;
#31247 = DIRECTION ( 'NONE',  ( 0.4999551463232373427, -0.8660512985181134660, 0.000000000000000000 ) ) ;
#31248 = CARTESIAN_POINT ( 'NONE',  ( -0.01548846960707524721, -0.4638115001430989648, 0.2459753896937853235 ) ) ;
#31249 = CARTESIAN_POINT ( 'NONE',  ( 0.5930815638500551712, -1.500577258630007904, -0.3915676963420799961 ) ) ;
#31250 = CIRCLE ( 'NONE', #19416, 0.1000000000000000194 ) ;
#31251 = CARTESIAN_POINT ( 'NONE',  ( 0.3238605203897769180, -1.709547670968458943, -0.3346915668799618770 ) ) ;
#31252 = VECTOR ( 'NONE', #34675, 39.37007874015748143 ) ;
#31253 = DIRECTION ( 'NONE',  ( 0.4999999999999972244, 0.7066258520834661772, 0.5006794435238159924 ) ) ;
#31254 = CARTESIAN_POINT ( 'NONE',  ( 0.4047110712422638534, -1.701609880936963970, 0.4182417262808776903 ) ) ;
#31255 = CARTESIAN_POINT ( 'NONE',  ( 0.1999999999999786671, -2.166079853131637201, -0.5407606602423821185 ) ) ;
#31256 = ORIENTED_EDGE ( 'NONE', *, *, #40605, .T. ) ;
#31257 = DIRECTION ( 'NONE',  ( 0.4999551463232377313, -0.8660512985181132439, -0.000000000000000000 ) ) ;
#31258 = CARTESIAN_POINT ( 'NONE',  ( 0.002290818369124609372, -0.5198888459286679087, 0.1457185332388686583 ) ) ;
#31259 = COORDINATED_UNIVERSAL_TIME_OFFSET ( 0, 0, .AHEAD. ) ;
#31260 = APPLIED_APPROVAL_ASSIGNMENT ( #19210, ( #25357 ) ) ;
#31261 = CARTESIAN_POINT ( 'NONE',  ( 0.4737957855049246270, -1.072208190283344909, 0.6181471139717461538 ) ) ;
#31262 = CARTESIAN_POINT ( 'NONE',  ( 0.4447797348688822261, -1.136753334708936247, 0.4441811018978158443 ) ) ;
#31263 = CARTESIAN_POINT ( 'NONE',  ( 0.4538227971951512285, -1.220717492415648975, 0.5856983068965044836 ) ) ;
#31264 = AXIS2_PLACEMENT_3D ( 'NONE', #38066, #6578, #22453 ) ;
#31265 = CARTESIAN_POINT ( 'NONE',  ( 0.3121344959780879558, -1.175754444927441300, 0.5182417262812437642 ) ) ;
#31266 = CARTESIAN_POINT ( 'NONE',  ( -0.003124719664520024271, -0.8057675726412024675, 0.09674340762273991867 ) ) ;
#31267 = CYLINDRICAL_SURFACE ( 'NONE', #15362, 0.1000000000000000194 ) ;
#31268 = FACE_OUTER_BOUND ( 'NONE', #38001, .T. ) ;
#31269 = EDGE_CURVE ( 'NONE', #36513, #4385, #16096, .T. ) ;
#31270 = ORIENTED_EDGE ( 'NONE', *, *, #35088, .F. ) ;
#31271 = ORIENTED_EDGE ( 'NONE', *, *, #5215, .T. ) ;
#31272 = PLANE ( 'NONE',  #30909 ) ;
#31273 = ORIENTED_EDGE ( 'NONE', *, *, #24878, .T. ) ;
#31274 = DIRECTION ( 'NONE',  ( 0.000000000000000000, -2.048885995248197236E-14, -1.000000000000000000 ) ) ;
#31275 = FACE_OUTER_BOUND ( 'NONE', #15064, .T. ) ;
#31276 = EDGE_CURVE ( 'NONE', #11981, #30141, #27075, .T. ) ;
#31277 = CARTESIAN_POINT ( 'NONE',  ( 0.3646774744596967821, -1.088638349586324994, 0.8066222157141976767 ) ) ;
#31279 = ORIENTED_EDGE ( 'NONE', *, *, #30864, .T. ) ;
#31278 = CARTESIAN_POINT ( 'NONE',  ( 0.009698722596325677972, -0.5609003310328917191, 0.05071314360984191527 ) ) ;
#31280 = CIRCLE ( 'NONE', #6943, 0.07999999999999996003 ) ;
#31281 = AXIS2_PLACEMENT_3D ( 'NONE', #7082, #38160, #9984 ) ;
#31282 = ADVANCED_FACE ( 'NONE', ( #39410 ), #4837, .T. ) ;
#31283 = ORIENTED_EDGE ( 'NONE', *, *, #38175, .T. ) ;
#31284 = CARTESIAN_POINT ( 'NONE',  ( 0.1890965627226634804, -1.347655541994686068, 0.5182417262812423209 ) ) ;
#31285 = CARTESIAN_POINT ( 'NONE',  ( 0.2857623305721883611, -1.591320169725852551, 0.8243244337802699828 ) ) ;
#31287 = DIRECTION ( 'NONE',  ( 0.4999551463232372317, -0.8660512985181135770, 0.000000000000000000 ) ) ;
#31286 = CARTESIAN_POINT ( 'NONE',  ( 0.1149644705236894937, -0.8668712750652664001, 0.4808557319664010787 ) ) ;
#31288 = APPLIED_APPROVAL_ASSIGNMENT ( #29739, ( #9595 ) ) ;
#31289 = CARTESIAN_POINT ( 'NONE',  ( 0.01184929641461734615, -0.5804339378642296987, -0.09026199020224340286 ) ) ;
#31290 = CARTESIAN_POINT ( 'NONE',  ( -2.112273405726188513E-14, -2.097675824466503691, -0.2588528740066097233 ) ) ;
#31292 = ORIENTED_EDGE ( 'NONE', *, *, #13242, .T. ) ;
#31291 = ORIENTED_EDGE ( 'NONE', *, *, #16187, .F. ) ;
#31293 = DIRECTION ( 'NONE',  ( 1.000000000000000000, 6.779273404243070203E-32, 4.314083075427408311E-32 ) ) ;
#31294 = AXIS2_PLACEMENT_3D ( 'NONE', #7946, #24030, #20322 ) ;
#31295 = DIRECTION ( 'NONE',  ( 0.000000000000000000, -1.000000000000000000, 0.000000000000000000 ) ) ;
#31296 = FACE_OUTER_BOUND ( 'NONE', #1691, .T. ) ;
#31297 = CARTESIAN_POINT ( 'NONE',  ( 0.5517015749519356138, -1.382230921397820556, 0.7776688410150216502 ) ) ;
#31298 = EDGE_CURVE ( 'NONE', #36573, #29082, #29969, .T. ) ;
#31299 = CARTESIAN_POINT ( 'NONE',  ( 0.1289960929160810510, -0.8267361313214416363, 0.2449634403921974735 ) ) ;
#31300 = CARTESIAN_POINT ( 'NONE',  ( -0.08000000000000000167, -2.548345659627495596, -0.2263512047145338768 ) ) ;
#31301 = PRODUCT_RELATED_PRODUCT_CATEGORY ( 'detail', '', ( #4853 ) ) ;
#31302 = CARTESIAN_POINT ( 'NONE',  ( 0.1174434333147871268, -0.9515856618589675353, 0.9146188126943564090 ) ) ;
#31303 = CARTESIAN_POINT ( 'NONE',  ( 0.4003933387480922423, -1.713626439352980091, 0.4219370341759499099 ) ) ;
#31304 = CARTESIAN_POINT ( 'NONE',  ( 0.02999999999997891853, -2.097675824466501915, -0.2588528740066096678 ) ) ;
#31305 = CARTESIAN_POINT ( 'NONE',  ( 0.4679778500672936992, -1.237826332153874942, 0.6057417262809768888 ) ) ;
#31306 = FACE_OUTER_BOUND ( 'NONE', #36116, .T. ) ;
#31307 = CIRCLE ( 'NONE', #40490, 0.03000000000000002318 ) ;
#31308 = CARTESIAN_POINT ( 'NONE',  ( 0.04946288932099399821, -0.2513464261306892489, 0.4057664802068525201 ) ) ;
#31309 = CARTESIAN_POINT ( 'NONE',  ( 0.01054327228848483088, -0.5372198261166355460, 0.4758561573974433023 ) ) ;
#31310 = TOROIDAL_SURFACE ( 'NONE', #13569, 0.08830708661417342731, 0.01499999999999999944 ) ;
#31311 = CARTESIAN_POINT ( 'NONE',  ( 0.08536197900831818397, -1.283296901138165191, 0.7335830683232681393 ) ) ;
#31312 = APPLICATION_PROTOCOL_DEFINITION ( 'international standard', 'automotive_design', 2000, #18750 ) ;
#31313 = CARTESIAN_POINT ( 'NONE',  ( 0.7228851465660607323, -1.479175389011975428, 0.5919814340071456460 ) ) ;
#31314 = LOCAL_TIME ( 0, 53, 7.000000000000000000, #27834 ) ;
#31315 = CARTESIAN_POINT ( 'NONE',  ( -0.03474878377839595717, 0.4640666366555314948, 0.2268437812334333226 ) ) ;
#31316 = B_SPLINE_CURVE_WITH_KNOTS ( 'NONE', 3,
 ( #34529, #28161, #15807, #37825, #22005, #22210, #34119, #18912, #16022, #31449, #34320, #3256, #28566, #28355, #27, #21594, #5735, #9640, #12514, #12720, #5921, #25486, #34727, #31040, #19107, #25070 ),
 .UNSPECIFIED., .F., .F.,
 ( 4, 2, 2, 2, 2, 2, 2, 2, 2, 2, 2, 2, 4 ),
 ( -5.999999996337358855E-08, 0.0003477659952063618613, 0.0006955919904126871538, 0.001391243980825333619, 0.002086895971237980735, 0.002782547961650626116, 0.003130373956856948373, 0.003478199952063270196, 0.003826025947269592452, 0.004173851942475916878, 0.004869503932888550116, 0.005217329928094866301, 0.005565155923301183354 ),
 .UNSPECIFIED. ) ;
#31317 = CARTESIAN_POINT ( 'NONE',  ( -0.2746410161513776482, -2.809880844172510272, -0.2480969101616946892 ) ) ;
#31318 = TOROIDAL_SURFACE ( 'NONE', #17507, 0.07749999999977548459, 0.01000000000000000021 ) ;
#31319 = CARTESIAN_POINT ( 'NONE',  ( 0.3704697912810962501, -1.166474544107111377, 0.4182417262808778013 ) ) ;
#31320 = EDGE_CURVE ( 'NONE', #28752, #13663, #27925, .T. ) ;
#31321 = CARTESIAN_POINT ( 'NONE',  ( -0.01548846960707490547, 0.5198120922912062847, -0.07362328916748482610 ) ) ;
#31322 = EDGE_LOOP ( 'NONE', ( #16042, #38293, #34749, #30460 ) ) ;
#31323 = CARTESIAN_POINT ( 'NONE',  ( -0.2399999999999999079, -2.425196952834860475, -0.6298687015330044492 ) ) ;
#31324 = B_SPLINE_CURVE_WITH_KNOTS ( 'NONE', 3,
 ( #9449, #25091, #12745, #3091, #15633, #37627, #22030, #28591, #31467, #3274, #2121, #15828, #25308, #12960, #25506, #17738, #14655, #26129 ),
 .UNSPECIFIED., .F., .F.,
 ( 4, 2, 2, 2, 2, 2, 2, 2, 4 ),
 ( 0.0003425652276237403562, 0.001007165397454252856, 0.001671765567284765356, 0.002336365737115277640, 0.003000965906945790573, 0.003665566076776302640, 0.004330166246606815574, 0.004994766416437328507, 0.005659366586267840574 ),
 .UNSPECIFIED. ) ;
#31325 = CARTESIAN_POINT ( 'NONE',  ( 0.2697570704576938150, -1.625148811348557043, 0.7999399077722737506 ) ) ;
#31326 = EDGE_CURVE ( 'NONE', #19134, #30280, #14932, .T. ) ;
#31328 = EDGE_LOOP ( 'NONE', ( #34223, #10997, #27780, #17650 ) ) ;
#31327 = CARTESIAN_POINT ( 'NONE',  ( 0.3070561426719275455, -1.006156790695110548, 0.7639484575383966858 ) ) ;
#31330 = ORIENTED_EDGE ( 'NONE', *, *, #13209, .F. ) ;
#31329 = DIRECTION ( 'NONE',  ( 0.8660254037844384856, -2.465190328815710609E-32, -0.5000000000000004441 ) ) ;
#31331 = EDGE_CURVE ( 'NONE', #34358, #3578, #3605, .T. ) ;
#31332 = CARTESIAN_POINT ( 'NONE',  ( 0.3136710858027207949, -0.8676775186001693951, 0.6334163436129683911 ) ) ;
#31334 = ORIENTED_EDGE ( 'NONE', *, *, #3407, .F. ) ;
#31333 = ORIENTED_EDGE ( 'NONE', *, *, #30767, .T. ) ;
#31335 = CARTESIAN_POINT ( 'NONE',  ( 0.4987283714208217700, -1.112815979792688204, 0.8110521570308895090 ) ) ;
#31336 = CARTESIAN_POINT ( 'NONE',  ( 0.3485300389640555441, -1.734513092226865449, -0.5719809208048397542 ) ) ;
#31337 = CARTESIAN_POINT ( 'NONE',  ( -0.1574377185082707353, 0.4885537809602777948, 0.09999999999999989453 ) ) ;
#31338 = APPROVAL_STATUS ( 'not_yet_approved' ) ;
#31339 = CARTESIAN_POINT ( 'NONE',  ( 0.3186320557803343223, -1.760432376530343568, 0.5682926660822772424 ) ) ;
#31340 = ORIENTED_EDGE ( 'NONE', *, *, #20488, .T. ) ;
#31341 = TOROIDAL_SURFACE ( 'NONE', #13593, 1.986674066779348768, 0.01499999999999999944 ) ;
#31342 = CARTESIAN_POINT ( 'NONE',  ( 0.2153886340467147109, -0.9136054407777869368, 0.6428213724677314111 ) ) ;
#31343 = CARTESIAN_POINT ( 'NONE',  ( 0.3166419384220154898, -1.752632602668677597, 0.7236431125229072503 ) ) ;
#31344 = CARTESIAN_POINT ( 'NONE',  ( 0.5253970528185427646, -1.521450895406853965, 0.6493258987034100649 ) ) ;
#31345 = DIRECTION ( 'NONE',  ( 0.000000000000000000, 0.000000000000000000, -1.000000000000000000 ) ) ;
#31346 = EDGE_CURVE ( 'NONE', #16208, #15639, #9531, .T. ) ;
#31347 = CARTESIAN_POINT ( 'NONE',  ( -0.1650539334306630468, 0.4792632177816705807, 0.1214379789123950643 ) ) ;
#31348 = SECURITY_CLASSIFICATION ( '', '', #26177 ) ;
#31349 = ORIENTED_EDGE ( 'NONE', *, *, #35580, .F. ) ;
#31350 = CARTESIAN_POINT ( 'NONE',  ( -1.040834085586084010E-16, 4.942613344993767655E-17, -0.07499999999999977518 ) ) ;
#31351 = CARTESIAN_POINT ( 'NONE',  ( 0.7432944383420270196, -1.516446101903487165, 0.5674244750120348568 ) ) ;
#31352 = CARTESIAN_POINT ( 'NONE',  ( 0.5947987396514448077, -1.485632953921246946, -0.6449812926602518370 ) ) ;
#31353 = CARTESIAN_POINT ( 'NONE',  ( -0.2399999999999999079, -4.134278792318540674, -0.4999285807449073693 ) ) ;
#31354 = DIRECTION ( 'NONE',  ( 0.4999551463232372317, -0.8660512985181134660, -6.869252350113302335E-17 ) ) ;
#31355 = CARTESIAN_POINT ( 'NONE',  ( 0.2684390043173380258, -1.673772033336743181, 0.5388446858685563834 ) ) ;
#31356 = LINE ( 'NONE', #37711, #38256 ) ;
#31357 = CARTESIAN_POINT ( 'NONE',  ( 0.5554409461590971153, -1.190971970253151824, 0.5682417262808781011 ) ) ;
#31358 = APPROVAL_STATUS ( 'not_yet_approved' ) ;
#31359 = CARTESIAN_POINT ( 'NONE',  ( 0.5908959048872449715, -1.601544548465861473, 0.4282886817583849703 ) ) ;
#31360 = FACE_OUTER_BOUND ( 'NONE', #32027, .T. ) ;
#31361 = CARTESIAN_POINT ( 'NONE',  ( -0.05187277790672430861, 0.01792103310037021849, 0.4704724753798314452 ) ) ;
#31362 = ADVANCED_FACE ( 'NONE', ( #28098, #3386 ), #12865, .F. ) ;
#31363 =( BOUNDED_SURFACE ( )  B_SPLINE_SURFACE ( 3, 2, ( 
 ( #22180, #37566, #18662 ),
 ( #37182, #12293, #15585 ),
 ( #28131, #3423, #18447 ),
 ( #30999, #21563, #25456 ),
 ( #34084, #2823, #15372 ),
 ( #27716, #28529, #18880 ),
 ( #27930, #6277, #24652 ),
 ( #18257, #40471, #30803 ),
 ( #2622, #9184, #8999 ),
 ( #31224, #37784, #24852 ) ),
 .UNSPECIFIED., .F., .F., .F. ) 
 B_SPLINE_SURFACE_WITH_KNOTS ( ( 4, 2, 2, 2, 4 ),
 ( 3, 3 ),
 ( 0.000000000000000000, 0.0005548957138909029006, 0.001109791427781805801, 0.001664687141672708702, 0.002219582855563611602 ),
 ( 0.000000000000000000, 1.000000000000000000 ),
 .UNSPECIFIED. ) 
 GEOMETRIC_REPRESENTATION_ITEM ( )  RATIONAL_B_SPLINE_SURFACE ( (
 ( 1.000000000000000000, 0.8164965809277185960, 1.000000000000000000),
 ( 1.000000000000000000, 0.8165294587845374208, 1.000000000000000000),
 ( 1.000000000000000000, 0.8155127232466478082, 1.000000000000000000),
 ( 1.000000000000000000, 0.8083607722978235488, 1.000000000000000000),
 ( 1.000000000000000000, 0.8021782943055887349, 1.000000000000000000),
 ( 1.000000000000000000, 0.7842736402517446193, 1.000000000000000000),
 ( 1.000000000000000000, 0.7723567727536417848, 1.000000000000000000),
 ( 1.000000000000000000, 0.7435640046126961167, 1.000000000000000000),
 ( 1.000000000000000000, 0.7266415285874683327, 1.000000000000000000),
 ( 1.000000000000000000, 0.7071067811843647632, 1.000000000000000000) ) ) 
 REPRESENTATION_ITEM ( '' )  SURFACE ( )  );
#31364 = VERTEX_POINT ( 'NONE', #36934 ) ;
#31365 = DIRECTION ( 'NONE',  ( 1.000000000000000000, 2.042862361497887782E-14, 7.734859593387037307E-16 ) ) ;
#31366 = CARTESIAN_POINT ( 'NONE',  ( -0.02872242845530528429, -0.2464193076120088921, 0.4721747535844859067 ) ) ;
#31367 = ADVANCED_FACE ( 'NONE', ( #34246 ), #361, .F. ) ;
#31368 = CARTESIAN_POINT ( 'NONE',  ( 0.1896960494042899126, -0.8386842184079319473, 0.2498764039407927462 ) ) ;
#31369 = ORIENTED_EDGE ( 'NONE', *, *, #8544, .F. ) ;
#31370 = CARTESIAN_POINT ( 'NONE',  ( -0.04047161733259106720, -0.06271464429809672780, -0.4973245071804597850 ) ) ;
#31371 = EDGE_CURVE ( 'NONE', #34187, #34796, #34051, .T. ) ;
#31372 = CARTESIAN_POINT ( 'NONE',  ( -0.01212677295819645021, -0.8635911836337304415, 0.3648026836272298401 ) ) ;
#31374 = EDGE_LOOP ( 'NONE', ( #899, #28829, #2402 ) ) ;
#31373 = VERTEX_POINT ( 'NONE', #22147 ) ;
#31375 = DIRECTION ( 'NONE',  ( 0.4999551463232373427, -0.8660512985181134660, 0.000000000000000000 ) ) ;
#31376 = DIRECTION ( 'NONE',  ( 1.000000000000000000, 1.113825344428167933E-31, -7.771561172376107616E-16 ) ) ;
#31377 = EDGE_CURVE ( 'NONE', #7253, #8899, #37337, .T. ) ;
#31378 = CARTESIAN_POINT ( 'NONE',  ( 0.3697297642830735809, -2.079360693035569696, -0.4724975067213835755 ) ) ;
#31380 = CARTESIAN_POINT ( 'NONE',  ( 0.006142123377964069098, -0.4287598720593460699, 0.1457185332388686305 ) ) ;
#31379 = CARTESIAN_POINT ( 'NONE',  ( 0.02881329448200726714, 0.4517642754607847921, 0.2100174381954101610 ) ) ;
#31381 = CARTESIAN_POINT ( 'NONE',  ( 0.02872242845529755437, -0.2464193076120163306, -0.4721747535845037258 ) ) ;
#31382 = ORIENTED_EDGE ( 'NONE', *, *, #27037, .T. ) ;
#31383 = CARTESIAN_POINT ( 'NONE',  ( 0.09080745303567185067, -0.5677619141264073077, 0.2083789338475214581 ) ) ;
#31384 = ORIENTED_EDGE ( 'NONE', *, *, #15580, .F. ) ;
#31385 = DIRECTION ( 'NONE',  ( 1.188678714063518227E-15, -1.000000000000000000, -3.263080277421930985E-16 ) ) ;
#31386 = CARTESIAN_POINT ( 'NONE',  ( 0.4413773429406284143, -1.573661458614751485, 0.5688663500546452534 ) ) ;
#31387 = EDGE_CURVE ( 'NONE', #15152, #17948, #12828, .T. ) ;
#31389 = CARTESIAN_POINT ( 'NONE',  ( 0.5667697670958626865, -1.627219054903903395, 0.5179411731989888024 ) ) ;
#31388 = CARTESIAN_POINT ( 'NONE',  ( 0.4894889402668303746, -1.607606434602806722, -0.3928725284401201612 ) ) ;
#31390 = CARTESIAN_POINT ( 'NONE',  ( 0.4511668698691140289, -1.684167190675012415, -0.7187326247832955817 ) ) ;
#31391 = CARTESIAN_POINT ( 'NONE',  ( 0.2352442375527352414, -0.9584679667894288047, 0.4983825088159561378 ) ) ;
#31392 = EDGE_CURVE ( 'NONE', #20992, #20650, #10584, .T. ) ;
#31393 = DIRECTION ( 'NONE',  ( 0.4999551463232372317, -0.8660512985181134660, 0.000000000000000000 ) ) ;
#31394 = EDGE_CURVE ( 'NONE', #4879, #20283, #18082, .T. ) ;
#31395 = CARTESIAN_POINT ( 'NONE',  ( 0.1153472994790071260, -0.4465945824750962023, 0.1471405910905037306 ) ) ;
#31396 = CARTESIAN_POINT ( 'NONE',  ( 0.5807592067643548850, -1.495225062396434046, 0.5704271586488920409 ) ) ;
#31397 = CARTESIAN_POINT ( 'NONE',  ( -0.03170752374382516253, 0.3312811549923315169, -0.3635342706644930089 ) ) ;
#31398 = CYLINDRICAL_SURFACE ( 'NONE', #8699, 0.07999999999999996003 ) ;
#31399 = DIRECTION ( 'NONE',  ( 0.000000000000000000, 0.000000000000000000, -1.000000000000000000 ) ) ;
#31400 = DIRECTION ( 'NONE',  ( -1.387778780781449423E-15, 6.590151126658375938E-16, -1.000000000000000000 ) ) ;
#31401 = CARTESIAN_POINT ( 'NONE',  ( 2.762449479338929480E-16, -0.02999999999999982889, 0.1849999999999999978 ) ) ;
#31402 = CARTESIAN_POINT ( 'NONE',  ( 0.6810725650087121608, -1.407094454800211558, 0.5876998678990568159 ) ) ;
#31403 = CARTESIAN_POINT ( 'NONE',  ( -0.01548846960707460536, 0.3688619771572935746, 0.3775276577326980854 ) ) ;
#31404 = CARTESIAN_POINT ( 'NONE',  ( 0.02344934057377633801, -1.099133950262376258, 0.6397433352409148677 ) ) ;
#31405 = CARTESIAN_POINT ( 'NONE',  ( 0.6239059973579713647, -1.614399174532030523, -0.4690470541687177808 ) ) ;
#31406 = CARTESIAN_POINT ( 'NONE',  ( -0.2399999999999999079, -3.747168848490688209, -0.4747258284076885104 ) ) ;
#31407 = CARTESIAN_POINT ( 'NONE',  ( 0.07670936359779292890, -0.8423313109294351397, 0.3268936787692559576 ) ) ;
#31408 = CARTESIAN_POINT ( 'NONE',  ( 0.2663522331702417034, -1.675380074340676151, 0.5698030654214122359 ) ) ;
#31409 = CARTESIAN_POINT ( 'NONE',  ( 0.09912479720125623450, -1.266807960652112097, 0.5182417262812423209 ) ) ;
#31410 = ORIENTED_EDGE ( 'NONE', *, *, #25582, .F. ) ;
#31411 = DIRECTION ( 'NONE',  ( 0.000000000000000000, 0.000000000000000000, -1.000000000000000000 ) ) ;
#31412 = CARTESIAN_POINT ( 'NONE',  ( 0.4879523740783364150, -1.280237457375205334, 0.7926971813901000363 ) ) ;
#31413 = CARTESIAN_POINT ( 'NONE',  ( 0.3660745003390204477, -2.015859508080472207, -0.4732687194387362739 ) ) ;
#31414 = EDGE_CURVE ( 'NONE', #9135, #7249, #1301, .T. ) ;
#31415 = CARTESIAN_POINT ( 'NONE',  ( 0.08510361377861434817, -0.8106636051554854117, 0.1454306519311501233 ) ) ;
#31416 = FACE_OUTER_BOUND ( 'NONE', #21198, .T. ) ;
#31417 = ADVANCED_FACE ( 'NONE', ( #9569 ), #3000, .F. ) ;
#31418 = ORIENTED_EDGE ( 'NONE', *, *, #39910, .T. ) ;
#31419 = DIRECTION ( 'NONE',  ( 1.000000000000000000, 0.000000000000000000, 0.000000000000000000 ) ) ;
#31420 = CARTESIAN_POINT ( 'NONE',  ( 0.1156610620243726933, -1.416230906443656901, 0.4172996703284162501 ) ) ;
#31421 = CARTESIAN_POINT ( 'NONE',  ( 2.058600446713667573E-16, 0.2900000000000004796, -0.01750000000000052902 ) ) ;
#31422 = CARTESIAN_POINT ( 'NONE',  ( 0.03474878377840454752, 0.2421023663934840364, -0.4562919991932258279 ) ) ;
#31423 = CARTESIAN_POINT ( 'NONE',  ( 0.3785755849098691450, -1.119414945699769959, 0.7435571456696157266 ) ) ;
#31424 = CARTESIAN_POINT ( 'NONE',  ( 0.5144487370624802880, -1.604612665234552926, -0.6158392069828952931 ) ) ;
#31425 = CARTESIAN_POINT ( 'NONE',  ( 0.4790383449168201802, -1.075084602395082634, 0.6124719440393814329 ) ) ;
#31426 = ORIENTED_EDGE ( 'NONE', *, *, #12176, .T. ) ;
#31427 = PRODUCT_CONTEXT ( 'NONE', #7424, 'mechanical' ) ;
#31428 = CIRCLE ( 'NONE', #581, 0.009999999999999995004 ) ;
#31429 = CARTESIAN_POINT ( 'NONE',  ( 0.08062789043467089023, -1.253025610042452831, 0.7448910529509513712 ) ) ;
#31430 = ORIENTED_EDGE ( 'NONE', *, *, #34936, .T. ) ;
#31431 = CARTESIAN_POINT ( 'NONE',  ( 0.3843449031254181913, -1.605279702831362787, 0.5608835269958394321 ) ) ;
#31433 = CARTESIAN_POINT ( 'NONE',  ( 0.1116987077102032100, -0.8808449370242167342, 0.0008922463578378222755 ) ) ;
#31432 = CARTESIAN_POINT ( 'NONE',  ( 0.06455621155043581028, -0.8342858573599853944, 0.1261830515498010841 ) ) ;
#31434 = CARTESIAN_POINT ( 'NONE',  ( 0.06705167635834106965, -0.6680383592416772043, -0.0009537033254834985244 ) ) ;
#31435 = VERTEX_POINT ( 'NONE', #21324 ) ;
#31436 = VERTEX_POINT ( 'NONE', #19036 ) ;
#31437 = ORIENTED_EDGE ( 'NONE', *, *, #39085, .T. ) ;
#31438 = CYLINDRICAL_SURFACE ( 'NONE', #39207, 0.1033070866141734129 ) ;
#31439 = CARTESIAN_POINT ( 'NONE',  ( 0.5282826409240604093, -1.443108049827171335, 0.7657529498032049631 ) ) ;
#31440 = ORIENTED_EDGE ( 'NONE', *, *, #24615, .F. ) ;
#31441 = CARTESIAN_POINT ( 'NONE',  ( 0.1853053032850285331, -0.8367218493003313329, 0.1362433201977383268 ) ) ;
#31442 = CARTESIAN_POINT ( 'NONE',  ( -0.004906298587631130297, -2.039712202718448442, -0.3118752401674445007 ) ) ;
#31443 = FACE_BOUND ( 'NONE', #13133, .T. ) ;
#31444 = CARTESIAN_POINT ( 'NONE',  ( 0.6630839938131345423, -1.446213159395746128, -0.6155857397476032222 ) ) ;
#31445 = CARTESIAN_POINT ( 'NONE',  ( 0.2647196283856586563, -1.647466429234020646, -0.3433666575725142223 ) ) ;
#31446 = CARTESIAN_POINT ( 'NONE',  ( 0.3335364369457424760, -1.652728420514769425, -0.6442615712401940087 ) ) ;
#31447 = DIRECTION ( 'NONE',  ( -0.4999551463232372317, 0.8660512985181135770, -0.000000000000000000 ) ) ;
#31448 = CARTESIAN_POINT ( 'NONE',  ( 0.4019696390288734489, -1.758754468419369221, -0.5306525527942117515 ) ) ;
#31449 = CARTESIAN_POINT ( 'NONE',  ( 0.1525961459700538314, -1.248272379099432339, 0.6216296366653764061 ) ) ;
#31450 = DIRECTION ( 'NONE',  ( 0.5682870691672845531, 0.000000000000000000, -0.8228303634512146303 ) ) ;
#31451 = CARTESIAN_POINT ( 'NONE',  ( -0.02000000000000000042, -1.599201040860868339, 0.2442182323853691606 ) ) ;
#31452 = PERSON_AND_ORGANIZATION ( #28500, #32463 ) ;
#31453 = CARTESIAN_POINT ( 'NONE',  ( 0.4162441775219429263, -1.040631601589554034, 0.6343403631529308528 ) ) ;
#31454 = CARTESIAN_POINT ( 'NONE',  ( 0.3121344959780879558, -1.175754444927441300, 0.5182417262812437642 ) ) ;
#31455 = DIRECTION ( 'NONE',  ( -0.0001066307966867950538, 1.551735798909011778E-06, 0.9999999943137325431 ) ) ;
#31457 = ORIENTED_EDGE ( 'NONE', *, *, #27603, .F. ) ;
#31456 = CARTESIAN_POINT ( 'NONE',  ( 0.3229289876128840775, -1.169687821100875658, 0.5631135379446852163 ) ) ;
#31458 = CARTESIAN_POINT ( 'NONE',  ( 0.006005486288604863949, -0.9514584861060970677, 0.4879672165010910390 ) ) ;
#31459 = CARTESIAN_POINT ( 'NONE',  ( 0.0003079261067442713869, -0.4760981469167980817, 0.01389499447167343027 ) ) ;
#31460 = LINE ( 'NONE', #3267, #2211 ) ;
#31461 = CARTESIAN_POINT ( 'NONE',  ( 0.3556570129879135789, -1.173715053083399740, 0.4182417262808778013 ) ) ;
#31462 = ORIENTED_EDGE ( 'NONE', *, *, #38971, .T. ) ;
#31463 = ORIENTED_EDGE ( 'NONE', *, *, #1219, .T. ) ;
#31464 = CARTESIAN_POINT ( 'NONE',  ( 0.03650581953630544635, -0.3643937567481972950, -0.3592734714612038638 ) ) ;
#31465 = ORIENTED_EDGE ( 'NONE', *, *, #9484, .T. ) ;
#31466 = FACE_OUTER_BOUND ( 'NONE', #15037, .T. ) ;
#31467 = CARTESIAN_POINT ( 'NONE',  ( 0.04229956186878620905, 0.2683474741743152592, 0.3842687663629376082 ) ) ;
#31468 = CARTESIAN_POINT ( 'NONE',  ( 0.5741579611739540123, -1.419304924894309927, 0.6377566456345815649 ) ) ;
#31470 = ORIENTED_EDGE ( 'NONE', *, *, #23188, .T. ) ;
#31469 = CARTESIAN_POINT ( 'NONE',  ( 0.001493246241084611415, -0.5596943232668920576, 0.04990435613214081606 ) ) ;
#31471 = ORIENTED_EDGE ( 'NONE', *, *, #39294, .T. ) ;
#31472 = CARTESIAN_POINT ( 'NONE',  ( 0.2004046765218066295, -0.7505902666037495008, 0.3314731723568724586 ) ) ;
#31473 = ORIENTED_EDGE ( 'NONE', *, *, #11667, .T. ) ;
#31474 = CARTESIAN_POINT ( 'NONE',  ( 0.01468336712996881274, -0.5833551626382605937, 0.3318062457441503521 ) ) ;
#31476 = CARTESIAN_POINT ( 'NONE',  ( 0.2948777445940948261, -1.312432472972675290, 0.4182417262808776348 ) ) ;
#31475 = CARTESIAN_POINT ( 'NONE',  ( 0.4226721025871904014, -1.212929281597423525, 0.6550521210678496020 ) ) ;
#31477 = CARTESIAN_POINT ( 'NONE',  ( -0.2300000000000000655, 0.5182417262804733804, 0.3749999999999999445 ) ) ;
#31478 = CARTESIAN_POINT ( 'NONE',  ( 0.01194082430585321694, -0.5163470803647776108, -0.04948302235635338581 ) ) ;
#31479 = DIRECTION ( 'NONE',  ( 1.000000000000000000, 0.000000000000000000, 0.000000000000000000 ) ) ;
#31481 = ORIENTED_EDGE ( 'NONE', *, *, #791, .F. ) ;
#31480 = EDGE_LOOP ( 'NONE', ( #27578, #7538, #32171, #34606, #3552, #29122, #15729 ) ) ;
#31482 = CARTESIAN_POINT ( 'NONE',  ( 0.4688459138424371786, -1.061988423737608045, -0.4248180574663140141 ) ) ;
#31483 = CIRCLE ( 'NONE', #19003, 0.01500000000000000291 ) ;
#31484 = CARTESIAN_POINT ( 'NONE',  ( 0.1862143093560909568, -0.9153542374866630027, 0.1397141703224119846 ) ) ;
#31485 = CARTESIAN_POINT ( 'NONE',  ( -0.03474824846560085195, -0.5087747035359800885, 0.08925086559847709988 ) ) ;
#31486 = CARTESIAN_POINT ( 'NONE',  ( 0.5578360211051590634, -1.391431592590435251, 0.7485196725347594837 ) ) ;
#31487 = CARTESIAN_POINT ( 'NONE',  ( 0.1943267261999117590, -0.8912486778694943546, 0.5787461573889725042 ) ) ;
#31488 = CARTESIAN_POINT ( 'NONE',  ( 0.2693423574607928805, -1.623096489475305271, 0.8033103420475437018 ) ) ;
#31489 = CARTESIAN_POINT ( 'NONE',  ( 0.2357496974250468946, -1.376590845310902145, 1.030782602123143876 ) ) ;
#31490 = DIRECTION ( 'NONE',  ( 2.532366176626906196E-12, 0.3090169943749446757, -0.9510565162951545304 ) ) ;
#31491 = CARTESIAN_POINT ( 'NONE',  ( 0.6059691746655119227, -1.480133143157562170, 0.5526975506195443977 ) ) ;
#31492 = CARTESIAN_POINT ( 'NONE',  ( 0.3722391882570431632, -1.729214173715589720, -0.4195648250677492808 ) ) ;
#31493 = CARTESIAN_POINT ( 'NONE',  ( 0.04047043078436834973, -0.3430608037303031765, 0.3654822131371281979 ) ) ;
#31494 = CARTESIAN_POINT ( 'NONE',  ( -0.09579104668929026845, -0.04310840302198015034, 0.08499999999999910405 ) ) ;
#31495 = CARTESIAN_POINT ( 'NONE',  ( 0.08953535957268946022, -1.239962282013243877, 0.7545938977955062299 ) ) ;
#31496 = CALENDAR_DATE ( 2026, 13, 10 ) ;
#31497 = CARTESIAN_POINT ( 'NONE',  ( -0.02953079040095606816, 0.4684706630666136684, 0.2484463060367380904 ) ) ;
#31498 = CARTESIAN_POINT ( 'NONE',  ( 0.6937844480354340426, -1.537461556741912760, 0.5870152100781083071 ) ) ;
#31499 = EDGE_CURVE ( 'NONE', #40356, #2485, #21405, .T. ) ;
#31500 = CARTESIAN_POINT ( 'NONE',  ( -0.3000000000000000999, -2.511040369707300268, -0.5948468226404902692 ) ) ;
#31501 = ORIENTED_EDGE ( 'NONE', *, *, #35816, .F. ) ;
#31502 = CARTESIAN_POINT ( 'NONE',  ( 0.2709623010280027278, -1.672610760848568967, 0.4891849873696615392 ) ) ;
#31503 = APPROVAL ( #26831, 'UNKNOWN' ) ;
#31504 = CARTESIAN_POINT ( 'NONE',  ( 0.2662581717953377836, -1.658323607150117285, 0.7400210192072117499 ) ) ;
#31506 = ORIENTED_EDGE ( 'NONE', *, *, #11893, .T. ) ;
#31505 = CARTESIAN_POINT ( 'NONE',  ( 0.5820653343257259360, -1.465606132385127935, 0.6997249523535519211 ) ) ;
#31508 = VERTEX_POINT ( 'NONE', #2788 ) ;
#31507 = CARTESIAN_POINT ( 'NONE',  ( 0.3499317094845075249, -1.754137739073151181, 0.4513909310129907704 ) ) ;
#31510 = ORIENTED_EDGE ( 'NONE', *, *, #11241, .T. ) ;
#31509 = ORIENTED_EDGE ( 'NONE', *, *, #27739, .F. ) ;
#31511 = CARTESIAN_POINT ( 'NONE',  ( 0.1399999999999994582, -6.554815759418801904E-17, -0.2526340763130725531 ) ) ;
#31512 = CARTESIAN_POINT ( 'NONE',  ( 0.1109092093543055241, -0.9286325583098424818, 0.1457252011008478843 ) ) ;
#31513 = DIRECTION ( 'NONE',  ( 0.4999999999999990008, 0.5755298573121164774, -0.6471208413753150035 ) ) ;
#31514 = SECURITY_CLASSIFICATION_LEVEL ( 'unclassified' ) ;
#31515 = CARTESIAN_POINT ( 'NONE',  ( 0.3409152363046567547, -1.516880185093696154, -0.5318766032426672785 ) ) ;
#31516 = ORIENTED_EDGE ( 'NONE', *, *, #2387, .F. ) ;
#31517 = CARTESIAN_POINT ( 'NONE',  ( 0.1035168011811207489, -0.7883913148987408137, 0.3594284199549346304 ) ) ;
#31518 = CARTESIAN_POINT ( 'NONE',  ( 0.4120574151838698462, -1.590911390411421156, -0.3441652514538682817 ) ) ;
#31519 = CARTESIAN_POINT ( 'NONE',  ( 0.1042374422282348334, -0.5569725106795370140, 0.2106683946891434178 ) ) ;
#31520 = ADVANCED_FACE ( 'NONE', ( #40430 ), #15730, .T. ) ;
#31521 = DIRECTION ( 'NONE',  ( 0.000000000000000000, 0.000000000000000000, -1.000000000000000000 ) ) ;
#31522 = CARTESIAN_POINT ( 'NONE',  ( -0.1583356623530634000, 0.4914777262839043481, 0.1012105261661027239 ) ) ;
#31523 = ORIENTED_EDGE ( 'NONE', *, *, #3621, .F. ) ;
#31524 = CARTESIAN_POINT ( 'NONE',  ( 0.4153535842760917585, -1.704503823779182081, 0.6190792889780868391 ) ) ;
#31525 = B_SPLINE_CURVE_WITH_KNOTS ( 'NONE', 3,
 ( #10554, #7677, #23129, #20242, #38940, #1529 ),
 .UNSPECIFIED., .F., .F.,
 ( 4, 2, 4 ),
 ( 0.000000000000000000, 0.0006315621964318843306, 0.001263124392863768661 ),
 .UNSPECIFIED. ) ;
#31526 = CARTESIAN_POINT ( 'NONE',  ( 0.6984060551207101897, -1.438828591659085054, 0.5657311187875787573 ) ) ;
#31527 = ADVANCED_FACE ( 'NONE', ( #34856 ), #29502, .F. ) ;
#31528 = CARTESIAN_POINT ( 'NONE',  ( -0.2399999999999999079, -3.384162466027138105, -0.4389494074304161608 ) ) ;
#31529 = EDGE_CURVE ( 'NONE', #24330, #17955, #19240, .T. ) ;
#31530 = CARTESIAN_POINT ( 'NONE',  ( 0.1820744924655830210, -0.7238696534340168798, 0.5246764128789646042 ) ) ;
#31531 = CARTESIAN_POINT ( 'NONE',  ( 0.1927077495703349852, -0.8180328145591141409, 0.2791508387892263077 ) ) ;
#31532 = ADVANCED_FACE ( 'NONE', ( #22538 ), #158, .T. ) ;
#31533 = CARTESIAN_POINT ( 'NONE',  ( 0.05560027925352286488, -1.335209592177159843, 0.5707417262808780478 ) ) ;
#31534 = CARTESIAN_POINT ( 'NONE',  ( 0.04229956186878621599, -0.4429651807893704718, -0.1531492745855136950 ) ) ;
#31535 = EDGE_CURVE ( 'NONE', #11782, #31436, #34197, .T. ) ;
#31536 = CARTESIAN_POINT ( 'NONE',  ( 0.05086546246741921462, -1.198860143930047473, 0.7015125153497857591 ) ) ;
#31537 = CARTESIAN_POINT ( 'NONE',  ( 0.2067623920994063613, -0.8133810345767992223, 0.3693416354660131184 ) ) ;
#31538 = SHAPE_DEFINITION_REPRESENTATION ( #26894, #31708 ) ;
#31539 = DIRECTION ( 'NONE',  ( -1.000000000000000000, 0.000000000000000000, -7.762644838731319154E-16 ) ) ;
#31540 = DIRECTION ( 'NONE',  ( 0.4999999999999991118, 0.2433878240179132291, 0.8311211506873266153 ) ) ;
#31541 = CARTESIAN_POINT ( 'NONE',  ( -0.04308449196698887346, -0.05688586270224561120, 0.4910287377915159568 ) ) ;
#31542 = EDGE_CURVE ( 'NONE', #22988, #10878, #27634, .T. ) ;
#31543 = ORIENTED_EDGE ( 'NONE', *, *, #26401, .T. ) ;
#31544 = CARTESIAN_POINT ( 'NONE',  ( 0.2133635201206025567, -1.295927705172547739, -0.4087570219343043543 ) ) ;
#31545 = DIRECTION ( 'NONE',  ( 0.4999551463232372317, -0.8660512985181135770, 0.000000000000000000 ) ) ;
#31546 = AXIS2_PLACEMENT_3D ( 'NONE', #6359, #32250, #28971 ) ;
#31547 = CARTESIAN_POINT ( 'NONE',  ( 0.08805730728144700592, -0.6472740652894640734, 0.02916467596460211448 ) ) ;
#31548 = EDGE_LOOP ( 'NONE', ( #10774, #37742, #33188, #18043 ) ) ;
#31549 = CARTESIAN_POINT ( 'NONE',  ( 0.2319960710055803677, -1.232736008543062090, 0.4687417262808780127 ) ) ;
#31550 = CARTESIAN_POINT ( 'NONE',  ( 0.01072073033491486443, -0.9808573846632955284, 0.6679598757981023427 ) ) ;
#31552 = ORIENTED_EDGE ( 'NONE', *, *, #6663, .T. ) ;
#31551 = EDGE_LOOP ( 'NONE', ( #32869, #7296 ) ) ;
#31553 = CARTESIAN_POINT ( 'NONE',  ( -0.1126900943574667274, -0.5191528599708484792, 0.1528658435936963711 ) ) ;
#31554 = VECTOR ( 'NONE', #19386, 39.37007874015748854 ) ;
#31555 = ORIENTED_EDGE ( 'NONE', *, *, #28021, .T. ) ;
#31556 = CARTESIAN_POINT ( 'NONE',  ( 0.4178394282659816938, -1.669152271385904607, -0.5063121030242170306 ) ) ;
#31558 = CARTESIAN_POINT ( 'NONE',  ( 0.01548846960707524721, 0.3772621329473435647, -0.3651003739302673967 ) ) ;
#31557 = CARTESIAN_POINT ( 'NONE',  ( 0.03301200226530935644, 0.4610556019031807895, 0.2426442821263211647 ) ) ;
#31559 = DIRECTION ( 'NONE',  ( 0.4999551463232372317, -0.8660512985181135770, 0.000000000000000000 ) ) ;
#31560 = EDGE_LOOP ( 'NONE', ( #22332, #25761, #33922, #40063, #24454 ) ) ;
#31561 = CARTESIAN_POINT ( 'NONE',  ( -0.2399999999999999079, -3.094053300116982985, 0.06803269733885447534 ) ) ;
#31562 = EDGE_LOOP ( 'NONE', ( #5716, #2548, #2887, #36081 ) ) ;
#31563 = EDGE_LOOP ( 'NONE', ( #651, #9816, #31369, #33687 ) ) ;
#31564 = CARTESIAN_POINT ( 'NONE',  ( 0.09119287031673356525, -0.6099748663625392808, 0.2139121366898841525 ) ) ;
#31565 = EDGE_LOOP ( 'NONE', ( #11590, #25303, #11086 ) ) ;
#31566 = ORIENTED_EDGE ( 'NONE', *, *, #17975, .T. ) ;
#31567 = DIRECTION ( 'NONE',  ( 1.000000000000000000, 2.341930812374887555E-31, -1.664003471950578127E-31 ) ) ;
#31568 = CARTESIAN_POINT ( 'NONE',  ( 0.2024955851830932685, -0.9687359790435555729, 0.7686808776775244656 ) ) ;
#31570 = DIRECTION ( 'NONE',  ( 0.5794373887239150367, -0.8150167559926670968, 2.848458103903287201E-16 ) ) ;
#31569 = CARTESIAN_POINT ( 'NONE',  ( 0.4708300887478357732, -1.591450557125715148, -0.4363017091322234364 ) ) ;
#31571 = FACE_OUTER_BOUND ( 'NONE', #14300, .T. ) ;
#31572 = CARTESIAN_POINT ( 'NONE',  ( 0.1938692902500353255, -0.9317700634581833619, 0.3727138502448550383 ) ) ;
#31573 = ORIENTED_EDGE ( 'NONE', *, *, #25336, .F. ) ;
#31574 = DIRECTION ( 'NONE',  ( -0.4999551463232373427, 0.8660512985181134660, -0.000000000000000000 ) ) ;
#31575 = B_SPLINE_CURVE_WITH_KNOTS ( 'NONE', 3,
 ( #8822, #27964, #12326, #24884, #3673, #6739 ),
 .UNSPECIFIED., .F., .F.,
 ( 4, 2, 4 ),
 ( 0.001507239257244120598, 0.001922639214874271663, 0.002338039172504422728 ),
 .UNSPECIFIED. ) ;
#31576 = CARTESIAN_POINT ( 'NONE',  ( 0.1153481622643483390, -0.4466190433387221548, 0.1494994773299645197 ) ) ;
#31577 = CARTESIAN_POINT ( 'NONE',  ( 0.1281471506186622478, -0.5867175007372630313, 0.2851988856149638707 ) ) ;
#31578 = CARTESIAN_POINT ( 'NONE',  ( -0.05076541221973554507, 0.3165406372985248851, -0.3525330185552898454 ) ) ;
#31579 = EDGE_CURVE ( 'NONE', #11533, #24870, #27958, .T. ) ;
#31580 = FACE_BOUND ( 'NONE', #21471, .T. ) ;
#31581 = CARTESIAN_POINT ( 'NONE',  ( -0.01548846960707375361, -0.4730347584886793189, -0.2341461249029842817 ) ) ;
#31582 = ADVANCED_FACE ( 'NONE', ( #9303 ), #39575, .T. ) ;
#31583 = AXIS2_PLACEMENT_3D ( 'NONE', #36525, #25195, #557 ) ;
#31584 = CARTESIAN_POINT ( 'NONE',  ( 0.06924866487494936440, -0.5400458411302934136, 0.1497098795544565819 ) ) ;
#31585 = DIRECTION ( 'NONE',  ( 0.000000000000000000, -0.5914787413272157846, -0.8063205929144887651 ) ) ;
#31586 = ADVANCED_FACE ( 'NONE', ( #18574 ), #30560, .T. ) ;
#31587 = CARTESIAN_POINT ( 'NONE',  ( 0.3418186750811026964, -0.8703758711135023418, 0.7017026408156415984 ) ) ;
#31588 = AXIS2_PLACEMENT_3D ( 'NONE', #1431, #30192, #14157 ) ;
#31589 =( BOUNDED_SURFACE ( )  B_SPLINE_SURFACE ( 3, 2, ( 
 ( #29146, #13104, #1012 ),
 ( #16601, #25664, #32030 ),
 ( #38004, #38198, #13309 ),
 ( #38400, #35328, #10023 ),
 ( #22986, #22593, #7534 ),
 ( #6928, #7313, #19501 ),
 ( #19683, #32218, #10425 ),
 ( #4036, #13524, #26086 ),
 ( #38605, #35505, #4249 ),
 ( #13706, #16817, #1203 ),
 ( #10622, #23198, #32640 ),
 ( #24209, #11447, #36733 ),
 ( #8541, #5055, #21111 ),
 ( #39008, #36120, #23803 ),
 ( #24014, #17412, #39827 ),
 ( #11650, #29752, #36540 ) ),
 .UNSPECIFIED., .F., .F., .T. ) 
 B_SPLINE_SURFACE_WITH_KNOTS ( ( 4, 2, 2, 2, 2, 2, 2, 4 ),
 ( 3, 3 ),
 ( 0.000000000000000000, 0.0008227173377846956582, 0.001645434675569391316, 0.002468152013354086866, 0.003290869351138782633, 0.004113586688923477966, 0.004936304026708173733, 0.006581738702277565266 ),
 ( 0.000000000000000000, 1.000000000000000000 ),
 .UNSPECIFIED. ) 
 GEOMETRIC_REPRESENTATION_ITEM ( )  RATIONAL_B_SPLINE_SURFACE ( (
 ( 1.000000000000000000, 0.9337218516597696194, 1.000000000000000000),
 ( 1.000000000000000000, 0.9361136716705305005, 1.000000000000000000),
 ( 1.000000000000000000, 0.9384872499382632682, 1.000000000000000000),
 ( 1.000000000000000000, 0.9429186473287669568, 1.000000000000000000),
 ( 1.000000000000000000, 0.9449938870051080020, 1.000000000000000000),
 ( 1.000000000000000000, 0.9484294354700106844, 1.000000000000000000),
 ( 1.000000000000000000, 0.9497728432793278719, 1.000000000000000000),
 ( 1.000000000000000000, 0.9515742818507496592, 1.000000000000000000),
 ( 1.000000000000000000, 0.9520286448580135286, 1.000000000000000000),
 ( 1.000000000000000000, 0.9520600083455192930, 1.000000000000000000),
 ( 1.000000000000000000, 0.9516561831818339812, 1.000000000000000000),
 ( 1.000000000000000000, 0.9502672014312925075, 1.000000000000000000),
 ( 1.000000000000000000, 0.9492778443961910062, 1.000000000000000000),
 ( 1.000000000000000000, 0.9459276863539570757, 1.000000000000000000),
 ( 1.000000000000000000, 0.9431151263514566674, 1.000000000000000000),
 ( 1.000000000000000000, 0.9405852554627032180, 1.000000000000000000) ) ) 
 REPRESENTATION_ITEM ( '' )  SURFACE ( )  );
#31590 = CARTESIAN_POINT ( 'NONE',  ( 0.4469149852457636185, -1.151100400589097239, 0.3906371383882983328 ) ) ;
#31591 = CARTESIAN_POINT ( 'NONE',  ( 0.03048720409776598320, -1.144242443753076932, 0.6605958360182316857 ) ) ;
#31592 = CIRCLE ( 'NONE', #4005, 0.1700000000000000400 ) ;
#31593 = CIRCLE ( 'NONE', #25679, 0.009999999999999925615 ) ;
#31594 = CARTESIAN_POINT ( 'NONE',  ( 0.5958209082783288979, -1.583864344932945478, -0.4282463924674004274 ) ) ;
#31595 = CARTESIAN_POINT ( 'NONE',  ( 0.3999999999999786504, -2.092100694519134052, -0.4698241118115154547 ) ) ;
#31596 = CARTESIAN_POINT ( 'NONE',  ( 0.05999999999999990757, -0.3497707857934448938, -0.3763954645181781244 ) ) ;
#31597 = CARTESIAN_POINT ( 'NONE',  ( 0.1443375672974070711, 0.05141091571461162829, 0.000000000000000000 ) ) ;
#31598 = DIRECTION ( 'NONE',  ( 4.410796239770416717E-15, -0.9901182710308658041, -0.1402348365095101024 ) ) ;
#31599 = ADVANCED_FACE ( 'NONE', ( #15499 ), #31958, .F. ) ;
#31600 = ORIENTED_EDGE ( 'NONE', *, *, #10693, .T. ) ;
#31601 = FACE_OUTER_BOUND ( 'NONE', #22439, .T. ) ;
#31602 = CARTESIAN_POINT ( 'NONE',  ( 0.3909945020765858148, -1.648962484502373149, -0.3938746075551732839 ) ) ;
#31603 = CARTESIAN_POINT ( 'NONE',  ( 0.6568168296554719454, -1.515518412142557558, 0.4182417262808776903 ) ) ;
#31604 = LINE ( 'NONE', #31814, #30329 ) ;
#31605 = CARTESIAN_POINT ( 'NONE',  ( -0.04582705327698315817, -0.06484491888962914952, 0.4826014279685451047 ) ) ;
#31606 = ADVANCED_FACE ( 'NONE', ( #28438 ), #34524, .T. ) ;
#31607 = B_SPLINE_CURVE_WITH_KNOTS ( 'NONE', 3,
 ( #22662, #25727, #26151, #38858, #6785, #35196 ),
 .UNSPECIFIED., .F., .F.,
 ( 4, 2, 4 ),
 ( 0.1257255050569696386, 0.5628627525284848332, 1.000000000000000000 ),
 .UNSPECIFIED. ) ;
#31608 = VERTEX_POINT ( 'NONE', #29258 ) ;
#31609 = CARTESIAN_POINT ( 'NONE',  ( 0.4130089464348675188, -1.611935647216347300, -0.6680384904433120941 ) ) ;
#31610 = CARTESIAN_POINT ( 'NONE',  ( 0.1499999999999994671, -0.5203207976467941753, 0.08861466064782175245 ) ) ;
#31611 = DIRECTION ( 'NONE',  ( 0.000000000000000000, 0.000000000000000000, -1.000000000000000000 ) ) ;
#31612 = CARTESIAN_POINT ( 'NONE',  ( 0.05561310505366983542, 0.2871713500421194110, -0.3605322861779143295 ) ) ;
#31613 = CARTESIAN_POINT ( 'NONE',  ( 0.5014444851153065930, -1.296109412195814548, 0.5893235223995025862 ) ) ;
#31614 = AXIS2_PLACEMENT_3D ( 'NONE', #7, #34097, #5899 ) ;
#31616 = CARTESIAN_POINT ( 'NONE',  ( 0.3182134860132462828, -1.756684620118125206, 0.4922052827999418012 ) ) ;
#31615 = FACE_OUTER_BOUND ( 'NONE', #7528, .T. ) ;
#31617 = CARTESIAN_POINT ( 'NONE',  ( 0.4544126380536514520, -1.061573323663441704, 0.6302127423442334120 ) ) ;
#31618 = VERTEX_POINT ( 'NONE', #23096 ) ;
#31619 = APPROVAL_ROLE ( '' ) ;
#31620 = CIRCLE ( 'NONE', #27604, 0.1000000000000000194 ) ;
#31621 = DIRECTION ( 'NONE',  ( 0.000000000000000000, 0.000000000000000000, -1.000000000000000000 ) ) ;
#31622 = VERTEX_POINT ( 'NONE', #7217 ) ;
#31623 = CIRCLE ( 'NONE', #17813, 0.01000000000000002970 ) ;
#31624 = CARTESIAN_POINT ( 'NONE',  ( 0.3848986351367806868, -1.605492212228826876, 0.5691465893987337488 ) ) ;
#31626 = CARTESIAN_POINT ( 'NONE',  ( 0.1757587063316443377, -0.7188061800751018859, -0.08258769630449679100 ) ) ;
#31625 = CARTESIAN_POINT ( 'NONE',  ( 0.08657002633575118511, -0.7500003421022021222, 0.03948150975026209347 ) ) ;
#31627 = CARTESIAN_POINT ( 'NONE',  ( 0.06682908180107070828, -0.6872203660146791737, -0.001923513761143209400 ) ) ;
#31628 = CIRCLE ( 'NONE', #39428, 0.04330708661417322775 ) ;
#31629 = ORIENTED_EDGE ( 'NONE', *, *, #7210, .T. ) ;
#31630 = VECTOR ( 'NONE', #20430, 39.37007874015748143 ) ;
#31631 = EDGE_LOOP ( 'NONE', ( #4776, #37229, #23254, #6754 ) ) ;
#31632 = ORIENTED_EDGE ( 'NONE', *, *, #15028, .F. ) ;
#31633 = DIRECTION ( 'NONE',  ( 0.000000000000000000, 0.000000000000000000, -1.000000000000000000 ) ) ;
#31634 = CARTESIAN_POINT ( 'NONE',  ( 0.1210244766436220920, -0.5944767803591236577, 0.3087138919969779627 ) ) ;
#31635 = VERTEX_POINT ( 'NONE', #13203 ) ;
#31636 = CARTESIAN_POINT ( 'NONE',  ( 0.01730070817424270158, -0.9840727812340169800, 0.4636228551657111674 ) ) ;
#31637 = CARTESIAN_POINT ( 'NONE',  ( 0.1115022060487694811, -1.514603223676135757, -0.3697424615991000696 ) ) ;
#31638 = CARTESIAN_POINT ( 'NONE',  ( -0.01548846960707524721, 0.000000000000000000, 0.000000000000000000 ) ) ;
#31639 = LINE ( 'NONE', #19306, #14575 ) ;
#31640 = CARTESIAN_POINT ( 'NONE',  ( 0.4351293263873937667, -1.231514889939106849, 0.5832342842089121016 ) ) ;
#31641 = ADVANCED_FACE ( 'NONE', ( #3939 ), #708, .T. ) ;
#31642 = CARTESIAN_POINT ( 'NONE',  ( 0.1909286924077255032, -1.257064795538239022, -0.2869361388274795921 ) ) ;
#31643 = CARTESIAN_POINT ( 'NONE',  ( 0.08588225126352896921, -0.7695447752400129682, 0.06148066954598682687 ) ) ;
#31644 = DIRECTION ( 'NONE',  ( -1.188678714063518227E-15, 1.000000000000000000, 3.263080277421930985E-16 ) ) ;
#31645 = FACE_OUTER_BOUND ( 'NONE', #16349, .T. ) ;
#31646 = DIRECTION ( 'NONE',  ( -0.000000000000000000, -0.6595282642760668113, -0.7516797646744247663 ) ) ;
#31647 = CARTESIAN_POINT ( 'NONE',  ( 0.1589950187058424280, -2.107936428766274073, -0.7005084057759861649 ) ) ;
#31648 = DIRECTION ( 'NONE',  ( 1.000000000000000000, 0.000000000000000000, 0.000000000000000000 ) ) ;
#31649 = COORDINATED_UNIVERSAL_TIME_OFFSET ( 0, 0, .AHEAD. ) ;
#31650 = VECTOR ( 'NONE', #38250, 39.37007874015748143 ) ;
#31651 = CARTESIAN_POINT ( 'NONE',  ( 0.2448569360945407336, -0.9465973144586597998, 0.4687868266098103587 ) ) ;
#31652 = DIRECTION ( 'NONE',  ( -0.3468893892380657817, -0.7770416411310581140, 0.5252371270030266048 ) ) ;
#31653 = CARTESIAN_POINT ( 'NONE',  ( 0.4509566158158128113, -1.245465350927563275, 0.6057417262809816627 ) ) ;
#31654 = LINE ( 'NONE', #6746, #3491 ) ;
#31655 = CIRCLE ( 'NONE', #13896, 0.1333070866141734534 ) ;
#31656 = CARTESIAN_POINT ( 'NONE',  ( 0.06257380981966247091, -1.147456929947968884, 0.7547943717889301629 ) ) ;
#31657 = EDGE_CURVE ( 'NONE', #32089, #24957, #17447, .T. ) ;
#31658 = CIRCLE ( 'NONE', #21151, 0.5302738246768105013 ) ;
#31659 = CARTESIAN_POINT ( 'NONE',  ( 0.6894051875735035528, -1.431063707384874206, 0.5165551067006461938 ) ) ;
#31660 = APPLIED_PERSON_AND_ORGANIZATION_ASSIGNMENT ( #9463, #12354, ( #12929 ) ) ;
#31661 = CARTESIAN_POINT ( 'NONE',  ( 0.3663975874019590462, -1.157438136726376410, 0.4269148889825734039 ) ) ;
#31662 = EDGE_CURVE ( 'NONE', #1392, #7421, #1066, .T. ) ;
#31663 = VERTEX_POINT ( 'NONE', #1110 ) ;
#31664 = EDGE_LOOP ( 'NONE', ( #8444, #26920, #21321, #11819 ) ) ;
#31665 = CARTESIAN_POINT ( 'NONE',  ( 0.05082303569918651676, -0.3162776479886611480, -0.3525632866555280520 ) ) ;
#31666 = EDGE_LOOP ( 'NONE', ( #37469, #1686, #26143 ) ) ;
#31667 = CARTESIAN_POINT ( 'NONE',  ( 0.7053080889764471451, -1.513942001867420339, 0.5667347313869608438 ) ) ;
#31668 = FACE_OUTER_BOUND ( 'NONE', #8291, .T. ) ;
#31669 = CARTESIAN_POINT ( 'NONE',  ( 0.4043733228583301087, -1.150869673211134758, 0.8142501428070664238 ) ) ;
#31671 = ORIENTED_EDGE ( 'NONE', *, *, #37167, .T. ) ;
#31670 = CARTESIAN_POINT ( 'NONE',  ( 0.6047538891612445067, -1.605163873594933843, 0.4396382108053981108 ) ) ;
#31672 = CIRCLE ( 'NONE', #6688, 0.5302738246768088359 ) ;
#31673 = ORIENTED_EDGE ( 'NONE', *, *, #36301, .T. ) ;
#31674 = CARTESIAN_POINT ( 'NONE',  ( 0.1946548089260772552, -0.8036002232862070604, 0.2951871216237044182 ) ) ;
#31675 = VERTEX_POINT ( 'NONE', #26183 ) ;
#31676 = CARTESIAN_POINT ( 'NONE',  ( 0.01780422884439210318, -0.6047825753528456305, 0.3790601057835611964 ) ) ;
#31678 = CARTESIAN_POINT ( 'NONE',  ( 0.09455834122667663988, -1.311775142721860465, 0.5782422391874576517 ) ) ;
#31677 = CARTESIAN_POINT ( 'NONE',  ( 0.6411073885017467555, -1.563549741984003871, 0.4256454981679176908 ) ) ;
#31679 = CARTESIAN_POINT ( 'NONE',  ( 0.01175241438441537722, -0.6703469306311590215, -0.1131776774227842425 ) ) ;
#31680 = CARTESIAN_POINT ( 'NONE',  ( -0.1167294259372889248, -0.5331983348239512921, 0.3032895567580763396 ) ) ;
#31682 = ORIENTED_EDGE ( 'NONE', *, *, #18541, .T. ) ;
#31681 = VERTEX_POINT ( 'NONE', #22289 ) ;
#31683 = DIRECTION ( 'NONE',  ( 1.000000000000000000, 0.000000000000000000, 0.000000000000000000 ) ) ;
#31684 = CARTESIAN_POINT ( 'NONE',  ( 0.1204209576885674760, -0.9337813714611812310, 0.2981324907430850657 ) ) ;
#31685 = CARTESIAN_POINT ( 'NONE',  ( -0.04155248107635951815, -0.01723053523176999030, -0.4699878081388675355 ) ) ;
#31686 = CARTESIAN_POINT ( 'NONE',  ( 0.5852598773693732381, -1.437030116779531852, 0.6911710792806706749 ) ) ;
#31687 = VECTOR ( 'NONE', #22099, 39.37007874015748143 ) ;
#31688 = CIRCLE ( 'NONE', #23800, 0.9237847906030128842 ) ;
#31689 = CARTESIAN_POINT ( 'NONE',  ( 0.1427198293237539606, -0.8385480555221326293, 0.3785612601687390333 ) ) ;
#31690 = CARTESIAN_POINT ( 'NONE',  ( 0.1499999999999994948, 0.4638115001431033502, 0.2459753896937746653 ) ) ;
#31691 = CIRCLE ( 'NONE', #8004, 0.03000000000000002318 ) ;
#31692 = ADVANCED_FACE ( 'NONE', ( #34804 ), #28006, .F. ) ;
#31693 = EDGE_CURVE ( 'NONE', #8526, #34885, #4094, .T. ) ;
#31694 = CARTESIAN_POINT ( 'NONE',  ( 0.2706084658143584898, -1.502104413432969521, 1.006559446342335296 ) ) ;
#31695 = CARTESIAN_POINT ( 'NONE',  ( -0.1107910466892899765, -0.04310840302197994911, 0.3599999999999985989 ) ) ;
#31696 = CARTESIAN_POINT ( 'NONE',  ( 0.08222542156927918622, -1.327483614382551913, 0.4683366274853996702 ) ) ;
#31697 = CARTESIAN_POINT ( 'NONE',  ( 0.5876212857572584713, -1.642967741421476058, 0.5182417262812423209 ) ) ;
#31698 = CARTESIAN_POINT ( 'NONE',  ( 0.3820855590050560857, -1.701428075840956344, -0.4116647734693053007 ) ) ;
#31699 = CARTESIAN_POINT ( 'NONE',  ( 0.000000000000000000, 0.000000000000000000, 0.000000000000000000 ) ) ;
#31700 = CARTESIAN_POINT ( 'NONE',  ( -0.1399999999999997358, -1.330566893520353813E-17, -0.05000000000000000971 ) ) ;
#31701 = CARTESIAN_POINT ( 'NONE',  ( -3.414809992080329023E-17, -0.4300901116921415634, 0.2008512132480425316 ) ) ;
#31702 = CARTESIAN_POINT ( 'NONE',  ( 0.1070510364273958154, -1.394009378634261109, 0.6504313826203965698 ) ) ;
#31703 = PERSON_AND_ORGANIZATION ( #28500, #32463 ) ;
#31704 = AXIS2_PLACEMENT_3D ( 'NONE', #26388, #10962, #3200 ) ;
#31705 = CARTESIAN_POINT ( 'NONE',  ( -0.04047170147978008253, 0.4536011460193690725, 0.2133323880731032574 ) ) ;
#31706 = LINE ( 'NONE', #16290, #22838 ) ;
#31707 = AXIS2_PLACEMENT_3D ( 'NONE', #29568, #7757, #7330 ) ;
#31708 = SHAPE_REPRESENTATION ( 'pulley bushing', ( #27819 ), #30435 ) ;
#31709 = AXIS2_PLACEMENT_3D ( 'NONE', #4711, #26759, #32294 ) ;
#31710 = ORIENTED_EDGE ( 'NONE', *, *, #31101, .T. ) ;
#31711 = CARTESIAN_POINT ( 'NONE',  ( 0.1971908949274000789, -0.5803567546090362406, 0.3041702164619223270 ) ) ;
#31712 = VERTEX_POINT ( 'NONE', #25945 ) ;
#31713 = DIRECTION ( 'NONE',  ( 1.000000000000000000, 2.280301054154496446E-31, 1.355854680848613603E-31 ) ) ;
#31714 = CARTESIAN_POINT ( 'NONE',  ( 0.2391977394211191044, -1.507150632361212272, 0.9053633066493101955 ) ) ;
#31715 = CARTESIAN_POINT ( 'NONE',  ( 0.5949735957244766116, -1.487199741921636509, 0.5738185825883982405 ) ) ;
#31717 = ORIENTED_EDGE ( 'NONE', *, *, #8977, .F. ) ;
#31716 = DIRECTION ( 'NONE',  ( 1.000000000000000000, 0.000000000000000000, 0.000000000000000000 ) ) ;
#31718 = B_SPLINE_CURVE_WITH_KNOTS ( 'NONE', 3,
 ( #35135, #19509, #7125, #38013, #15796, #214 ),
 .UNSPECIFIED., .F., .F.,
 ( 4, 2, 4 ),
 ( 0.000000000000000000, 0.0006045613306913027790, 0.001209122661382605558 ),
 .UNSPECIFIED. ) ;
#31720 = ORIENTED_EDGE ( 'NONE', *, *, #18768, .T. ) ;
#31719 = ORIENTED_EDGE ( 'NONE', *, *, #24012, .T. ) ;
#31721 = LINE ( 'NONE', #37900, #9357 ) ;
#31722 = ORIENTED_EDGE ( 'NONE', *, *, #3712, .F. ) ;
#31723 = CIRCLE ( 'NONE', #24512, 0.02999999999999999195 ) ;
#31724 = CARTESIAN_POINT ( 'NONE',  ( 0.6418149653042463099, -1.608749606796000098, -0.5875140676452391686 ) ) ;
#31725 = DATE_TIME_ROLE ( 'classification_date' ) ;
#31726 = CARTESIAN_POINT ( 'NONE',  ( 0.01548846960721225047, -0.5203207976464844231, 0.08861466064783186936 ) ) ;
#31727 = ORIENTED_EDGE ( 'NONE', *, *, #31770, .F. ) ;
#31728 = CARTESIAN_POINT ( 'NONE',  ( 0.08697380094426622466, -0.7473793666617782883, 0.2016807350946292765 ) ) ;
#31729 = CARTESIAN_POINT ( 'NONE',  ( 0.1131952306228060368, -0.6121952599734634681, 0.3538291842944602528 ) ) ;
#31730 = CARTESIAN_POINT ( 'NONE',  ( 0.6413879784614744395, -1.405912376546664122, -0.6250000000000000000 ) ) ;
#31731 = CARTESIAN_POINT ( 'NONE',  ( -0.1588702854552091759, 0.4932535771925591894, 0.1179163363090176136 ) ) ;
#31732 = ORIENTED_EDGE ( 'NONE', *, *, #28075, .T. ) ;
#31733 = AXIS2_PLACEMENT_3D ( 'NONE', #8819, #31447, #40285 ) ;
#31734 = CARTESIAN_POINT ( 'NONE',  ( 0.4718170957853269898, -1.683435688723164292, 0.5702107750036669032 ) ) ;
#31735 = CARTESIAN_POINT ( 'NONE',  ( 0.6931178826097424972, -1.423648263565181704, 0.6754457899003547539 ) ) ;
#31736 = B_SPLINE_CURVE_WITH_KNOTS ( 'NONE', 3,
 ( #26916, #35764, #36360, #39446, #14772, #11486 ),
 .UNSPECIFIED., .F., .F.,
 ( 4, 2, 4 ),
 ( 0.000000000000000000, 0.5000000000000000000, 1.000000000000000000 ),
 .UNSPECIFIED. ) ;
#31737 = ORIENTED_EDGE ( 'NONE', *, *, #12763, .T. ) ;
#31738 = DIRECTION ( 'NONE',  ( -1.725633230170962886E-31, -0.4685245517978552932, 0.8834504764629530493 ) ) ;
#31739 = AXIS2_PLACEMENT_3D ( 'NONE', #25078, #11912, #2662 ) ;
#31740 = CARTESIAN_POINT ( 'NONE',  ( 0.5669781996639940980, -1.422531521005945043, 0.7532994004924005171 ) ) ;
#31741 = AXIS2_PLACEMENT_3D ( 'NONE', #38876, #36004, #17285 ) ;
#31742 = CARTESIAN_POINT ( 'NONE',  ( 0.005968620458395522063, -0.8455642846060320572, 0.1487736266978308408 ) ) ;
#31743 = B_SPLINE_CURVE_WITH_KNOTS ( 'NONE', 3,
 ( #8339, #4828, #33624, #29959, #30349, #39814, #36307, #8129, #5043, #33236, #1978, #14500, #2179, #11432, #23999, #5236, #14718, #11639, #12433, #12040, #5841, #5654 ),
 .UNSPECIFIED., .F., .F.,
 ( 4, 2, 2, 2, 2, 2, 2, 2, 2, 2, 4 ),
 ( 0.000000000000000000, 0.0007691844400138901378, 0.001538368880027780276, 0.003076737760055560118, 0.006153475520111119368, 0.007691844400138887934, 0.008461028840152783059, 0.009230213280166679052, 0.01076858216019446757, 0.01153776660020836183, 0.01230695104022225608 ),
 .UNSPECIFIED. ) ;
#31744 = CARTESIAN_POINT ( 'NONE',  ( 0.3207919832889619127, -1.182535135427784878, 0.4177417262808780229 ) ) ;
#31745 = CARTESIAN_POINT ( 'NONE',  ( 0.4494697147526631742, -1.096181161593837050, -0.6251428030132534230 ) ) ;
#31746 = CARTESIAN_POINT ( 'NONE',  ( 0.05825416142610396336, -1.237506905460590723, 0.6972702062804553291 ) ) ;
#31747 = AXIS2_PLACEMENT_3D ( 'NONE', #18140, #11962, #30695 ) ;
#31748 = CARTESIAN_POINT ( 'NONE',  ( 0.5017447040277105419, -1.102516469585429260, 0.6180670868896422920 ) ) ;
#31749 = PERSON_AND_ORGANIZATION ( #28500, #32463 ) ;
#31750 = CARTESIAN_POINT ( 'NONE',  ( 0.000000000000000000, 0.2954784694557334168, 0.05188905557145093855 ) ) ;
#31751 = CARTESIAN_POINT ( 'NONE',  ( -0.04155248107635974020, 0.4416604393009535556, -0.1616214326753681041 ) ) ;
#31752 = CARTESIAN_POINT ( 'NONE',  ( -0.04211812644076826789, 0.008544267401289764793, 0.4689465636496595868 ) ) ;
#31753 = ORIENTED_EDGE ( 'NONE', *, *, #2155, .F. ) ;
#31754 = CARTESIAN_POINT ( 'NONE',  ( -0.1443375672974067936, 0.05141091571461216952, 0.000000000000000000 ) ) ;
#31755 = DIRECTION ( 'NONE',  ( 1.000000000000000000, 0.000000000000000000, 0.000000000000000000 ) ) ;
#31756 = CIRCLE ( 'NONE', #14020, 0.01500000000000000638 ) ;
#31757 = FACE_OUTER_BOUND ( 'NONE', #28597, .T. ) ;
#31758 = ORIENTED_EDGE ( 'NONE', *, *, #12355, .T. ) ;
#31759 = CARTESIAN_POINT ( 'NONE',  ( 0.3366372923301772513, -1.754154571440896593, 0.4608008921661775337 ) ) ;
#31760 = EDGE_CURVE ( 'NONE', #27450, #20248, #6382, .T. ) ;
#31761 = CARTESIAN_POINT ( 'NONE',  ( 0.05446806353428223363, -1.187490080796402170, 0.7666483277446362044 ) ) ;
#31763 = EDGE_LOOP ( 'NONE', ( #2984, #8942, #729, #8638, #23995, #32616, #26204, #11778 ) ) ;
#31762 = ORIENTED_EDGE ( 'NONE', *, *, #37528, .T. ) ;
#31764 = EDGE_CURVE ( 'NONE', #30658, #25698, #6992, .T. ) ;
#31765 = DIRECTION ( 'NONE',  ( 0.000000000000000000, -0.8660489055767767175, -0.4999592914920847897 ) ) ;
#31766 = VECTOR ( 'NONE', #1136, 39.37007874015748143 ) ;
#31767 = CONICAL_SURFACE ( 'NONE', #8769, 0.1600000000000006140, 1.047197551196599630 ) ;
#31768 = CARTESIAN_POINT ( 'NONE',  ( 0.3303674864723026849, -1.765107817504619980, 0.5532596536417452304 ) ) ;
#31769 = CARTESIAN_POINT ( 'NONE',  ( 0.4064036231482041073, -1.678616732723309024, -0.5150861416748760968 ) ) ;
#31770 = EDGE_CURVE ( 'NONE', #29903, #1932, #39105, .T. ) ;
#31772 = DIRECTION ( 'NONE',  ( -3.235562306570549665E-32, 0.6954292836767010932, 0.7185945389473191725 ) ) ;
#31771 = CARTESIAN_POINT ( 'NONE',  ( 0.5958380658908700722, -1.598773897477913319, 0.4314101756398622256 ) ) ;
#31773 = CARTESIAN_POINT ( 'NONE',  ( 0.05634206451479712580, -0.2780979935378002366, -0.3651623763481146034 ) ) ;
#31774 = ORIENTED_EDGE ( 'NONE', *, *, #6586, .F. ) ;
#31775 = CARTESIAN_POINT ( 'NONE',  ( 0.1718750000000005274, -0.4925660985513966028, 0.3136681013253508898 ) ) ;
#31776 = EDGE_CURVE ( 'NONE', #13497, #32636, #11040, .T. ) ;
#31777 = ORIENTED_EDGE ( 'NONE', *, *, #32624, .F. ) ;
#31778 = ORIENTED_EDGE ( 'NONE', *, *, #10692, .F. ) ;
#31779 = CARTESIAN_POINT ( 'NONE',  ( 0.09029415657535862227, -0.5650508117823077603, 0.1858836665007985722 ) ) ;
#31780 = ORIENTED_EDGE ( 'NONE', *, *, #33516, .T. ) ;
#31781 = VECTOR ( 'NONE', #17282, 39.37007874015748143 ) ;
#31782 = ORIENTED_EDGE ( 'NONE', *, *, #26053, .T. ) ;
#31783 = CARTESIAN_POINT ( 'NONE',  ( 0.01223808240847633344, -0.4396073437767880621, 0.2324838087239345930 ) ) ;
#31784 = CARTESIAN_POINT ( 'NONE',  ( 0.4577816522039453995, -1.524573175657774282, 0.7453819971993982385 ) ) ;
#31785 = CIRCLE ( 'NONE', #14039, 0.01500000000000001506 ) ;
#31787 = CARTESIAN_POINT ( 'NONE',  ( -0.1093417548587973798, -0.4991680509864717674, 0.3564048400776359538 ) ) ;
#31786 = CARTESIAN_POINT ( 'NONE',  ( 0.01431878725343691504, -0.6569777124000869550, 0.5019137659709727028 ) ) ;
#31788 = CARTESIAN_POINT ( 'NONE',  ( 0.4137599315576335757, -1.590143257116447995, -0.4137273532990812797 ) ) ;
#31789 = CARTESIAN_POINT ( 'NONE',  ( 0.1745125816602956792, -0.9195344838042885938, 0.2322212926758656093 ) ) ;
#31790 = CARTESIAN_POINT ( 'NONE',  ( 0.1999999999999780564, -2.097675824466503247, -0.7286991843995637153 ) ) ;
#31791 = CARTESIAN_POINT ( 'NONE',  ( 0.1153471661799889414, -0.4465907051537492123, 0.1406012133455230018 ) ) ;
#31792 = CARTESIAN_POINT ( 'NONE',  ( 0.3341561371861889174, -1.068396439941279530, 0.7924052243473069801 ) ) ;
#31793 = CARTESIAN_POINT ( 'NONE',  ( -0.02238765564325451152, 0.3549921663302683106, -0.3695537732572939937 ) ) ;
#31794 = ADVANCED_FACE ( 'NONE', ( #10304 ), #18950, .T. ) ;
#31795 = APPROVAL ( #3862, 'UNSPECIFIED' ) ;
#31796 = CARTESIAN_POINT ( 'NONE',  ( -0.04760454375022137724, -0.4435184909896772165, -0.1893283029546962704 ) ) ;
#31797 = VECTOR ( 'NONE', #35711, 39.37007874015748143 ) ;
#31798 = CARTESIAN_POINT ( 'NONE',  ( 0.1479676914811787758, -0.7747515144801853104, 0.6021013852491187146 ) ) ;
#31799 = DIRECTION ( 'NONE',  ( 0.000000000000000000, 0.8090169943749455639, -0.5877852522924756906 ) ) ;
#31800 = CARTESIAN_POINT ( 'NONE',  ( 0.6622529324379804461, -1.370658042826599310, 0.7087354899337895420 ) ) ;
#31801 = VECTOR ( 'NONE', #5426, 39.37007874015748143 ) ;
#31802 = AXIS2_PLACEMENT_3D ( 'NONE', #21893, #28449, #16127 ) ;
#31803 = DIRECTION ( 'NONE',  ( 0.000000000000000000, 0.000000000000000000, 1.000000000000000000 ) ) ;
#31804 = CARTESIAN_POINT ( 'NONE',  ( 0.03820739074425011372, -1.193531024389712369, 0.6672744448627624392 ) ) ;
#31805 = DIRECTION ( 'NONE',  ( 3.414809992080326361E-15, 1.000000000000000000, -2.845674993400271967E-15 ) ) ;
#31806 = CARTESIAN_POINT ( 'NONE',  ( 0.4795819664771984736, -1.106247336020415917, -0.4111404562665418871 ) ) ;
#31807 = CARTESIAN_POINT ( 'NONE',  ( 0.2058175959260750976, -0.8974321954632414888, 0.6308810174354192446 ) ) ;
#31808 = CARTESIAN_POINT ( 'NONE',  ( 0.02231181081520633436, 0.07006449514257805100, 0.5077922075898764209 ) ) ;
#31809 = CARTESIAN_POINT ( 'NONE',  ( 0.6845239711983126529, -1.512855307908938185, 0.4537933262130811052 ) ) ;
#31810 = VECTOR ( 'NONE', #21897, 39.37007874015748143 ) ;
#31811 = EDGE_LOOP ( 'NONE', ( #24212, #29642, #4877, #30198, #34748 ) ) ;
#31812 = CARTESIAN_POINT ( 'NONE',  ( -0.02000000000000000042, -2.268861055605315258, -0.3290426542847164626 ) ) ;
#31813 = CARTESIAN_POINT ( 'NONE',  ( 0.005980720888701209978, -0.8455916207747946611, 0.1457185332388707122 ) ) ;
#31814 = CARTESIAN_POINT ( 'NONE',  ( -0.3000000000000000999, -2.461298705151934829, -0.7594706439553173816 ) ) ;
#31815 = CARTESIAN_POINT ( 'NONE',  ( 0.3556569928175498663, -1.173715065104882216, 0.4182417262808778013 ) ) ;
#31816 = VERTEX_POINT ( 'NONE', #7175 ) ;
#31817 = ADVANCED_FACE ( 'NONE', ( #19743 ), #12767, .F. ) ;
#31818 = CARTESIAN_POINT ( 'NONE',  ( -0.1574156176409216568, 0.4885425907994525030, 0.3417174393643538921 ) ) ;
#31819 = CARTESIAN_POINT ( 'NONE',  ( 0.1801801353197204358, -0.5022319782753607020, 0.1625915292881466023 ) ) ;
#31820 = LINE ( 'NONE', #25870, #14699 ) ;
#31821 = CIRCLE ( 'NONE', #22009, 0.05330708661417342398 ) ;
#31822 = EDGE_CURVE ( 'NONE', #26475, #8991, #31250, .T. ) ;
#31823 = CARTESIAN_POINT ( 'NONE',  ( 0.4019058561636069116, -1.150920537793857390, 0.7414317717734241198 ) ) ;
#31825 = CARTESIAN_POINT ( 'NONE',  ( -1.019575837292305609, -0.04310840302198155199, 0.3599999999999999867 ) ) ;
#31824 = DIRECTION ( 'NONE',  ( -0.4379975771764391679, 0.8989761522907986357, 0.000000000000000000 ) ) ;
#31826 = CARTESIAN_POINT ( 'NONE',  ( 0.3767165169986340101, -1.018944133209149783, 0.6225985890371608100 ) ) ;
#31827 = EDGE_LOOP ( 'NONE', ( #38501, #14617, #9624, #7633 ) ) ;
#31829 = AXIS2_PLACEMENT_3D ( 'NONE', #18420, #27694, #24624 ) ;
#31828 = PERSON_AND_ORGANIZATION_ROLE ( 'classification_officer' ) ;
#31830 = ADVANCED_FACE ( 'NONE', ( #39075 ), #26537, .F. ) ;
#31831 = CARTESIAN_POINT ( 'NONE',  ( 0.09044078639664698827, -1.315030787261194156, 0.7167242329630961750 ) ) ;
#31832 = ORIENTED_EDGE ( 'NONE', *, *, #30894, .T. ) ;
#31833 = VECTOR ( 'NONE', #20372, 39.37007874015748854 ) ;
#31834 = ORIENTED_EDGE ( 'NONE', *, *, #22274, .T. ) ;
#31835 = CARTESIAN_POINT ( 'NONE',  ( 0.3475135998290112549, -1.498927023588051188, 0.8450769405235730725 ) ) ;
#31837 = CARTESIAN_POINT ( 'NONE',  ( 0.1108945586471002803, -0.9285926214858456484, 0.1502493406847869584 ) ) ;
#31836 = CARTESIAN_POINT ( 'NONE',  ( 0.5602799925893692246, -1.505597493397644149, 0.5182417262812344383 ) ) ;
#31838 = DIRECTION ( 'NONE',  ( -6.162975822039151309E-33, 0.000000000000000000, -1.000000000000000000 ) ) ;
#31839 = LOCAL_TIME ( 0, 53, 7.000000000000000000, #16467 ) ;
#31840 = ORIENTED_EDGE ( 'NONE', *, *, #1154, .T. ) ;
#31841 = CARTESIAN_POINT ( 'NONE',  ( 0.4146010801322109196, -1.125553305772108104, 0.5889438968355630299 ) ) ;
#31842 = CARTESIAN_POINT ( 'NONE',  ( 0.5679433476211590559, -1.501425632804762822, 0.6203578022940468006 ) ) ;
#31843 = VERTEX_POINT ( 'NONE', #30027 ) ;
#31844 = CIRCLE ( 'NONE', #20012, 0.03000000000000006481 ) ;
#31845 = CARTESIAN_POINT ( 'NONE',  ( 0.1874563621180923845, -0.6894654218958394809, 0.06001567365385099967 ) ) ;
#31846 = CARTESIAN_POINT ( 'NONE',  ( 0.09522563388679633478, -1.586419958512597539, -0.3717731054125978374 ) ) ;
#31847 = DIRECTION ( 'NONE',  ( 1.707404996040163180E-15, -0.1725921171157359935, -0.9849933812516245002 ) ) ;
#31848 = EDGE_CURVE ( 'NONE', #28606, #20339, #9577, .T. ) ;
#31849 = CARTESIAN_POINT ( 'NONE',  ( -0.2000000000000003164, 0.5182417262804734914, 0.08500000000000001998 ) ) ;
#31850 = CARTESIAN_POINT ( 'NONE',  ( 0.1850841550199354701, -0.8515884040318244530, 0.1812164098636643572 ) ) ;
#31851 = CARTESIAN_POINT ( 'NONE',  ( 0.2534230856981304347, -1.365321207853003926, -0.2869361388274794256 ) ) ;
#31852 = CARTESIAN_POINT ( 'NONE',  ( 0.05999999999999990757, 7.654042494670956004E-18, -0.06250000000000000000 ) ) ;
#31853 = CARTESIAN_POINT ( 'NONE',  ( 0.4234909963964843538, -1.082397635545747638, -0.5155029497116575543 ) ) ;
#31854 = CARTESIAN_POINT ( 'NONE',  ( 0.3943729676430805520, -1.992383741152799370, -0.7037009085642309536 ) ) ;
#31855 = DIRECTION ( 'NONE',  ( 2.532366176626896502E-12, -1.000000000000000000, -5.691349986800531115E-16 ) ) ;
#31856 = CARTESIAN_POINT ( 'NONE',  ( 0.08788382977687533848, -1.333624949218704225, 0.7170191112640089681 ) ) ;
#31857 = APPROVAL_DATE_TIME ( #9430, #8649 ) ;
#31858 = DIRECTION ( 'NONE',  ( -1.000000000000000000, -0.000000000000000000, -0.000000000000000000 ) ) ;
#31859 = CONICAL_SURFACE ( 'NONE', #35151, 0.4488493849861018292, 1.047197551196600962 ) ;
#31860 = DIRECTION ( 'NONE',  ( 0.4999551463232371762, -0.8660512985181134660, 0.000000000000000000 ) ) ;
#31861 = CARTESIAN_POINT ( 'NONE',  ( 0.4409575364527853480, -1.228144365775162727, 0.5856983068965044836 ) ) ;
#31862 = CARTESIAN_POINT ( 'NONE',  ( -0.02000000000000000042, -1.802948570736253586, -0.8420585814095631338 ) ) ;
#31863 = CIRCLE ( 'NONE', #24009, 0.3698489655878011706 ) ;
#31864 = AXIS2_PLACEMENT_3D ( 'NONE', #17793, #24001, #5656 ) ;
#31865 = APPLIED_APPROVAL_ASSIGNMENT ( #26276, ( #17711 ) ) ;
#31866 = CARTESIAN_POINT ( 'NONE',  ( 0.2844183530474730937, -1.648412185216814541, 0.8663902821515296893 ) ) ;
#31867 = CARTESIAN_POINT ( 'NONE',  ( 0.0003498636168733311783, -0.4606750075364664521, 0.04272264150788647463 ) ) ;
#31868 = CARTESIAN_POINT ( 'NONE',  ( 0.6588040530991939869, -1.448684765798575080, 0.4330110937685633377 ) ) ;
#31869 = CARTESIAN_POINT ( 'NONE',  ( 0.2567678775328935958, -1.218994432343741163, 0.4282360825589090481 ) ) ;
#31870 = ORIENTED_EDGE ( 'NONE', *, *, #35147, .F. ) ;
#31871 = EDGE_LOOP ( 'NONE', ( #4334, #27534, #19504, #3535 ) ) ;
#31872 = EDGE_CURVE ( 'NONE', #3229, #28482, #13501, .T. ) ;
#31873 = LINE ( 'NONE', #16041, #5258 ) ;
#31874 = EDGE_LOOP ( 'NONE', ( #23499, #12893, #23357, #12389 ) ) ;
#31875 = CARTESIAN_POINT ( 'NONE',  ( -0.1304423469995338869, -0.5262799683630393632, 0.09999999999999933942 ) ) ;
#31876 = CARTESIAN_POINT ( 'NONE',  ( 0.5746577578530626118, -1.612782564726902290, -0.5066312177471922196 ) ) ;
#31877 = EDGE_CURVE ( 'NONE', #25200, #3242, #23379, .T. ) ;
#31878 = CARTESIAN_POINT ( 'NONE',  ( 0.3465686840206718689, -1.059727123120684400, 0.8002934259178389187 ) ) ;
#31880 = ORIENTED_EDGE ( 'NONE', *, *, #9368, .F. ) ;
#31879 = DIRECTION ( 'NONE',  ( 0.4999551463232372317, -0.8660512985181135770, 0.000000000000000000 ) ) ;
#31881 = VERTEX_POINT ( 'NONE', #35987 ) ;
#31882 = CARTESIAN_POINT ( 'NONE',  ( 0.2018967578894778903, -0.6341889671314926424, 0.3404161510980175942 ) ) ;
#31883 = ORIENTED_EDGE ( 'NONE', *, *, #24733, .T. ) ;
#31884 = CARTESIAN_POINT ( 'NONE',  ( 0.01081499117344541377, -0.5305016636949330122, 0.1645499100564967454 ) ) ;
#31886 = CARTESIAN_POINT ( 'NONE',  ( 0.1934284681205496736, -1.261395051998276839, -0.3194747338454530516 ) ) ;
#31885 = FACE_OUTER_BOUND ( 'NONE', #39541, .T. ) ;
#31887 = LINE ( 'NONE', #16056, #38490 ) ;
#31888 = CARTESIAN_POINT ( 'NONE',  ( 0.01210987442631182576, -0.4416276171603741307, 0.06224955564382433915 ) ) ;
#31889 = AXIS2_PLACEMENT_3D ( 'NONE', #22867, #35385, #270 ) ;
#31890 = CARTESIAN_POINT ( 'NONE',  ( 0.06691088171154270514, -1.526692643628365209, -0.3435217948658035314 ) ) ;
#31892 = ORIENTED_EDGE ( 'NONE', *, *, #18590, .T. ) ;
#31891 = ORIENTED_EDGE ( 'NONE', *, *, #39607, .F. ) ;
#31893 = AXIS2_PLACEMENT_3D ( 'NONE', #29879, #7437, #39135 ) ;
#31894 = CARTESIAN_POINT ( 'NONE',  ( 0.03113248654051816583, 0.5878163732725504298, -0.1704268771689479434 ) ) ;
#31895 = CARTESIAN_POINT ( 'NONE',  ( 0.1110471613688909648, -0.9287055108011992299, 0.1649583684456411847 ) ) ;
#31896 = CARTESIAN_POINT ( 'NONE',  ( -0.1443375672974067936, 0.000000000000000000, 0.000000000000000000 ) ) ;
#31897 = CARTESIAN_POINT ( 'NONE',  ( 0.5671292872122295492, -1.407209245721033675, 0.7602874898437926854 ) ) ;
#31898 = EDGE_CURVE ( 'NONE', #12543, #5617, #17473, .T. ) ;
#31899 = CARTESIAN_POINT ( 'NONE',  ( 0.3288109612775019230, -1.078958935667085894, 0.7405084338778586961 ) ) ;
#31900 = LOCAL_TIME ( 0, 53, 7.000000000000000000, #33170 ) ;
#31901 = CARTESIAN_POINT ( 'NONE',  ( 0.1193992653793402442, -1.100149244796670978, 0.8813937183720087498 ) ) ;
#31902 = EDGE_CURVE ( 'NONE', #3578, #40101, #37136, .T. ) ;
#31903 = CARTESIAN_POINT ( 'NONE',  ( 0.4403505402492592369, -1.147073999512834508, 0.4182417262808918457 ) ) ;
#31904 = ADVANCED_FACE ( 'NONE', ( #23860 ), #29925, .T. ) ;
#31905 = AXIS2_PLACEMENT_3D ( 'NONE', #31092, #6391, #40549 ) ;
#31906 = CARTESIAN_POINT ( 'NONE',  ( 0.4717768270077258852, -1.210421857018928460, 0.5378582626174832626 ) ) ;
#31907 = DIRECTION ( 'NONE',  ( 0.000000000000000000, 0.000000000000000000, -1.000000000000000000 ) ) ;
#31908 = DIRECTION ( 'NONE',  ( 1.387778780781449423E-15, -6.590151126658375938E-16, 1.000000000000000000 ) ) ;
#31909 = CARTESIAN_POINT ( 'NONE',  ( 0.03478489236950594449, -0.3590487419276154335, 0.3712145292149066078 ) ) ;
#31910 = DIRECTION ( 'NONE',  ( 1.000000000000000000, 0.000000000000000000, 0.000000000000000000 ) ) ;
#31911 = CARTESIAN_POINT ( 'NONE',  ( 0.1889659664986145515, -1.964260910147563655, -0.6656705585301033734 ) ) ;
#31912 = CALENDAR_DATE ( 2026, 13, 10 ) ;
#31913 = CARTESIAN_POINT ( 'NONE',  ( 0.3996799965260696141, -1.685664405872516980, -0.5055465857900723892 ) ) ;
#31914 = CARTESIAN_POINT ( 'NONE',  ( -0.05201782277453367159, 0.4527080286589615921, 0.1280848763234634091 ) ) ;
#31915 = CLOSED_SHELL ( 'NONE', ( #15192, #40468, #21538, #1768, #30021, #706, #13018, #28141, #17026, #8970, #18247, #22292, #26655, #34063, #19535, #24259, #29151, #6246, #17971, #24279, #39407, #12279, #27618, #32289, #16228, #8400, #2528, #14310, #18735, #18538, #29020, #9286, #13435, #21479, #19025, #13992, #18533, #4414, #18816, #23534, #6699, #13644, #35150, #3776, #13446, #10933, #31367, #35912, #34316, #37056, #20968, #32312, #22745, #7521, #24355, #7669, #39685, #5715, #34698, #30790, #28777, #26588, #35649, #25291, #15011, #11617, #26613, #20054, #19975, #16102, #34659, #37644, #37985, #19473, #34879, #9183, #4863, #22121, #654, #24, #21013, #10136, #19482, #25121, #40037, #35647, #38554, #39632, #7933, #32162, #15851, #10760, #7758, #19052, #37102, #3327, #34041, #13238, #3681, #8627, #16800, #12020, #13534, #19746, #9160, #31817, #7714, #38474, #535, #22534, #7883, #26272, #32384, #38076, #37921, #35944, #27308, #36312, #37084, #12418, #33003, #23603, #5195, #26936, #8452, #33299 ) ) ;
#31916 = CIRCLE ( 'NONE', #34556, 0.06000000000000021289 ) ;
#31917 = CARTESIAN_POINT ( 'NONE',  ( 0.3737379149731986927, -1.762635032660671230, -0.5786828194896244115 ) ) ;
#31918 = ORIENTED_EDGE ( 'NONE', *, *, #5215, .F. ) ;
#31919 = CARTESIAN_POINT ( 'NONE',  ( 0.1909151965350180669, -0.5465291738026563095, 0.2914815663883933983 ) ) ;
#31920 = VERTEX_POINT ( 'NONE', #32484 ) ;
#31921 = DIRECTION ( 'NONE',  ( -1.000000000000000000, -0.000000000000000000, -0.000000000000000000 ) ) ;
#31922 = APPLIED_APPROVAL_ASSIGNMENT ( #30992, ( #38779 ) ) ;
#31923 = CARTESIAN_POINT ( 'NONE',  ( 0.2713285965202352767, -1.671844724629077961, 0.7237048008743941496 ) ) ;
#31924 = ADVANCED_FACE ( 'NONE', ( #36383 ), #17063, .T. ) ;
#31925 = CARTESIAN_POINT ( 'NONE',  ( 0.5130770162454134642, -1.369941357579992580, 0.7991392945303081863 ) ) ;
#31927 = ORIENTED_EDGE ( 'NONE', *, *, #24249, .F. ) ;
#31926 = CARTESIAN_POINT ( 'NONE',  ( 0.5188695029506764644, -1.672825691405887216, -0.4370831669522161067 ) ) ;
#31928 = EDGE_CURVE ( 'NONE', #23895, #34187, #6903, .T. ) ;
#31929 = AXIS2_PLACEMENT_3D ( 'NONE', #23004, #35741, #816 ) ;
#31931 = ORIENTED_EDGE ( 'NONE', *, *, #22319, .F. ) ;
#31930 = ORIENTED_EDGE ( 'NONE', *, *, #16964, .F. ) ;
#31932 = DIRECTION ( 'NONE',  ( 0.7956551220374307176, 0.4593167559955306789, 0.3949190352937466675 ) ) ;
#31933 = ORIENTED_EDGE ( 'NONE', *, *, #39124, .T. ) ;
#31934 = PLANE ( 'NONE',  #6553 ) ;
#31935 = FACE_OUTER_BOUND ( 'NONE', #11999, .T. ) ;
#31936 = CALENDAR_DATE ( 2026, 13, 10 ) ;
#31937 = DIRECTION ( 'NONE',  ( 7.771561172376107616E-16, -7.170354002788761615E-17, 1.000000000000000000 ) ) ;
#31938 = EDGE_LOOP ( 'NONE', ( #38237, #32519, #8545, #31782 ) ) ;
#31939 = CARTESIAN_POINT ( 'NONE',  ( 0.09656389424368523600, -0.7804001749690797629, 0.3156549668601592029 ) ) ;
#31940 = CARTESIAN_POINT ( 'NONE',  ( 0.06924781316064872183, -0.5400285655940516572, 0.1484324165790556205 ) ) ;
#31941 = CARTESIAN_POINT ( 'NONE',  ( 0.4754402869458209668, -1.412207419392573993, 0.8084286269221809818 ) ) ;
#31942 = CARTESIAN_POINT ( 'NONE',  ( 0.6438069111488841090, -1.607599693877530544, -0.4632284053853421568 ) ) ;
#31943 = CARTESIAN_POINT ( 'NONE',  ( -0.1508021419688942433, 0.4665171419162573718, 0.09550516381870209626 ) ) ;
#31944 = CARTESIAN_POINT ( 'NONE',  ( -0.1670982076487625978, 0.5191099701766067609, 0.1307156235296936808 ) ) ;
#31945 = DIRECTION ( 'NONE',  ( 0.3468893892380796595, -0.7396492646830092887, -0.5767033179095778506 ) ) ;
#31946 = CARTESIAN_POINT ( 'NONE',  ( 0.6663302113144387029, -1.561568830604052716, 0.5775187608084981772 ) ) ;
#31947 = CIRCLE ( 'NONE', #28683, 0.009999999999999956840 ) ;
#31948 = CARTESIAN_POINT ( 'NONE',  ( -0.1107910466892899765, -0.04310840302197994911, 0.09999999999999809042 ) ) ;
#31949 = CARTESIAN_POINT ( 'NONE',  ( 0.5831096498430272668, -1.442877891438895555, 0.7273179858556853006 ) ) ;
#31950 = CARTESIAN_POINT ( 'NONE',  ( -0.002232160660486151842, -0.8557013418396056670, 0.1376595806906051045 ) ) ;
#31951 = SECURITY_CLASSIFICATION ( '', '', #15279 ) ;
#31952 = DIRECTION ( 'NONE',  ( 1.000000000000000000, 2.280301054154495132E-31, -1.664003471950577689E-31 ) ) ;
#31953 = CARTESIAN_POINT ( 'NONE',  ( 0.4670213778778394831, -1.236191465557153757, 0.6057417262809817737 ) ) ;
#31954 = AXIS2_PLACEMENT_3D ( 'NONE', #29064, #9541, #9740 ) ;
#31955 = CARTESIAN_POINT ( 'NONE',  ( 0.02666925540767700956, -1.119321828221852888, 0.6528166539191706530 ) ) ;
#31956 = CARTESIAN_POINT ( 'NONE',  ( 0.1971950993027475063, -0.8036775079564704161, 0.3187204964795984363 ) ) ;
#31957 = PERSON_AND_ORGANIZATION ( #28500, #32463 ) ;
#31958 =( BOUNDED_SURFACE ( )  B_SPLINE_SURFACE ( 3, 2, ( 
 ( #37481, #21881, #34409 ),
 ( #18986, #14885, #15894 ),
 ( #19784, #35423, #19189 ),
 ( #25376, #13413, #31518 ) ),
 .UNSPECIFIED., .F., .F., .T. ) 
 B_SPLINE_SURFACE_WITH_KNOTS ( ( 4, 4 ),
 ( 3, 3 ),
 ( -8.673617379884035472E-19, 0.002131800461895016693 ),
 ( 0.4549088439910530246, 0.5960639224100784395 ),
 .UNSPECIFIED. ) 
 GEOMETRIC_REPRESENTATION_ITEM ( )  RATIONAL_B_SPLINE_SURFACE ( (
 ( 0.8536398787998742410, 0.8498830870480222899, 0.8578866998027966373),
 ( 0.8543866741646273244, 0.8506490512590678676, 0.8586118259709549783),
 ( 0.8547489119030206028, 0.8510205869656279898, 0.8589635529307095840),
 ( 0.8547444188128500153, 0.8510159785461998139, 0.8589591902131400447) ) ) 
 REPRESENTATION_ITEM ( '' )  SURFACE ( )  );
#31959 = CARTESIAN_POINT ( 'NONE',  ( 0.4115766028365042128, -1.733048369835246794, 0.5182417262812423209 ) ) ;
#31960 = DIRECTION ( 'NONE',  ( 1.000000000000000000, 0.000000000000000000, 0.000000000000000000 ) ) ;
#31961 = CARTESIAN_POINT ( 'NONE',  ( 0.4233859075605026501, -1.153205106124581381, 0.4182417262808776903 ) ) ;
#31962 = ORIENTED_EDGE ( 'NONE', *, *, #19290, .F. ) ;
#31963 = CARTESIAN_POINT ( 'NONE',  ( -0.02953079040095700838, 0.000000000000000000, 0.000000000000000000 ) ) ;
#31964 = CARTESIAN_POINT ( 'NONE',  ( 0.04855986989123576431, 0.05683501216513837939, 0.1249999999999993616 ) ) ;
#31965 = CARTESIAN_POINT ( 'NONE',  ( 0.08771792644201747979, -0.6708790313995512955, 0.02355072261337067333 ) ) ;
#31966 = EDGE_LOOP ( 'NONE', ( #39198, #21557, #4993, #39232 ) ) ;
#31967 = AXIS2_PLACEMENT_3D ( 'NONE', #25228, #34073, #6296 ) ;
#31968 = CARTESIAN_POINT ( 'NONE',  ( 0.1435064959217801916, -1.283467536720964697, 0.5197417262808780025 ) ) ;
#31969 = CARTESIAN_POINT ( 'NONE',  ( 0.1288202176491853868, -1.269087133838645354, 0.7371036684735357003 ) ) ;
#31971 = ORIENTED_EDGE ( 'NONE', *, *, #13500, .F. ) ;
#31970 = VERTEX_POINT ( 'NONE', #16876 ) ;
#31972 = DIRECTION ( 'NONE',  ( 1.000000000000000000, -0.000000000000000000, -0.000000000000000000 ) ) ;
#31973 = EDGE_LOOP ( 'NONE', ( #32713, #20924, #945, #30410 ) ) ;
#31974 = DIRECTION ( 'NONE',  ( 0.8660512985181133550, 0.4999551463232372872, 0.000000000000000000 ) ) ;
#31975 = LOCAL_TIME ( 0, 53, 7.000000000000000000, #33528 ) ;
#31976 = B_SPLINE_CURVE_WITH_KNOTS ( 'NONE', 3,
 ( #20105, #16813, #29357, #13702, #1198, #26269, #10420 ),
 .UNSPECIFIED., .F., .F.,
 ( 4, 3, 4 ),
 ( 0.000000000000000000, 0.0001987961317490854899, 0.0002262042107145686282 ),
 .UNSPECIFIED. ) ;
#31977 = LINE ( 'NONE', #29084, #37716 ) ;
#31978 = CARTESIAN_POINT ( 'NONE',  ( 0.5947695011133637966, -1.599389987319376649, 0.4269865408061249146 ) ) ;
#31979 = CARTESIAN_POINT ( 'NONE',  ( 0.1909286924077255032, -1.257064795538239022, -0.2869361388274795921 ) ) ;
#31980 = ORIENTED_EDGE ( 'NONE', *, *, #12184, .T. ) ;
#31981 = CARTESIAN_POINT ( 'NONE',  ( 0.3802414748335787298, -1.273567264344565686, 1.090231875592916788 ) ) ;
#31982 = MANIFOLD_SOLID_BREP ( 'Boss-Extrude3', #25382 ) ;
#31983 = VECTOR ( 'NONE', #18901, 39.37007874015748143 ) ;
#31984 = CARTESIAN_POINT ( 'NONE',  ( 0.1943063309424913621, -0.8117621587600959421, 0.6459455874387924901 ) ) ;
#31985 = CARTESIAN_POINT ( 'NONE',  ( 0.08509875786982322443, -0.8822929212134896781, 0.8597185319039459817 ) ) ;
#31986 = CARTESIAN_POINT ( 'NONE',  ( 0.08687719282835834611, -0.5652987713911060697, 0.2467322302443580861 ) ) ;
#31988 = CARTESIAN_POINT ( 'NONE',  ( -0.1148620258665340038, -0.5252635219643339015, 0.3299751171063038946 ) ) ;
#31987 = CARTESIAN_POINT ( 'NONE',  ( 0.5063069112233773428, -1.619831626756517595, -0.4536019516388486439 ) ) ;
#31989 = CARTESIAN_POINT ( 'NONE',  ( -0.05464101615137785528, -2.196538720661423749, -0.6552417777791260667 ) ) ;
#31990 = CARTESIAN_POINT ( 'NONE',  ( 0.4470293266345468641, -1.057522354523741326, 0.6334801600245920650 ) ) ;
#31991 = ORIENTED_EDGE ( 'NONE', *, *, #13433, .F. ) ;
#31992 = CARTESIAN_POINT ( 'NONE',  ( 0.05999999999999990757, -0.2940959072101921867, -0.05922497245433272495 ) ) ;
#31993 = CARTESIAN_POINT ( 'NONE',  ( 0.1897112319679104542, -0.5340524121046181794, 0.1461038013937293045 ) ) ;
#31994 = CARTESIAN_POINT ( 'NONE',  ( -0.05489899477340578343, 0.2921074789649996672, -0.3589041746640609931 ) ) ;
#31995 = CARTESIAN_POINT ( 'NONE',  ( -0.04047076529491829000, -0.4536027527280144800, -0.2133348358548762813 ) ) ;
#31996 = CARTESIAN_POINT ( 'NONE',  ( -0.2399999999999999079, -2.294529520598973082, -0.6534431116140350104 ) ) ;
#31997 = AXIS2_PLACEMENT_3D ( 'NONE', #33778, #15665, #34175 ) ;
#31998 = CARTESIAN_POINT ( 'NONE',  ( 0.6508285628959425972, -1.351727978844563749, 0.7336055660202295270 ) ) ;
#31999 = CARTESIAN_POINT ( 'NONE',  ( -0.3000000000000000999, -3.941790907013290823, -0.009415996779116623042 ) ) ;
#32000 = CARTESIAN_POINT ( 'NONE',  ( 0.06294018881815957589, -1.325673485305720156, 0.6118058600197731067 ) ) ;
#32001 = CARTESIAN_POINT ( 'NONE',  ( 0.05078310099560631730, 0.4632425114130949151, -0.09919524461158422957 ) ) ;
#32002 = CARTESIAN_POINT ( 'NONE',  ( 0.1957937320930590308, -0.6579955005685824698, 0.3309870665194843964 ) ) ;
#32003 = CARTESIAN_POINT ( 'NONE',  ( 0.3543763647980864295, -1.087156323264319546, 0.7394228186721942819 ) ) ;
#32004 = EDGE_CURVE ( 'NONE', #33731, #36543, #29416, .T. ) ;
#32005 = CARTESIAN_POINT ( 'NONE',  ( 0.2923286432308245808, -1.660243258845594649, -0.6250000000000000000 ) ) ;
#32006 = DIRECTION ( 'NONE',  ( -1.000000000000000000, -0.000000000000000000, -0.000000000000000000 ) ) ;
#32007 = ORIENTED_EDGE ( 'NONE', *, *, #12448, .T. ) ;
#32008 = DIRECTION ( 'NONE',  ( 0.000000000000000000, 0.000000000000000000, -1.000000000000000000 ) ) ;
#32009 = CARTESIAN_POINT ( 'NONE',  ( 0.3742950363398350744, -1.612925599803100907, -0.4159227622875389385 ) ) ;
#32010 = CARTESIAN_POINT ( 'NONE',  ( -0.05464101615137773038, -2.626773565144302935, -0.2726934094652516127 ) ) ;
#32011 = CARTESIAN_POINT ( 'NONE',  ( -0.05082294681499039540, -0.04864283519431539249, 0.4711332289091956782 ) ) ;
#32012 = DIMENSIONAL_EXPONENTS ( 1.000000000000000000, 0.000000000000000000, 0.000000000000000000, 0.000000000000000000, 0.000000000000000000, 0.000000000000000000, 0.000000000000000000 ) ;
#32013 = ORIENTED_EDGE ( 'NONE', *, *, #37059, .F. ) ;
#32014 = CARTESIAN_POINT ( 'NONE',  ( -0.1613545236348471745, 0.5011730501304613172, 0.3493272269784281070 ) ) ;
#32015 = EDGE_CURVE ( 'NONE', #37937, #9810, #8596, .T. ) ;
#32016 = CARTESIAN_POINT ( 'NONE',  ( 0.1856296090430102352, -0.5404013791656668841, 0.2574253807303713004 ) ) ;
#32017 = CARTESIAN_POINT ( 'NONE',  ( -0.08000000000000000167, -2.320036485105098301, -0.2941690811493925528 ) ) ;
#32018 = APPLIED_DATE_AND_TIME_ASSIGNMENT ( #6102, #27940, ( #11907 ) ) ;
#32019 = FACE_OUTER_BOUND ( 'NONE', #24505, .T. ) ;
#32020 = CARTESIAN_POINT ( 'NONE',  ( 0.4713312593100775216, -1.246385543292204412, 0.6820353531022836924 ) ) ;
#32022 = CARTESIAN_POINT ( 'NONE',  ( -0.1969433606228568612, 0.5138636982738121750, 0.3749999999999991673 ) ) ;
#32021 = DIRECTION ( 'NONE',  ( 1.000000000000000000, 0.000000000000000000, 0.000000000000000000 ) ) ;
#32023 = CARTESIAN_POINT ( 'NONE',  ( 0.3535325904207607950, -1.006223909752091972, 0.6094712593526115940 ) ) ;
#32024 = ORIENTED_EDGE ( 'NONE', *, *, #3352, .F. ) ;
#32025 = APPROVAL_ROLE ( '' ) ;
#32026 = CARTESIAN_POINT ( 'NONE',  ( -0.2746410161513779258, -2.511040369707300268, -0.4948468226404901804 ) ) ;
#32027 = EDGE_LOOP ( 'NONE', ( #24991, #40170, #12358, #32037 ) ) ;
#32028 = CARTESIAN_POINT ( 'NONE',  ( 0.04813743803674420257, -0.5451878913138745730, 0.2046468533792761557 ) ) ;
#32030 = CARTESIAN_POINT ( 'NONE',  ( 0.1914787914739641550, -0.6027522233316701117, 0.3101915462042573179 ) ) ;
#32029 = CARTESIAN_POINT ( 'NONE',  ( 0.08533513956138601142, -0.8071986176931464918, 0.1158118763067559620 ) ) ;
#32031 = CARTESIAN_POINT ( 'NONE',  ( 0.3496751906377999486, -1.633240291291184088, -0.3739997235031339851 ) ) ;
#32032 = ORIENTED_EDGE ( 'NONE', *, *, #13037, .F. ) ;
#32033 = ORIENTED_EDGE ( 'NONE', *, *, #18311, .T. ) ;
#32034 = ORIENTED_EDGE ( 'NONE', *, *, #35816, .T. ) ;
#32035 = CARTESIAN_POINT ( 'NONE',  ( 0.3463719972086996557, -1.282768887459493579, 0.5758666892380096547 ) ) ;
#32036 = CARTESIAN_POINT ( 'NONE',  ( 0.5665446819737203210, -1.503126282076129083, 0.5658065823788898108 ) ) ;
#32037 = ORIENTED_EDGE ( 'NONE', *, *, #12304, .F. ) ;
#32038 = CARTESIAN_POINT ( 'NONE',  ( 0.5262299346437796510, -1.635933710071385550, -0.4253948248519428543 ) ) ;
#32039 = DIRECTION ( 'NONE',  ( 0.000000000000000000, -0.3090169943749375148, 0.9510565162951567508 ) ) ;
#32040 = CARTESIAN_POINT ( 'NONE',  ( -0.07216878364870325802, 0.000000000000000000, -0.1249999999999999029 ) ) ;
#32041 = EDGE_CURVE ( 'NONE', #8281, #22890, #30971, .T. ) ;
#32042 = CARTESIAN_POINT ( 'NONE',  ( 0.1864550573006002465, -0.7573172630633775437, 0.1903174488078394899 ) ) ;
#32043 = FACE_OUTER_BOUND ( 'NONE', #8076, .T. ) ;
#32044 = CARTESIAN_POINT ( 'NONE',  ( 0.08681952791238080336, -1.461498312203829864, -0.3696288966504583939 ) ) ;
#32045 = DIRECTION ( 'NONE',  ( 0.000000000000000000, 0.000000000000000000, -1.000000000000000000 ) ) ;
#32046 = MANIFOLD_SOLID_BREP ( 'Fillet2', #32579 ) ;
#32047 = EDGE_CURVE ( 'NONE', #27531, #16107, #20971, .T. ) ;
#32048 = B_SPLINE_CURVE_WITH_KNOTS ( 'NONE', 3,
 ( #16882, #29618, #19371, #35794, #872, #32290 ),
 .UNSPECIFIED., .F., .F.,
 ( 4, 2, 4 ),
 ( 0.000000000000000000, 0.0004418112746277370710, 0.0008836225492554741420 ),
 .UNSPECIFIED. ) ;
#32049 = DIRECTION ( 'NONE',  ( -0.000000000000000000, 0.9679004486746793923, 0.2513338844154409668 ) ) ;
#32050 = EDGE_CURVE ( 'NONE', #14981, #33895, #36782, .T. ) ;
#32051 = CARTESIAN_POINT ( 'NONE',  ( 0.3961980758757063792, -2.017725590686155979, -0.5051786489766182386 ) ) ;
#32052 = CARTESIAN_POINT ( 'NONE',  ( 2.793950402287933479E-16, -1.219177958431796432E-16, 0.1849999999999994982 ) ) ;
#32053 = LINE ( 'NONE', #31451, #36277 ) ;
#32054 = DATE_AND_TIME ( #10643, #37762 ) ;
#32055 = EDGE_CURVE ( 'NONE', #26063, #15823, #27691, .T. ) ;
#32056 = DIRECTION ( 'NONE',  ( -1.000000000000000000, -2.280301054154495132E-31, 1.664003471950577689E-31 ) ) ;
#32057 = DIRECTION ( 'NONE',  ( -1.387778780781449225E-15, 6.402768735150633127E-16, -1.000000000000000000 ) ) ;
#32058 = FACE_OUTER_BOUND ( 'NONE', #24170, .T. ) ;
#32059 = ADVANCED_FACE ( 'NONE', ( #15399 ), #7869, .F. ) ;
#32060 = CARTESIAN_POINT ( 'NONE',  ( 0.2589997918842421032, -1.679437038669657101, 0.5654899826020431952 ) ) ;
#32061 = CARTESIAN_POINT ( 'NONE',  ( 0.2631702476264848878, -1.684641432726900812, 0.5623523273860218108 ) ) ;
#32062 = CARTESIAN_POINT ( 'NONE',  ( -8.537024980200822558E-17, -0.6872203660140400183, 0.1290053960929137267 ) ) ;
#32063 = CARTESIAN_POINT ( 'NONE',  ( 0.5834517445836356897, -1.469888346549154123, -0.4281759616558344361 ) ) ;
#32064 = CARTESIAN_POINT ( 'NONE',  ( -2.125292368820994835E-14, -2.097675824466503691, -0.2907077406111384654 ) ) ;
#32065 = CARTESIAN_POINT ( 'NONE',  ( 0.02953079040095673430, -0.2329676531120430660, 0.4763574306556350169 ) ) ;
#32066 = CARTESIAN_POINT ( 'NONE',  ( 0.3261429079507188744, -1.179155933352486141, 0.4282554876890583562 ) ) ;
#32067 = ORIENTED_EDGE ( 'NONE', *, *, #1882, .F. ) ;
#32068 = ORIENTED_EDGE ( 'NONE', *, *, #36088, .F. ) ;
#32069 = EDGE_CURVE ( 'NONE', #38442, #35047, #30289, .T. ) ;
#32070 = DIRECTION ( 'NONE',  ( -2.563099466555624080E-12, -0.5877852522924748024, -0.8090169943749461190 ) ) ;
#32071 = EDGE_LOOP ( 'NONE', ( #16537, #30469, #31014, #32127 ) ) ;
#32072 = DIRECTION ( 'NONE',  ( 0.000000000000000000, 3.885780586188049371E-16, 1.000000000000000000 ) ) ;
#32073 = APPROVAL ( #14804, 'UNSPECIFIED' ) ;
#32074 = CARTESIAN_POINT ( 'NONE',  ( 0.3553889254481614746, -1.722186678249592262, -0.4852332081978528167 ) ) ;
#32075 = CARTESIAN_POINT ( 'NONE',  ( 0.4315594706875046094, -1.193550431808111156, 0.7933049988976597078 ) ) ;
#32077 = ORIENTED_EDGE ( 'NONE', *, *, #39120, .F. ) ;
#32076 = CARTESIAN_POINT ( 'NONE',  ( -0.02000000000000000042, -2.230494317742474308, -0.6487310457122437146 ) ) ;
#32078 = CARTESIAN_POINT ( 'NONE',  ( 0.5505100836374232642, -1.180854739677868359, 0.6191363254822006557 ) ) ;
#32079 = ORIENTED_EDGE ( 'NONE', *, *, #31542, .T. ) ;
#32080 = CARTESIAN_POINT ( 'NONE',  ( 0.2012152395183745279, -0.6237198413727698121, 0.3371149615413488454 ) ) ;
#32081 = ORIENTED_EDGE ( 'NONE', *, *, #19687, .T. ) ;
#32082 = CARTESIAN_POINT ( 'NONE',  ( 0.2982621269202000436, -1.656938567095597614, 0.5878592735844545558 ) ) ;
#32084 = CARTESIAN_POINT ( 'NONE',  ( -0.03868264068766696234, -0.4624969084406944098, 0.1149348357506064511 ) ) ;
#32083 = CARTESIAN_POINT ( 'NONE',  ( 0.5317043845607695163, -1.659957901717503237, -0.4539538042794677986 ) ) ;
#32085 = DIRECTION ( 'NONE',  ( 0.3981087504120420228, -0.9173382270707802766, 0.000000000000000000 ) ) ;
#32086 = CARTESIAN_POINT ( 'NONE',  ( 0.01187895423176401136, -0.5576892020588504195, -0.07857960794242428715 ) ) ;
#32087 = CARTESIAN_POINT ( 'NONE',  ( 0.02679060571419135048, -1.592882453846480306, -0.3460849381908203126 ) ) ;
#32089 = VERTEX_POINT ( 'NONE', #2457 ) ;
#32088 = ORIENTED_EDGE ( 'NONE', *, *, #14683, .F. ) ;
#32090 = FACE_OUTER_BOUND ( 'NONE', #4942, .T. ) ;
#32091 = CARTESIAN_POINT ( 'NONE',  ( 0.1144355769441696286, -0.9305145192040954472, 0.2393571899215944099 ) ) ;
#32092 = CARTESIAN_POINT ( 'NONE',  ( -0.04230188431063494625, 0.008729788072059678147, -0.4686063437799716791 ) ) ;
#32093 = CARTESIAN_POINT ( 'NONE',  ( 0.5956095749048035959, -1.454553929209333463, 0.7022256299952198688 ) ) ;
#32094 = CARTESIAN_POINT ( 'NONE',  ( 0.3439005628038807050, -1.201380011439704409, 0.7079972624627315358 ) ) ;
#32095 = FACE_OUTER_BOUND ( 'NONE', #2547, .T. ) ;
#32096 = DIRECTION ( 'NONE',  ( -0.9378410757839561462, -0.2807814858886641951, -0.2039996905746319089 ) ) ;
#32097 = CARTESIAN_POINT ( 'NONE',  ( 0.4591732152518574472, -1.217687017036588770, 0.5510147970674943441 ) ) ;
#32098 = EDGE_CURVE ( 'NONE', #13663, #14824, #35543, .T. ) ;
#32099 = CARTESIAN_POINT ( 'NONE',  ( 0.000000000000000000, -0.02999999999999995379, 0.000000000000000000 ) ) ;
#32100 = DIRECTION ( 'NONE',  ( 1.000000000000000000, 0.000000000000000000, 0.000000000000000000 ) ) ;
#32101 = FACE_OUTER_BOUND ( 'NONE', #8178, .T. ) ;
#32102 = PERSON_AND_ORGANIZATION ( #28500, #32463 ) ;
#32103 = EDGE_CURVE ( 'NONE', #17298, #20307, #5515, .T. ) ;
#32104 = CARTESIAN_POINT ( 'NONE',  ( 0.04575185649130927845, -0.3363955107642125353, 0.3523382570435877326 ) ) ;
#32105 = EDGE_CURVE ( 'NONE', #7716, #16211, #20380, .T. ) ;
#32106 = CARTESIAN_POINT ( 'NONE',  ( 0.2927350798623002959, -1.544518291098198715, -0.6925464747855896164 ) ) ;
#32107 = CARTESIAN_POINT ( 'NONE',  ( 0.2483187509121489445, -1.578255509793611733, -0.6753565671395465042 ) ) ;
#32108 = EDGE_CURVE ( 'NONE', #8681, #17043, #29562, .T. ) ;
#32109 = DIRECTION ( 'NONE',  ( 0.000000000000000000, 0.000000000000000000, -1.000000000000000000 ) ) ;
#32110 = CARTESIAN_POINT ( 'NONE',  ( 0.3572467526666761040, -1.837614999197383803, -0.4832994198719710033 ) ) ;
#32111 = CARTESIAN_POINT ( 'NONE',  ( -0.03171861681797786409, 0.5171399723077546584, 0.08825220573715056305 ) ) ;
#32112 = CARTESIAN_POINT ( 'NONE',  ( -1.019575837292306053, -0.04310840302198148261, 0.09999999999999975575 ) ) ;
#32113 = EDGE_CURVE ( 'NONE', #4242, #33794, #2642, .T. ) ;
#32114 = ORIENTED_EDGE ( 'NONE', *, *, #16199, .T. ) ;
#32115 = CARTESIAN_POINT ( 'NONE',  ( 0.3631564311673132206, -1.147350365566272012, 0.4353599662575116658 ) ) ;
#32116 = EDGE_LOOP ( 'NONE', ( #25863, #30744, #25186, #15835 ) ) ;
#32117 = CARTESIAN_POINT ( 'NONE',  ( 0.1052687179629149677, -1.411243498674495056, 0.5672272397140760702 ) ) ;
#32118 = DIRECTION ( 'NONE',  ( -1.000000000000000000, 0.000000000000000000, 0.000000000000000000 ) ) ;
#32119 = ADVANCED_FACE ( 'NONE', ( #40069 ), #36598, .T. ) ;
#32120 = CARTESIAN_POINT ( 'NONE',  ( 0.5943352790997880053, -1.487036568974021478, 0.5610698389965180777 ) ) ;
#32122 = ORIENTED_EDGE ( 'NONE', *, *, #25629, .T. ) ;
#32121 = CARTESIAN_POINT ( 'NONE',  ( 0.09152739630308469321, -1.274033986120670425, -0.5155029497116575543 ) ) ;
#32123 = EDGE_CURVE ( 'NONE', #5617, #2236, #38191, .T. ) ;
#32125 = ORIENTED_EDGE ( 'NONE', *, *, #29496, .F. ) ;
#32124 = ORIENTED_EDGE ( 'NONE', *, *, #20063, .T. ) ;
#32126 = CARTESIAN_POINT ( 'NONE',  ( 0.6667424451566161814, -1.554879396669469616, 0.6527706085860663920 ) ) ;
#32127 = ORIENTED_EDGE ( 'NONE', *, *, #36722, .T. ) ;
#32128 = ADVANCED_FACE ( 'NONE', ( #30424 ), #21169, .T. ) ;
#32129 = DIRECTION ( 'NONE',  ( 1.000000000000000000, -0.000000000000000000, -0.000000000000000000 ) ) ;
#32130 = DIRECTION ( 'NONE',  ( 0.000000000000000000, 0.000000000000000000, 1.000000000000000000 ) ) ;
#32131 = CALENDAR_DATE ( 2026, 13, 10 ) ;
#32132 = CARTESIAN_POINT ( 'NONE',  ( -0.001778489194304756814, -0.8469330747986113517, -0.01138449076159475312 ) ) ;
#32133 = ORIENTED_EDGE ( 'NONE', *, *, #15583, .T. ) ;
#32134 = CARTESIAN_POINT ( 'NONE',  ( 0.1227777051252067902, -0.8276546441510483909, 0.4419462746931263064 ) ) ;
#32135 =( REPRESENTATION_RELATIONSHIP ('NONE','NONE', #27514, #9349 ) REPRESENTATION_RELATIONSHIP_WITH_TRANSFORMATION ( #36875 )SHAPE_REPRESENTATION_RELATIONSHIP( ) );
#32136 = CARTESIAN_POINT ( 'NONE',  ( 0.3616412802241143476, -1.759290408630900693, -0.5212859374495405484 ) ) ;
#32137 = CARTESIAN_POINT ( 'NONE',  ( 0.2441247229987116574, -0.9568115778297857643, 0.7460559785473861449 ) ) ;
#32138 = ORIENTED_EDGE ( 'NONE', *, *, #30646, .T. ) ;
#32139 = CARTESIAN_POINT ( 'NONE',  ( 0.5854253530110696824, -1.600634416322008979, -0.5807582330271072735 ) ) ;
#32140 = CARTESIAN_POINT ( 'NONE',  ( 0.4159916692016358830, -1.069406866067976081, -0.5155029497116575543 ) ) ;
#32141 = CARTESIAN_POINT ( 'NONE',  ( 0.6984911126381643243, -1.438784201617487213, 0.5700049453098480212 ) ) ;
#32142 = CARTESIAN_POINT ( 'NONE',  ( 0.3580783248953228193, -1.750072000699193886, 0.5928448878684623446 ) ) ;
#32143 = CARTESIAN_POINT ( 'NONE',  ( -0.1339136704200473982, -0.4685718226220191851, 0.3606502365330779836 ) ) ;
#32144 = CARTESIAN_POINT ( 'NONE',  ( 0.4932954302610373931, -1.588333833162793862, -0.5706078562424887757 ) ) ;
#32145 = CARTESIAN_POINT ( 'NONE',  ( 0.5577295431261173331, -1.410318962983360569, 0.7650052283543964382 ) ) ;
#32146 = CARTESIAN_POINT ( 'NONE',  ( -2.184821959533202540E-05, -0.8965584091505671704, -0.01106805737880345482 ) ) ;
#32147 = EDGE_CURVE ( 'NONE', #2067, #25764, #21392, .T. ) ;
#32148 = CARTESIAN_POINT ( 'NONE',  ( -0.1073276781670975538, -0.4890918960634570989, 0.09878957693462706025 ) ) ;
#32149 = CARTESIAN_POINT ( 'NONE',  ( 0.4697623592636160361, -1.061459377010899541, -0.6056023639864149821 ) ) ;
#32150 = EDGE_CURVE ( 'NONE', #37816, #40536, #11814, .T. ) ;
#32151 = CARTESIAN_POINT ( 'NONE',  ( 0.009238630504655715933, -0.9704941665429688280, 0.5327612241319219510 ) ) ;
#32152 = CARTESIAN_POINT ( 'NONE',  ( 0.5137780172988268834, -1.118801028709976109, 0.5682417262808779901 ) ) ;
#32153 = DATE_AND_TIME ( #3774, #1699 ) ;
#32154 = PLANE ( 'NONE',  #10301 ) ;
#32155 = CARTESIAN_POINT ( 'NONE',  ( 0.3699999999999786793, -2.143627883852845528, -0.5325888117242428832 ) ) ;
#32156 = CARTESIAN_POINT ( 'NONE',  ( -0.2300000000000000100, 0.5182417262804744906, 0.3749999999999995559 ) ) ;
#32157 = ORIENTED_EDGE ( 'NONE', *, *, #32069, .T. ) ;
#32158 = CARTESIAN_POINT ( 'NONE',  ( 0.4575003298888031256, -1.565075629471692320, 0.5772771306695322346 ) ) ;
#32159 = CARTESIAN_POINT ( 'NONE',  ( 0.002367394983765177055, -0.5282119844061777814, 0.1369805761320312121 ) ) ;
#32160 = CARTESIAN_POINT ( 'NONE',  ( 0.08693319772243246479, -0.7265168537571531360, 0.02880095135038760606 ) ) ;
#32161 = ORIENTED_EDGE ( 'NONE', *, *, #9139, .F. ) ;
#32162 = ADVANCED_FACE ( 'NONE', ( #33929 ), #24679, .T. ) ;
#32163 = CARTESIAN_POINT ( 'NONE',  ( 0.4972320539234349468, -1.080138254241686413, 0.5197417262808780025 ) ) ;
#32164 = CARTESIAN_POINT ( 'NONE',  ( 0.4683780286950792182, -1.066659082333339059, 0.7984748632466120988 ) ) ;
#32166 = ORIENTED_EDGE ( 'NONE', *, *, #32147, .T. ) ;
#32165 = ORIENTED_EDGE ( 'NONE', *, *, #28012, .T. ) ;
#32167 = CARTESIAN_POINT ( 'NONE',  ( -0.2399999999999999079, -2.139295658456680904, -0.2024034539465678073 ) ) ;
#32168 = ORIENTED_EDGE ( 'NONE', *, *, #9491, .T. ) ;
#32169 = CARTESIAN_POINT ( 'NONE',  ( 0.3624061103390766592, -1.968824918581878025, -0.4968426515054770176 ) ) ;
#32170 = CYLINDRICAL_SURFACE ( 'NONE', #20025, 0.09249999999977555343 ) ;
#32171 = ORIENTED_EDGE ( 'NONE', *, *, #22101, .T. ) ;
#32172 = CARTESIAN_POINT ( 'NONE',  ( 0.009057834069440865235, -0.6081530143950221179, 0.008737474963860569765 ) ) ;
#32173 = MANIFOLD_SOLID_BREP ( 'Mirror1', #27986 ) ;
#32174 = CARTESIAN_POINT ( 'NONE',  ( 0.08992510688325755508, -0.6057077997829157789, 0.1457185332388716836 ) ) ;
#32175 = CARTESIAN_POINT ( 'NONE',  ( 0.02313328105944277915, -0.6057138157609148754, 0.5881823741868851263 ) ) ;
#32176 = CARTESIAN_POINT ( 'NONE',  ( 0.08665346048445875249, -0.5632608708817946619, 0.2407920386536964441 ) ) ;
#32178 = CARTESIAN_POINT ( 'NONE',  ( 0.3768783096114195486, -1.720370743462858343, 0.4222122349756301518 ) ) ;
#32177 = CARTESIAN_POINT ( 'NONE',  ( 0.4939403457259635144, -1.587801743525764975, -0.4617121892232378122 ) ) ;
#32179 = CARTESIAN_POINT ( 'NONE',  ( 0.4929465528686921560, -1.082715557938388029, 0.5757886449898332870 ) ) ;
#32180 = VERTEX_POINT ( 'NONE', #19303 ) ;
#32181 = ORIENTED_EDGE ( 'NONE', *, *, #18740, .T. ) ;
#32182 = CARTESIAN_POINT ( 'NONE',  ( 0.3242776434854518497, -1.641852578769815718, 0.5412648777784947463 ) ) ;
#32183 = CARTESIAN_POINT ( 'NONE',  ( 0.2207973309884857516, -1.612506204770620455, -0.3262751652180214679 ) ) ;
#32184 = CARTESIAN_POINT ( 'NONE',  ( -0.04229883635637934902, 0.2789693855191321403, -0.3765531589812268209 ) ) ;
#32185 =( BOUNDED_SURFACE ( )  B_SPLINE_SURFACE ( 3, 2, ( 
 ( #13120, #37824, #9639 ),
 ( #34931, #3462, #9216 ),
 ( #38214, #35142, #12938 ),
 ( #25485, #6738, #37403 ),
 ( #38021, #9830, #16231 ),
 ( #19313, #31854, #3672 ),
 ( #6946, #19518, #32051 ),
 ( #28953, #5411, #4052 ),
 ( #17976, #19701, #1776 ),
 ( #27043, #39377, #30536 ),
 ( #36284, #39572, #38418 ),
 ( #30131, #16617, #14691 ),
 ( #4802, #7134, #29166 ),
 ( #5021, #11619, #1028 ),
 ( #10255, #10441, #29936 ),
 ( #1959, #26850, #23003 ),
 ( #14473, #11199, #26107 ),
 ( #14288, #23763, #17378 ),
 ( #22823, #17586, #33214 ),
 ( #39787, #11405, #23973 ),
 ( #32233, #13539, #38621 ),
 ( #35527, #35343, #24177 ),
 ( #17768, #7328, #8102 ),
 ( #36505, #13326, #20680 ),
 ( #8317, #5218, #36702 ),
 ( #20887, #19906, #32996 ) ),
 .UNSPECIFIED., .F., .F., .F. ) 
 B_SPLINE_SURFACE_WITH_KNOTS ( ( 4, 2, 2, 2, 2, 2, 2, 2, 2, 2, 2, 2, 4 ),
 ( 3, 3 ),
 ( 0.03478970966414503263, 0.03529932688707621696, 0.03580894411000740130, 0.03682817855586976996, 0.03886664744759451423, 0.04090511633931925850, 0.04294358523104399583, 0.04498205412276873316, 0.04600128856863110183, 0.04702052301449347743, 0.04803975746035585304, 0.04905899190621822170, 0.05109746079794295903 ),
 ( 0.000000000000000000, 1.000000000000000000 ),
 .UNSPECIFIED. ) 
 GEOMETRIC_REPRESENTATION_ITEM ( )  RATIONAL_B_SPLINE_SURFACE ( (
 ( 1.000000000000000000, 0.7053326528219874270, 1.000000000000000000),
 ( 1.000000000000000000, 0.7069087193608286634, 1.000000000000000000),
 ( 1.000000000000000000, 0.7074454249098807157, 1.000000000000000000),
 ( 1.000000000000000000, 0.7079727039066889827, 1.000000000000000000),
 ( 1.000000000000000000, 0.7079140579849851900, 1.000000000000000000),
 ( 1.000000000000000000, 0.7072990859638627059, 1.000000000000000000),
 ( 1.000000000000000000, 0.7062992663257997572, 1.000000000000000000),
 ( 1.000000000000000000, 0.7026654075174076919, 1.000000000000000000),
 ( 1.000000000000000000, 0.6993568048661583658, 1.000000000000000000),
 ( 1.000000000000000000, 0.6923303540839972348, 1.000000000000000000),
 ( 1.000000000000000000, 0.6885467396574445065, 1.000000000000000000),
 ( 1.000000000000000000, 0.6809569680526224023, 1.000000000000000000),
 ( 1.000000000000000000, 0.6771650901614095774, 1.000000000000000000),
 ( 1.000000000000000000, 0.6704471956692915624, 1.000000000000000000),
 ( 1.000000000000000000, 0.6675067785250806685, 1.000000000000000000),
 ( 1.000000000000000000, 0.6649784099743589749, 1.000000000000000000),
 ( 1.000000000000000000, 0.6644567522674703630, 1.000000000000000000),
 ( 1.000000000000000000, 0.6643594168463616834, 1.000000000000000000),
 ( 1.000000000000000000, 0.6647836916441944854, 1.000000000000000000),
 ( 1.000000000000000000, 0.6667676599422263095, 1.000000000000000000),
 ( 1.000000000000000000, 0.6683270600133986994, 1.000000000000000000),
 ( 1.000000000000000000, 0.6727537477507504748, 1.000000000000000000),
 ( 1.000000000000000000, 0.6756357399904314720, 1.000000000000000000),
 ( 1.000000000000000000, 0.6860398255729156514, 1.000000000000000000),
 ( 1.000000000000000000, 0.6954024235277513899, 1.000000000000000000),
 ( 1.000000000000000000, 0.7067908011272805435, 1.000000000000000000) ) ) 
 REPRESENTATION_ITEM ( '' )  SURFACE ( )  );
#32186 = CARTESIAN_POINT ( 'NONE',  ( 0.000000000000000000, 0.6304109427692223822, -0.1442409525262416947 ) ) ;
#32187 = EDGE_CURVE ( 'NONE', #16904, #9810, #27921, .T. ) ;
#32188 = CARTESIAN_POINT ( 'NONE',  ( 0.5429545225213536774, -1.169342262964648826, 0.5420566649409339632 ) ) ;
#32189 = CARTESIAN_POINT ( 'NONE',  ( 0.6566606523871314494, -1.361328185136354119, 0.7219929986176217840 ) ) ;
#32190 = DIRECTION ( 'NONE',  ( -0.5115305431914159984, 0.8592650949400278959, 0.000000000000000000 ) ) ;
#32191 = CARTESIAN_POINT ( 'NONE',  ( 0.01609855503149690281, -0.8901359181507617624, 0.5067106340194477143 ) ) ;
#32192 = AXIS2_PLACEMENT_3D ( 'NONE', #2825, #15374, #18056 ) ;
#32193 = CARTESIAN_POINT ( 'NONE',  ( 0.04575185649130717597, 0.4792489163483486525, -0.08731931755211801149 ) ) ;
#32194 = CARTESIAN_POINT ( 'NONE',  ( 0.5090125390690136697, -1.650034892930424268, -0.5917945072846980681 ) ) ;
#32195 = CARTESIAN_POINT ( 'NONE',  ( 0.3198275229399000219, -1.030254701108176185, 0.7542690204297112233 ) ) ;
#32196 = CARTESIAN_POINT ( 'NONE',  ( 0.04229956186878594537, -0.2825373843407186225, 0.3739591931584704820 ) ) ;
#32197 = CARTESIAN_POINT ( 'NONE',  ( 0.1851558620279397105, -1.247064763968795287, -0.6244862546769320844 ) ) ;
#32198 = AXIS2_PLACEMENT_3D ( 'NONE', #18604, #31545, #5829 ) ;
#32199 = ORIENTED_EDGE ( 'NONE', *, *, #28710, .T. ) ;
#32200 = FACE_OUTER_BOUND ( 'NONE', #2817, .T. ) ;
#32201 = CARTESIAN_POINT ( 'NONE',  ( 0.5828811169494957367, -1.432893170591135190, 0.6998973824865686311 ) ) ;
#32202 = CARTESIAN_POINT ( 'NONE',  ( 0.3658297366832102271, -1.745592370396174875, -0.4954708084374069288 ) ) ;
#32203 = CARTESIAN_POINT ( 'NONE',  ( 0.3918182118607624331, -1.107073211027153725, 0.6042946153017959565 ) ) ;
#32204 = CARTESIAN_POINT ( 'NONE',  ( 0.07659484908144738313, -0.8729867003811840886, 0.4791183106292659089 ) ) ;
#32205 = ORIENTED_EDGE ( 'NONE', *, *, #1221, .F. ) ;
#32206 = CARTESIAN_POINT ( 'NONE',  ( 0.3788106256558574914, -1.616048764795402937, -0.3641495012956140198 ) ) ;
#32207 = CARTESIAN_POINT ( 'NONE',  ( 0.4869195250931122043, -1.660191309538731286, 0.5031962290216808187 ) ) ;
#32208 = DIRECTION ( 'NONE',  ( 0.4999999999999985567, -0.7377595849475284684, -0.4535535192433764462 ) ) ;
#32209 = CARTESIAN_POINT ( 'NONE',  ( 0.4500590111990616093, -1.213600599699063531, 0.6848325471722976898 ) ) ;
#32211 = CARTESIAN_POINT ( 'NONE',  ( 0.3161404488835721782, -1.757546004036539600, 0.4995768716934911868 ) ) ;
#32210 = CARTESIAN_POINT ( 'NONE',  ( 0.4419048264408250715, -1.686280600454902245, 0.4284299735159858291 ) ) ;
#32212 = CARTESIAN_POINT ( 'NONE',  ( 0.3845716336272441138, -1.023253965646789831, 0.6260147105531964629 ) ) ;
#32213 = ORIENTED_EDGE ( 'NONE', *, *, #21830, .F. ) ;
#32214 = CARTESIAN_POINT ( 'NONE',  ( -0.2399999999999999079, -3.941790907013290823, -0.2762780017083287243 ) ) ;
#32215 = VERTEX_POINT ( 'NONE', #32040 ) ;
#32216 = CARTESIAN_POINT ( 'NONE',  ( 0.3728004488347659295, -1.485653693715612622, 0.8362323834158711389 ) ) ;
#32218 = CARTESIAN_POINT ( 'NONE',  ( 0.2019560640872724577, -0.6669419321649556753, 0.3380954050266351540 ) ) ;
#32217 = CARTESIAN_POINT ( 'NONE',  ( 0.06660121735839297230, -0.7068563761969431924, -0.0009791055646058395914 ) ) ;
#32219 = DIRECTION ( 'NONE',  ( 1.000000000000000000, 2.280301054154495132E-31, -1.664003471950577689E-31 ) ) ;
#32220 = ORIENTED_EDGE ( 'NONE', *, *, #36145, .T. ) ;
#32221 = CIRCLE ( 'NONE', #9228, 0.1000000000000000194 ) ;
#32222 = CARTESIAN_POINT ( 'NONE',  ( -0.2399999999999999079, -3.667123564397057667, -0.3682398926280779361 ) ) ;
#32223 = CARTESIAN_POINT ( 'NONE',  ( 0.1201110248123422458, -0.5699891019612776111, 0.2421155355894170913 ) ) ;
#32224 = ORIENTED_EDGE ( 'NONE', *, *, #24249, .T. ) ;
#32225 = CARTESIAN_POINT ( 'NONE',  ( 0.07279848815817739627, -1.323290893158621584, 0.4931731530909873040 ) ) ;
#32226 = CARTESIAN_POINT ( 'NONE',  ( 0.001665905518637939096, -1.790954619074065945, -0.3617774004250685072 ) ) ;
#32227 = VECTOR ( 'NONE', #38281, 39.37007874015748854 ) ;
#32228 = DIRECTION ( 'NONE',  ( 1.000000000000000000, 0.000000000000000000, 0.000000000000000000 ) ) ;
#32229 = AXIS2_PLACEMENT_3D ( 'NONE', #13418, #15689, #12819 ) ;
#32230 = DIRECTION ( 'NONE',  ( -9.860761315262646473E-32, -0.8518913899333638851, -0.5237184928541300799 ) ) ;
#32231 = CARTESIAN_POINT ( 'NONE',  ( 0.08752222435001974499, -0.6850407580105462024, 0.1042154167643189189 ) ) ;
#32232 = CARTESIAN_POINT ( 'NONE',  ( 0.7426951793279046310, -1.510662807742832348, 0.6358527240479500131 ) ) ;
#32233 = CARTESIAN_POINT ( 'NONE',  ( 0.2100158411153514038, -1.623712120995903341, -0.6928538852213783628 ) ) ;
#32234 = LINE ( 'NONE', #32052, #27328 ) ;
#32235 = CARTESIAN_POINT ( 'NONE',  ( 0.09721366830544136972, -1.364942592095733209, 0.6896469871951299568 ) ) ;
#32236 = APPROVAL_DATE_TIME ( #16836, #11684 ) ;
#32237 = CARTESIAN_POINT ( 'NONE',  ( 0.6635990329685389488, -1.451118425079158891, -0.6162234092229578186 ) ) ;
#32238 = CARTESIAN_POINT ( 'NONE',  ( 0.04946426091936848013, 0.2513512500265263072, 0.4057590668656822497 ) ) ;
#32239 = CARTESIAN_POINT ( 'NONE',  ( -0.2399999999999999079, -3.941790907013290823, -0.4709369376873030477 ) ) ;
#32240 = CARTESIAN_POINT ( 'NONE',  ( -0.2399999999999999079, -3.812085038045152974, -0.02801711824816583915 ) ) ;
#32241 = CARTESIAN_POINT ( 'NONE',  ( -0.3000000000000000999, -2.183180860297908144, -0.5562760292030870524 ) ) ;
#32242 = CARTESIAN_POINT ( 'NONE',  ( 0.04402670621142950463, -0.8156408044542829971, 0.6980404683681784572 ) ) ;
#32243 = CARTESIAN_POINT ( 'NONE',  ( -3.228764966566807510E-05, -0.7201249671145206754, -0.1017258316044593325 ) ) ;
#32244 = VECTOR ( 'NONE', #34610, 39.37007874015748143 ) ;
#32245 = DIRECTION ( 'NONE',  ( 1.000000000000000000, -0.000000000000000000, -0.000000000000000000 ) ) ;
#32246 = CARTESIAN_POINT ( 'NONE',  ( 0.7305197500123582488, -1.560475142278366478, 0.5182417262812423209 ) ) ;
#32247 = ORIENTED_EDGE ( 'NONE', *, *, #22464, .F. ) ;
#32248 = ORIENTED_EDGE ( 'NONE', *, *, #33306, .F. ) ;
#32249 = TOROIDAL_SURFACE ( 'NONE', #10561, 1.986674066779348768, 0.01499999999999999944 ) ;
#32250 = DIRECTION ( 'NONE',  ( 1.000000000000000000, 2.280301054154495132E-31, -1.664003471950577689E-31 ) ) ;
#32251 = VERTEX_POINT ( 'NONE', #3066 ) ;
#32252 = AXIS2_PLACEMENT_3D ( 'NONE', #23339, #7675, #20239 ) ;
#32253 = DIRECTION ( 'NONE',  ( 0.8660512985181132439, 0.4999551463232376758, 0.000000000000000000 ) ) ;
#32254 = CARTESIAN_POINT ( 'NONE',  ( 0.3433798484762162762, -1.649580330210344226, -0.4420781474354099072 ) ) ;
#32255 = AXIS2_PLACEMENT_3D ( 'NONE', #1212, #38799, #13530 ) ;
#32256 = CARTESIAN_POINT ( 'NONE',  ( 0.5211167752495460270, -1.329540253312506914, 0.7191629022700860574 ) ) ;
#32258 = ORIENTED_EDGE ( 'NONE', *, *, #5199, .T. ) ;
#32257 = CARTESIAN_POINT ( 'NONE',  ( -0.2399999999999999079, -3.334889855281614857, -0.6641625420049475093 ) ) ;
#32259 = CARTESIAN_POINT ( 'NONE',  ( 0.1912825281910040254, -0.6944471949468554728, 0.2480975638430023278 ) ) ;
#32260 = EDGE_CURVE ( 'NONE', #27640, #35830, #40151, .T. ) ;
#32261 = CARTESIAN_POINT ( 'NONE',  ( 0.3391898079600526028, -1.708268844615858484, -0.6004883020675078065 ) ) ;
#32262 = ORIENTED_EDGE ( 'NONE', *, *, #13793, .T. ) ;
#32263 = CARTESIAN_POINT ( 'NONE',  ( 0.6004930002435877601, -1.482345764245047937, -0.6229362720418619714 ) ) ;
#32264 = EDGE_CURVE ( 'NONE', #19390, #10166, #6635, .T. ) ;
#32265 = EDGE_LOOP ( 'NONE', ( #19549, #11932, #460, #7570 ) ) ;
#32266 = CARTESIAN_POINT ( 'NONE',  ( 0.02322713698175598793, -0.5357957426655662880, 0.1845586416323105050 ) ) ;
#32268 = LINE ( 'NONE', #25712, #1867 ) ;
#32267 = CARTESIAN_POINT ( 'NONE',  ( 0.5361355449682986274, -1.657745371039847759, -0.4610437686141751201 ) ) ;
#32269 = LINE ( 'NONE', #473, #22772 ) ;
#32270 = ADVANCED_FACE ( 'NONE', ( #3453 ), #28761, .T. ) ;
#32271 = CARTESIAN_POINT ( 'NONE',  ( 0.03256590615868563965, -1.845618522021015728, -0.3210350534622004592 ) ) ;
#32272 = VERTEX_POINT ( 'NONE', #6333 ) ;
#32273 = AXIS2_PLACEMENT_3D ( 'NONE', #28148, #13105, #25665 ) ;
#32274 = DIMENSIONAL_EXPONENTS ( 1.000000000000000000, 0.000000000000000000, 0.000000000000000000, 0.000000000000000000, 0.000000000000000000, 0.000000000000000000, 0.000000000000000000 ) ;
#32275 = EDGE_CURVE ( 'NONE', #40017, #1162, #16011, .T. ) ;
#32276 = DIRECTION ( 'NONE',  ( -0.8660254037844415942, 0.4219433715391002759, 0.2682606777263707998 ) ) ;
#32277 = CARTESIAN_POINT ( 'NONE',  ( 0.2988694321510503848, -0.9099035776915582741, 0.5838633149813420298 ) ) ;
#32278 = CARTESIAN_POINT ( 'NONE',  ( 0.1999999999999789724, -2.183180860297921466, -0.2737760292030870235 ) ) ;
#32279 = CARTESIAN_POINT ( 'NONE',  ( 0.5672114294812768964, -1.448954238197414757, 0.7332268910936999839 ) ) ;
#32280 = CARTESIAN_POINT ( 'NONE',  ( 0.3950454177327251681, -1.172102527061769983, 0.7080655069546051283 ) ) ;
#32281 = CARTESIAN_POINT ( 'NONE',  ( 0.06420656066988442157, -0.8824955108432496198, 0.7451941067001949248 ) ) ;
#32282 = AXIS2_PLACEMENT_3D ( 'NONE', #8860, #3290, #6776 ) ;
#32283 = CARTESIAN_POINT ( 'NONE',  ( 0.4687039633801927674, -1.165676228951822546, 0.4182417262808778013 ) ) ;
#32284 = CARTESIAN_POINT ( 'NONE',  ( -0.1631341089705869718, 0.4729174206798188451, 0.3373594846482096399 ) ) ;
#32285 = CIRCLE ( 'NONE', #38830, 0.2000000000000000111 ) ;
#32286 = CARTESIAN_POINT ( 'NONE',  ( -0.2399999999999999079, -2.289343986263487896, -0.7686455968847020204 ) ) ;
#32287 = VECTOR ( 'NONE', #34165, 39.37007874015748854 ) ;
#32288 = DIRECTION ( 'NONE',  ( 0.4999551463232372317, -0.8660512985181135770, 0.000000000000000000 ) ) ;
#32289 = ADVANCED_FACE ( 'NONE', ( #18906, #38014, #22395, #31443, #3250, #620 ), #12507, .F. ) ;
#32290 = CARTESIAN_POINT ( 'NONE',  ( 0.4291849790131893050, -1.119523916798046859, -0.6481113851292223949 ) ) ;
#32291 = APPLIED_PERSON_AND_ORGANIZATION_ASSIGNMENT ( #16026, #40505, ( #19398 ) ) ;
#32292 = VECTOR ( 'NONE', #8670, 39.37007874015748143 ) ;
#32293 = CARTESIAN_POINT ( 'NONE',  ( 0.03113248654051816583, -0.4578766358967566452, -0.4053162176620347945 ) ) ;
#32294 = DIRECTION ( 'NONE',  ( 0.000000000000000000, 0.000000000000000000, 1.000000000000000000 ) ) ;
#32295 = CARTESIAN_POINT ( 'NONE',  ( 0.1781635123675364418, -1.733799861008286758, -0.6515288039002870013 ) ) ;
#32296 = DIRECTION ( 'NONE',  ( 0.4999999999999973910, -0.8563665354314760059, -0.1289820025937470083 ) ) ;
#32297 = CARTESIAN_POINT ( 'NONE',  ( 0.1748197985926945586, -1.826458824642884782, -0.6524116373567239169 ) ) ;
#32298 = DIRECTION ( 'NONE',  ( 8.881784197001246407E-16, -2.361472542561082612E-16, 1.000000000000000000 ) ) ;
#32299 = CARTESIAN_POINT ( 'NONE',  ( 0.2409193767872376546, -1.343661558146008073, -0.2869361388274795921 ) ) ;
#32300 = EDGE_CURVE ( 'NONE', #30159, #20992, #24408, .T. ) ;
#32301 = ORIENTED_EDGE ( 'NONE', *, *, #30569, .T. ) ;
#32302 = CARTESIAN_POINT ( 'NONE',  ( 0.3795613398208534384, -1.760143698493221942, -0.5723197561600823491 ) ) ;
#32303 = VERTEX_POINT ( 'NONE', #16222 ) ;
#32304 = DIRECTION ( 'NONE',  ( 0.000000000000000000, 0.000000000000000000, -1.000000000000000000 ) ) ;
#32305 = CIRCLE ( 'NONE', #37561, 0.08000000000000000167 ) ;
#32306 = CARTESIAN_POINT ( 'NONE',  ( 0.4067172716121477127, -1.179764143288656086, 0.8178903262834292809 ) ) ;
#32308 = ORIENTED_EDGE ( 'NONE', *, *, #18050, .T. ) ;
#32307 = CARTESIAN_POINT ( 'NONE',  ( 0.4738546087217575531, -1.652018268363231401, -0.3975985852014373156 ) ) ;
#32310 = ORIENTED_EDGE ( 'NONE', *, *, #24778, .F. ) ;
#32309 = ORIENTED_EDGE ( 'NONE', *, *, #26778, .F. ) ;
#32311 = CARTESIAN_POINT ( 'NONE',  ( 0.6019566843391931377, -1.400796273631349509, 0.8618335802499477172 ) ) ;
#32312 = ADVANCED_FACE ( 'NONE', ( #28347 ), #13114, .T. ) ;
#32313 = CIRCLE ( 'NONE', #40182, 0.1000000000000000194 ) ;
#32314 = ORIENTED_EDGE ( 'NONE', *, *, #12395, .F. ) ;
#32315 = CARTESIAN_POINT ( 'NONE',  ( -0.2399999999999999079, -2.646062248599815092, -0.5806902395129298622 ) ) ;
#32316 = CARTESIAN_POINT ( 'NONE',  ( -0.05464101615137771650, -1.538828486247671101, 0.2167077994389897955 ) ) ;
#32317 = APPROVAL_ROLE ( '' ) ;
#32318 = AXIS2_PLACEMENT_3D ( 'NONE', #35609, #3748, #12803 ) ;
#32319 = EDGE_CURVE ( 'NONE', #13520, #16165, #10032, .T. ) ;
#32320 = EDGE_CURVE ( 'NONE', #13940, #11991, #4575, .T. ) ;
#32321 = CARTESIAN_POINT ( 'NONE',  ( -0.002121425808298199340, -0.4210325180397653244, -0.06462206035643883184 ) ) ;
#32322 = ORIENTED_EDGE ( 'NONE', *, *, #14586, .F. ) ;
#32323 = ADVANCED_FACE ( 'NONE', ( #19510 ), #36144, .T. ) ;
#32324 = CARTESIAN_POINT ( 'NONE',  ( 0.2845110416328373026, -1.007666087979148806, 0.6983705601599040635 ) ) ;
#32325 = CARTESIAN_POINT ( 'NONE',  ( 0.08991294088452159161, -0.5647436697761467617, 0.1521524643572742530 ) ) ;
#32326 = CARTESIAN_POINT ( 'NONE',  ( 0.4419887564222924614, -1.353243676712053700, 0.8323238201494266297 ) ) ;
#32327 = ORIENTED_EDGE ( 'NONE', *, *, #9195, .F. ) ;
#32328 = CARTESIAN_POINT ( 'NONE',  ( 0.1766676265724269612, -0.4909283402585992717, 0.1805520534859691439 ) ) ;
#32329 = DIRECTION ( 'NONE',  ( 0.000000000000000000, 0.000000000000000000, -1.000000000000000000 ) ) ;
#32330 = CARTESIAN_POINT ( 'NONE',  ( 0.7205019089780672070, -1.476770077061609454, 0.5381834689638800295 ) ) ;
#32331 = CARTESIAN_POINT ( 'NONE',  ( -0.1210148435730035998, -0.5061394519556905447, 0.1438724812234790928 ) ) ;
#32332 = CARTESIAN_POINT ( 'NONE',  ( 0.6657177695133712492, -1.561535871981375223, 0.5657877757939010488 ) ) ;
#32333 = DIRECTION ( 'NONE',  ( 0.4999551463232372317, -0.8660512985181135770, 0.000000000000000000 ) ) ;
#32334 = LINE ( 'NONE', #25214, #20559 ) ;
#32335 = CARTESIAN_POINT ( 'NONE',  ( 0.4721987900744024635, -1.279206107442438123, 0.8150767136317752515 ) ) ;
#32336 = CARTESIAN_POINT ( 'NONE',  ( 0.01158385750371686805, -0.8255970240247688663, -0.07329882424099665172 ) ) ;
#32337 = EDGE_CURVE ( 'NONE', #39872, #2349, #37236, .T. ) ;
#32338 = EDGE_CURVE ( 'NONE', #12540, #37319, #5946, .T. ) ;
#32339 = CIRCLE ( 'NONE', #31704, 0.5756329413417604624 ) ;
#32340 = FACE_OUTER_BOUND ( 'NONE', #8237, .T. ) ;
#32341 = CARTESIAN_POINT ( 'NONE',  ( 0.03158843595483527833, -0.4482533282648944462, -0.2030547983902471210 ) ) ;
#32342 = CARTESIAN_POINT ( 'NONE',  ( 0.09860045244982779122, -1.306187320691368337, 0.7507959704929506595 ) ) ;
#32343 = CARTESIAN_POINT ( 'NONE',  ( 0.1843752803354802017, -0.7900634509218507073, 0.1541083617713018827 ) ) ;
#32344 = COORDINATED_UNIVERSAL_TIME_OFFSET ( 0, 0, .AHEAD. ) ;
#32345 = CONICAL_SURFACE ( 'NONE', #14605, 0.1600000000000004197, 1.047197551196596743 ) ;
#32346 = AXIS2_PLACEMENT_3D ( 'NONE', #31046, #3263, #37413 ) ;
#32347 = AXIS2_PLACEMENT_3D ( 'NONE', #9711, #25762, #901 ) ;
#32348 = CARTESIAN_POINT ( 'NONE',  ( -0.03868649100028190291, 0.4417196792138938788, -0.1788567627196049059 ) ) ;
#32349 = CONICAL_SURFACE ( 'NONE', #8714, 0.01999999999999927530, 1.047197551196600962 ) ;
#32350 = EDGE_LOOP ( 'NONE', ( #15768, #34615, #22969, #40044 ) ) ;
#32351 = CARTESIAN_POINT ( 'NONE',  ( 0.3220325133609698853, -1.710602945088052884, -0.6976313533424302049 ) ) ;
#32352 = CARTESIAN_POINT ( 'NONE',  ( 0.002299670934844304584, -0.5203385876834750734, 0.1590128112158734619 ) ) ;
#32353 = CARTESIAN_POINT ( 'NONE',  ( 0.2210032901071049827, -1.227910525351944893, 0.5087335351181689891 ) ) ;
#32354 = ORIENTED_EDGE ( 'NONE', *, *, #39607, .T. ) ;
#32355 = CARTESIAN_POINT ( 'NONE',  ( 0.4971324743577882899, -1.079965756743124006, 0.4177417262808780229 ) ) ;
#32356 = CARTESIAN_POINT ( 'NONE',  ( 0.6205349385892930947, -1.302967389835202772, 0.7736340727560927499 ) ) ;
#32358 = ORIENTED_EDGE ( 'NONE', *, *, #32634, .F. ) ;
#32357 = VERTEX_POINT ( 'NONE', #34138 ) ;
#32359 = CARTESIAN_POINT ( 'NONE',  ( -2.070754768975505034, -0.09959325338431362917, 0.3749999999999976130 ) ) ;
#32360 = ORIENTED_EDGE ( 'NONE', *, *, #9486, .T. ) ;
#32361 = CARTESIAN_POINT ( 'NONE',  ( 0.3545879618755022888, -1.837530425579354754, -0.4889651724334035388 ) ) ;
#32362 = LINE ( 'NONE', #4188, #7488 ) ;
#32363 = AXIS2_PLACEMENT_3D ( 'NONE', #10487, #6786, #19367 ) ;
#32364 = EDGE_CURVE ( 'NONE', #4884, #6766, #39912, .T. ) ;
#32365 = CARTESIAN_POINT ( 'NONE',  ( -1.019575837292306053, -0.04310840302198148261, 0.09999999999999975575 ) ) ;
#32366 = ORIENTED_EDGE ( 'NONE', *, *, #2407, .T. ) ;
#32367 = DIRECTION ( 'NONE',  ( 0.000000000000000000, 0.000000000000000000, -1.000000000000000000 ) ) ;
#32368 = CARTESIAN_POINT ( 'NONE',  ( 0.2292120464367194133, -0.8985078094207066268, 0.6777055952005869299 ) ) ;
#32369 = CARTESIAN_POINT ( 'NONE',  ( 0.08687450833421726804, -0.8754084042801643095, 0.8684160286065422119 ) ) ;
#32370 = CIRCLE ( 'NONE', #12007, 0.1333070866141734812 ) ;
#32371 = CARTESIAN_POINT ( 'NONE',  ( 0.4181162624911300418, -1.391114915320552647, 0.8390373960833495959 ) ) ;
#32373 = CARTESIAN_POINT ( 'NONE',  ( 0.06980746140711582837, 0.000000000000000000, 0.000000000000000000 ) ) ;
#32372 = CARTESIAN_POINT ( 'NONE',  ( 0.1152873670910658371, -0.4465801609609503786, 0.1298222201462807257 ) ) ;
#32374 = CARTESIAN_POINT ( 'NONE',  ( 0.09902269473968819402, -0.9382648416710920314, 0.3009685187709933984 ) ) ;
#32375 = VERTEX_POINT ( 'NONE', #9053 ) ;
#32376 = EDGE_CURVE ( 'NONE', #32724, #19429, #15853, .T. ) ;
#32377 = AXIS2_PLACEMENT_3D ( 'NONE', #23485, #13983, #39095 ) ;
#32378 = CARTESIAN_POINT ( 'NONE',  ( -2.070754768975505034, -0.09959325338431362917, 0.1178658435936983939 ) ) ;
#32379 = CARTESIAN_POINT ( 'NONE',  ( 0.2153037633907589343, -0.6407961093961948018, 0.4236369251119138646 ) ) ;
#32380 = VECTOR ( 'NONE', #13125, 39.37007874015748143 ) ;
#32381 = CARTESIAN_POINT ( 'NONE',  ( -0.01548846960707455332, 0.2450655194479865739, -0.4674710490749279246 ) ) ;
#32382 =( GEOMETRIC_REPRESENTATION_CONTEXT ( 3 ) GLOBAL_UNCERTAINTY_ASSIGNED_CONTEXT ( ( #22343 ) ) GLOBAL_UNIT_ASSIGNED_CONTEXT ( ( #16516, #15698, #3954 ) ) REPRESENTATION_CONTEXT ( 'NONE', 'WORKASPACE' ) );
#32383 = CARTESIAN_POINT ( 'NONE',  ( -0.05489899477340617201, -0.4316043292239965523, -0.1669032320049002316 ) ) ;
#32384 = ADVANCED_FACE ( 'NONE', ( #27172 ), #5133, .F. ) ;
#32385 = APPLIED_PERSON_AND_ORGANIZATION_ASSIGNMENT ( #16705, #7417, ( #18145 ) ) ;
#32386 = CYLINDRICAL_SURFACE ( 'NONE', #4971, 0.1999999999999994837 ) ;
#32387 = B_SPLINE_CURVE_WITH_KNOTS ( 'NONE', 3,
 ( #38775, #35312, #785, #19873, #38589, #1190, #10606, #22970, #20094, #13293, #23180, #10826, #6701, #10411, #35491, #3637, #28735, #597 ),
 .UNSPECIFIED., .F., .F.,
 ( 4, 2, 2, 2, 2, 2, 2, 2, 4 ),
 ( -0.002633528389679661366, -0.001975271857855668677, -0.001317015326031676205, -0.0006587587942076789625, -5.022623836819367638E-07, 0.0006577542694403155227, 0.001316010801264312982, 0.001974267333088309574, 0.002632523864912307034 ),
 .UNSPECIFIED. ) ;
#32388 = ADVANCED_FACE ( 'NONE', ( #14600 ), #14393, .F. ) ;
#32389 = FACE_OUTER_BOUND ( 'NONE', #14678, .T. ) ;
#32390 = CARTESIAN_POINT ( 'NONE',  ( 0.5799898087634006716, -1.239070881731211049, 0.8001874111395332889 ) ) ;
#32391 = CARTESIAN_POINT ( 'NONE',  ( 0.4891551093075355294, -1.126829402807817626, 0.4573268544095612231 ) ) ;
#32392 = CARTESIAN_POINT ( 'NONE',  ( -0.01548846960707477016, 0.4638115001430995199, 0.2459753896937826034 ) ) ;
#32393 = CIRCLE ( 'NONE', #35694, 0.1050424246542346618 ) ;
#32394 = CARTESIAN_POINT ( 'NONE',  ( 0.02953079040095510019, 0.4684706630666146121, -0.2484463060367390341 ) ) ;
#32395 = CARTESIAN_POINT ( 'NONE',  ( 0.5313292079975693305, -1.639131752853789203, -0.5569014201383083451 ) ) ;
#32396 = EDGE_LOOP ( 'NONE', ( #21165, #25476, #11174, #5141 ) ) ;
#32397 = CARTESIAN_POINT ( 'NONE',  ( 0.2456149479727556262, -0.9794485632045497603, 0.6980560059640830151 ) ) ;
#32398 = CARTESIAN_POINT ( 'NONE',  ( 0.02869942827333496829, -0.2420058122830158198, 0.4357544236535315640 ) ) ;
#32399 = CARTESIAN_POINT ( 'NONE',  ( 0.4893454517239185231, -1.274357042672645157, 0.6057417262808995062 ) ) ;
#32400 = CIRCLE ( 'NONE', #8087, 0.1000000000000000194 ) ;
#32401 = CIRCLE ( 'NONE', #16652, 0.1620173459747806799 ) ;
#32402 = EDGE_LOOP ( 'NONE', ( #12845, #11690, #17188, #39203 ) ) ;
#32403 = DIRECTION ( 'NONE',  ( -0.7993299944781128152, -0.4614381908250200781, 0.3848978513524763390 ) ) ;
#32404 = CARTESIAN_POINT ( 'NONE',  ( 0.5337844292675856250, -1.163613296893691418, 0.5164530006208986057 ) ) ;
#32405 = CARTESIAN_POINT ( 'NONE',  ( 0.3048982267989297501, -1.756746414302344350, 0.5594309555313059512 ) ) ;
#32406 = DIRECTION ( 'NONE',  ( 0.000000000000000000, 1.951319995474454795E-15, -1.000000000000000000 ) ) ;
#32407 = AXIS2_PLACEMENT_3D ( 'NONE', #9433, #38425, #35152 ) ;
#32408 = CARTESIAN_POINT ( 'NONE',  ( 0.2700465502981880261, -1.304386535474396869, 0.6466137386760588690 ) ) ;
#32409 = ORIENTED_EDGE ( 'NONE', *, *, #18885, .T. ) ;
#32410 = CARTESIAN_POINT ( 'NONE',  ( -0.1659631349965166869, 0.5156080474714462847, 0.3322463110352252280 ) ) ;
#32411 = AXIS2_PLACEMENT_3D ( 'NONE', #25123, #19157, #22666 ) ;
#32412 = CARTESIAN_POINT ( 'NONE',  ( -8.628166150854817443E-33, -3.491513147198971704E-33, 0.2000000000000000111 ) ) ;
#32413 = DIRECTION ( 'NONE',  ( -0.4999551463232372317, 0.8660512985181133550, -0.000000000000000000 ) ) ;
#32414 = CARTESIAN_POINT ( 'NONE',  ( 0.1857376701173840405, -0.7573068233460694687, 0.1312443193538671837 ) ) ;
#32415 = CARTESIAN_POINT ( 'NONE',  ( 0.4672008347720292831, -1.238708369555474809, 0.6671083618078329502 ) ) ;
#32416 = ADVANCED_FACE ( 'NONE', ( #21195 ), #36645, .T. ) ;
#32417 = EDGE_CURVE ( 'NONE', #24392, #33731, #31620, .T. ) ;
#32419 = CARTESIAN_POINT ( 'NONE',  ( 0.01548846960707528191, -0.3772621329473441198, 0.3651003739302687290 ) ) ;
#32418 = FACE_OUTER_BOUND ( 'NONE', #10070, .T. ) ;
#32420 = CARTESIAN_POINT ( 'NONE',  ( 0.2530466182501821537, -0.9510907114987208200, 0.4863111693326979679 ) ) ;
#32421 = EDGE_LOOP ( 'NONE', ( #25234, #8379, #33225, #3875 ) ) ;
#32422 = CARTESIAN_POINT ( 'NONE',  ( 0.000000000000000000, 0.000000000000000000, 0.000000000000000000 ) ) ;
#32423 = EDGE_LOOP ( 'NONE', ( #22280, #17359, #14174, #5394 ) ) ;
#32424 =( BOUNDED_SURFACE ( )  B_SPLINE_SURFACE ( 3, 2, ( 
 ( #19410, #9920, #32141 ),
 ( #4148, #32330, #38517 ),
 ( #916, #29263, #13812 ),
 ( #20215, #17112, #16718 ),
 ( #32740, #22490, #13212 ),
 ( #13421, #25572, #7651 ),
 ( #23315, #7222, #10739 ),
 ( #6828, #4547, #38911 ) ),
 .UNSPECIFIED., .F., .F., .T. ) 
 B_SPLINE_SURFACE_WITH_KNOTS ( ( 4, 2, 2, 4 ),
 ( 3, 3 ),
 ( 0.01175530705606903266, 0.01325526436763865314, 0.01400524302342346337, 0.01475522167920827361 ),
 ( 0.4190931457273361360, 1.000000000000000000 ),
 .UNSPECIFIED. ) 
 GEOMETRIC_REPRESENTATION_ITEM ( )  RATIONAL_B_SPLINE_SURFACE ( (
 ( 0.8578808472140506680, 0.8304444319420907217, 1.000000000000000000),
 ( 0.8578018857223783655, 0.8303502267606441833, 1.000000000000000000),
 ( 0.8574190045897945867, 0.8298934295826334573, 1.000000000000000000),
 ( 0.8568921888178224755, 0.8292649108662777380, 1.000000000000000000),
 ( 0.8567216579868570658, 0.8290614586830293842, 1.000000000000000000),
 ( 0.8564019985838529081, 0.8286800883286544739, 1.000000000000000000),
 ( 0.8562511564427921495, 0.8285001257802345753, 1.000000000000000000),
 ( 0.8561112709294405043, 0.8283332350606202876, 1.000000000000000000) ) ) 
 REPRESENTATION_ITEM ( '' )  SURFACE ( )  );
#32425 = CARTESIAN_POINT ( 'NONE',  ( 0.04965443803015197333, -0.5664236144437935216, 0.2699224481367241135 ) ) ;
#32426 = DIRECTION ( 'NONE',  ( -0.8660512985181141321, -0.4999551463232362325, 0.000000000000000000 ) ) ;
#32427 = CARTESIAN_POINT ( 'NONE',  ( 0.2936582543218392294, -1.659717270275419487, 0.5856070495615782745 ) ) ;
#32428 = ORIENTED_EDGE ( 'NONE', *, *, #33516, .F. ) ;
#32429 = CIRCLE ( 'NONE', #22626, 0.1499999999999989675 ) ;
#32430 = DIRECTION ( 'NONE',  ( -0.3468893892380665034, 0.9373665302208726846, -0.03180785525185936963 ) ) ;
#32431 = CARTESIAN_POINT ( 'NONE',  ( 0.4708981006924713997, -1.339116817097131262, 0.8202851355120116539 ) ) ;
#32432 = VERTEX_POINT ( 'NONE', #37021 ) ;
#32433 = CARTESIAN_POINT ( 'NONE',  ( 0.3888736924534981765, -1.922885813500992302, -0.5052802514659558986 ) ) ;
#32434 = CARTESIAN_POINT ( 'NONE',  ( 0.01548846960706616940, -0.5203207976468143814, 0.08861466064781831076 ) ) ;
#32435 = VECTOR ( 'NONE', #5422, 39.37007874015748143 ) ;
#32436 = VECTOR ( 'NONE', #9054, 39.37007874015748143 ) ;
#32437 = CARTESIAN_POINT ( 'NONE',  ( 0.1852770244791848431, -0.8385451057929541596, 0.1525445887411581436 ) ) ;
#32438 = PRODUCT_DEFINITION_SHAPE ( 'NONE', 'NONE',  #40652 ) ;
#32439 = CARTESIAN_POINT ( 'NONE',  ( 0.4194637470453334571, -1.704445962963519134, 0.4281874859184326976 ) ) ;
#32440 = FACE_OUTER_BOUND ( 'NONE', #31067, .T. ) ;
#32441 = DIRECTION ( 'NONE',  ( 1.000000000000000000, 0.000000000000000000, 0.000000000000000000 ) ) ;
#32442 = CARTESIAN_POINT ( 'NONE',  ( 0.6952872927582756102, -1.427253715223001374, 0.8000406204621429707 ) ) ;
#32443 = CIRCLE ( 'NONE', #960, 0.01500000000000000291 ) ;
#32444 = CARTESIAN_POINT ( 'NONE',  ( 0.1999999999999789724, -2.107936428766273629, -0.7005084057759867200 ) ) ;
#32445 = CARTESIAN_POINT ( 'NONE',  ( 0.01895884884825209393, -0.3622979475331352117, -0.3730907371368787917 ) ) ;
#32446 = COORDINATED_UNIVERSAL_TIME_OFFSET ( 0, 0, .AHEAD. ) ;
#32447 = EDGE_CURVE ( 'NONE', #1211, #16949, #3343, .T. ) ;
#32448 = CARTESIAN_POINT ( 'NONE',  ( 0.6554566019120018350, -1.532497645495064287, -0.6162739285286029656 ) ) ;
#32449 = CARTESIAN_POINT ( 'NONE',  ( 0.03303737228521357733, 0.3731855291841458810, 0.3634704002369245623 ) ) ;
#32450 = CARTESIAN_POINT ( 'NONE',  ( -0.1167294259372914089, -0.5331983348239582865, 0.3032895567580760066 ) ) ;
#32451 = CARTESIAN_POINT ( 'NONE',  ( 0.6960571170990073053, -1.427233132848869435, 0.5266323208858617599 ) ) ;
#32452 = CARTESIAN_POINT ( 'NONE',  ( 0.1548759089261000366, -1.279768374172243650, 0.4182417262808777458 ) ) ;
#32453 = CARTESIAN_POINT ( 'NONE',  ( 0.2565019309081923438, -1.535068652515254151, 0.9594965307338887417 ) ) ;
#32454 = CARTESIAN_POINT ( 'NONE',  ( 0.5807455352771149215, -1.554996163023655065, -0.4302623287978634692 ) ) ;
#32455 = CIRCLE ( 'NONE', #7457, 0.1762268159172233339 ) ;
#32456 = CARTESIAN_POINT ( 'NONE',  ( 0.02999999999997872077, -2.097675824466503691, -0.2588528740066097233 ) ) ;
#32457 = FACE_OUTER_BOUND ( 'NONE', #40196, .T. ) ;
#32458 = ORIENTED_EDGE ( 'NONE', *, *, #12667, .T. ) ;
#32459 = EDGE_LOOP ( 'NONE', ( #21862, #10207, #13792, #11327 ) ) ;
#32460 = CIRCLE ( 'NONE', #1635, 0.4614999999999880864 ) ;
#32461 = CARTESIAN_POINT ( 'NONE',  ( -0.2399999999999999079, -3.941790907013290823, -0.4709369376873030477 ) ) ;
#32462 = ORIENTED_EDGE ( 'NONE', *, *, #34633, .T. ) ;
#32463 = ORGANIZATION ( 'UNSPECIFIED', 'UNSPECIFIED', '' ) ;
#32464 = CARTESIAN_POINT ( 'NONE',  ( -0.01548846960707524721, 0.000000000000000000, 0.000000000000000000 ) ) ;
#32465 = CARTESIAN_POINT ( 'NONE',  ( 0.3574355869465279389, -1.729638559385621166, -0.4925610001298441065 ) ) ;
#32466 = CARTESIAN_POINT ( 'NONE',  ( 0.3808652519481688925, -1.119552471694881257, 0.7720269669908987886 ) ) ;
#32468 = ORIENTED_EDGE ( 'NONE', *, *, #25580, .T. ) ;
#32467 = DIRECTION ( 'NONE',  ( 0.8660512985181133550, 0.4999551463232371207, 0.000000000000000000 ) ) ;
#32469 = CARTESIAN_POINT ( 'NONE',  ( 0.5214254866212318928, -1.138125297403113523, 0.6686424646332703725 ) ) ;
#32470 = CARTESIAN_POINT ( 'NONE',  ( -0.05464101615137762630, -1.910390638264138685, -0.7420407338378623985 ) ) ;
#32471 = ORIENTED_EDGE ( 'NONE', *, *, #40125, .F. ) ;
#32472 = CARTESIAN_POINT ( 'NONE',  ( 0.5849095050029387011, -1.491341823319836335, -0.5960747874205124530 ) ) ;
#32473 = CONICAL_SURFACE ( 'NONE', #983, 0.1600000000000015854, 1.047197551196600518 ) ;
#32474 = CARTESIAN_POINT ( 'NONE',  ( 0.02324396854566065235, -0.5381434244155830493, 0.1953742764374014340 ) ) ;
#32476 = CARTESIAN_POINT ( 'NONE',  ( -0.04229956186878531393, -0.4429651807893734139, 0.1531492745855153881 ) ) ;
#32475 = CARTESIAN_POINT ( 'NONE',  ( 0.5308991136117184872, -1.672779244483038719, -0.4688114127759857030 ) ) ;
#32477 = CARTESIAN_POINT ( 'NONE',  ( 0.1438070510857625550, -1.283988175806205723, 0.3667417262808778111 ) ) ;
#32478 = B_SPLINE_CURVE_WITH_KNOTS ( 'NONE', 3,
 ( #503, #2059, #20587, #13784, #33121, #14593, #26952, #4929, #36620, #17678, #20186, #1682, #29631, #39099, #39486, #26352, #38878, #33507 ),
 .UNSPECIFIED., .F., .F.,
 ( 4, 2, 2, 2, 2, 2, 2, 2, 4 ),
 ( 0.0003425652276237360736, 0.001007165397454251772, 0.001671765567284767525, 0.002336365737115283711, 0.003000965906945799247, 0.003665566076776314783, 0.004330166246606831186, 0.004994766416437346722, 0.005659366586267862258 ),
 .UNSPECIFIED. ) ;
#32479 = CARTESIAN_POINT ( 'NONE',  ( 0.05387575222800708441, -1.597043685520700862, -0.3437276073321817726 ) ) ;
#32480 = ORIENTED_EDGE ( 'NONE', *, *, #23552, .T. ) ;
#32481 = CARTESIAN_POINT ( 'NONE',  ( -2.112273405726188513E-14, -2.183180860297921466, -0.2437760292030870524 ) ) ;
#32482 = CARTESIAN_POINT ( 'NONE',  ( 0.1852701303283973699, -0.8388891762519852247, 0.1468424033789395289 ) ) ;
#32483 = CARTESIAN_POINT ( 'NONE',  ( -0.02881329448201180518, -0.4517642754607882338, 0.2100174381954052760 ) ) ;
#32484 = CARTESIAN_POINT ( 'NONE',  ( -0.3000000000000000999, -2.342996121808762044, -0.6842569225768811991 ) ) ;
#32485 = CARTESIAN_POINT ( 'NONE',  ( 0.4352861832349482762, -1.225511609506093835, 0.6135475364930662590 ) ) ;
#32486 = CARTESIAN_POINT ( 'NONE',  ( 0.4810758011828559777, -1.682094021195914113, -0.6143846718455718836 ) ) ;
#32487 = AXIS2_PLACEMENT_3D ( 'NONE', #39964, #24948, #33999 ) ;
#32488 = CARTESIAN_POINT ( 'NONE',  ( 0.4615846830202947615, -1.152285184765094117, 0.4229742390834214660 ) ) ;
#32489 = AXIS2_PLACEMENT_3D ( 'NONE', #10482, #10303, #35384 ) ;
#32490 = CIRCLE ( 'NONE', #10839, 0.1600000000000015854 ) ;
#32491 = CARTESIAN_POINT ( 'NONE',  ( 0.4512927739169904640, -1.222232343183551784, 0.5547766907096001177 ) ) ;
#32492 = CARTESIAN_POINT ( 'NONE',  ( 0.6666052399636229753, -1.487988217786094136, 0.4225755393100666946 ) ) ;
#32493 = AXIS2_PLACEMENT_3D ( 'NONE', #36214, #8029, #33137 ) ;
#32494 = FACE_OUTER_BOUND ( 'NONE', #11126, .T. ) ;
#32495 = LINE ( 'NONE', #7386, #20072 ) ;
#32496 = CARTESIAN_POINT ( 'NONE',  ( 0.1316017208954911588, -1.248059642665102942, 0.5182417262812423209 ) ) ;
#32497 = LENGTH_MEASURE_WITH_UNIT ( LENGTH_MEASURE( 0.02539999999999999897 ), #23057 );
#32498 = APPLIED_SECURITY_CLASSIFICATION_ASSIGNMENT ( #17414, ( #26625 ) ) ;
#32499 = CARTESIAN_POINT ( 'NONE',  ( 0.003854562734146099994, -0.9635350917426001027, 0.4274684093136688623 ) ) ;
#32500 = EDGE_CURVE ( 'NONE', #26308, #9095, #796, .T. ) ;
#32501 = CARTESIAN_POINT ( 'NONE',  ( 0.1909286924077255310, -1.257064795538239022, -0.3824824602286830411 ) ) ;
#32502 = AXIS2_PLACEMENT_3D ( 'NONE', #14948, #18424, #12273 ) ;
#32503 = CARTESIAN_POINT ( 'NONE',  ( 0.1095009179483210360, -1.409958579616226393, 0.6174315292831226154 ) ) ;
#32504 = CARTESIAN_POINT ( 'NONE',  ( 0.01548846960721252282, 0.3688619771570336159, -0.3775276577325234473 ) ) ;
#32505 = CARTESIAN_POINT ( 'NONE',  ( 0.1886650716668294425, -1.684993351743720336, -0.6545385004037254095 ) ) ;
#32506 = ADVANCED_FACE ( 'NONE', ( #9852 ), #35169, .F. ) ;
#32507 = CARTESIAN_POINT ( 'NONE',  ( 0.2388732087844057106, -1.438419725007294314, 1.017786028862666559 ) ) ;
#32508 = DIRECTION ( 'NONE',  ( -0.8667346922030155776, -0.4987694591008393075, -3.159300867369172999E-12 ) ) ;
#32509 = EDGE_CURVE ( 'NONE', #14209, #4083, #3092, .T. ) ;
#32510 = ORIENTED_EDGE ( 'NONE', *, *, #216, .T. ) ;
#32511 = CARTESIAN_POINT ( 'NONE',  ( 0.1887384672550382336, -0.5142388724832238633, 0.08767850434337061405 ) ) ;
#32512 = ORIENTED_EDGE ( 'NONE', *, *, #33305, .F. ) ;
#32513 = FACE_OUTER_BOUND ( 'NONE', #2297, .T. ) ;
#32514 = AXIS2_PLACEMENT_3D ( 'NONE', #27488, #37146, #21930 ) ;
#32515 = CARTESIAN_POINT ( 'NONE',  ( 0.6019331370556211258, -1.483128407181113939, 0.5723791298540690242 ) ) ;
#32517 = ORIENTED_EDGE ( 'NONE', *, *, #40116, .T. ) ;
#32516 = CARTESIAN_POINT ( 'NONE',  ( 0.4989284167723000429, -1.653128005833214065, -0.4311520333451080433 ) ) ;
#32518 = VECTOR ( 'NONE', #34012, 39.37007874015748854 ) ;
#32520 = VERTEX_POINT ( 'NONE', #6760 ) ;
#32519 = ORIENTED_EDGE ( 'NONE', *, *, #887, .T. ) ;
#32521 = CARTESIAN_POINT ( 'NONE',  ( 0.3938429588588502339, -1.036934036128653647, 0.8714819481111626409 ) ) ;
#32522 = AXIS2_PLACEMENT_3D ( 'NONE', #25402, #22926, #13233 ) ;
#32523 = ORIENTED_EDGE ( 'NONE', *, *, #23061, .F. ) ;
#32524 = ADVANCED_FACE ( 'NONE', ( #25507 ), #24510, .F. ) ;
#32525 = CARTESIAN_POINT ( 'NONE',  ( 0.2059273467974228888, -1.283046334493782803, -0.6702542665264737964 ) ) ;
#32526 = CARTESIAN_POINT ( 'NONE',  ( 0.5237801217064862458, -1.180371363492203285, -0.6194292131661300882 ) ) ;
#32527 = LOCAL_TIME ( 0, 53, 7.000000000000000000, #20023 ) ;
#32528 = APPLIED_DATE_AND_TIME_ASSIGNMENT ( #22265, #25543, ( #8373 ) ) ;
#32529 = CARTESIAN_POINT ( 'NONE',  ( 0.6223120740387964034, -1.620008259572149445, -0.4840127556439880463 ) ) ;
#32530 = CARTESIAN_POINT ( 'NONE',  ( 0.0002183020222796143764, -0.9534082139883228724, 0.09509064842809067386 ) ) ;
#32532 = ORIENTED_EDGE ( 'NONE', *, *, #8667, .F. ) ;
#32531 = ORIENTED_EDGE ( 'NONE', *, *, #17074, .T. ) ;
#32533 = CARTESIAN_POINT ( 'NONE',  ( 0.08636792212753842402, -0.7903263359433837509, 0.2049882209949519252 ) ) ;
#32534 = AXIS2_PLACEMENT_3D ( 'NONE', #1081, #28818, #10911 ) ;
#32535 = CARTESIAN_POINT ( 'NONE',  ( 0.09291248155910060424, -0.5915724845055667647, 0.2542574423113423965 ) ) ;
#32536 = CARTESIAN_POINT ( 'NONE',  ( 0.5389492827143899101, -1.519008290879962697, 0.5707740500833556885 ) ) ;
#32537 = ORIENTED_EDGE ( 'NONE', *, *, #39802, .F. ) ;
#32538 = CARTESIAN_POINT ( 'NONE',  ( 0.05894831851802598277, -1.250166165718733291, 0.6518816580813121542 ) ) ;
#32539 = CARTESIAN_POINT ( 'NONE',  ( 0.1759300380180282841, -1.231083256582695906, -0.6184399470714002645 ) ) ;
#32540 = FACE_OUTER_BOUND ( 'NONE', #15365, .T. ) ;
#32541 = CARTESIAN_POINT ( 'NONE',  ( 0.3084565412903440551, -1.760887085980910483, 0.5691548551326652827 ) ) ;
#32542 = CARTESIAN_POINT ( 'NONE',  ( 0.7429086483856627288, -1.516424694377827898, 0.5595610635296612845 ) ) ;
#32543 = CARTESIAN_POINT ( 'NONE',  ( 0.06936654275856572738, -1.327133429011284393, 0.5458395137742207970 ) ) ;
#32544 = DIRECTION ( 'NONE',  ( -1.000000000000000000, -0.000000000000000000, -0.000000000000000000 ) ) ;
#32545 = CARTESIAN_POINT ( 'NONE',  ( 0.3999999999999798161, -2.166079853131637645, -0.4467913981637911536 ) ) ;
#32546 = CARTESIAN_POINT ( 'NONE',  ( 0.01153255118075396934, -0.8600574543152128548, -0.04784606081928678006 ) ) ;
#32547 = CARTESIAN_POINT ( 'NONE',  ( 0.5388299548087387425, -1.396690896044502139, 0.7799327982793118341 ) ) ;
#32548 =( NAMED_UNIT ( * ) PLANE_ANGLE_UNIT ( ) SI_UNIT ( $, .RADIAN. ) );
#32549 = CARTESIAN_POINT ( 'NONE',  ( 0.4970273525888077026, -1.079783658718535877, 0.3157417262808778213 ) ) ;
#32550 = B_SPLINE_CURVE_WITH_KNOTS ( 'NONE', 3,
 ( #27538, #33919, #11885, #18465 ),
 .UNSPECIFIED., .F., .F.,
 ( 4, 4 ),
 ( 7.949501638480626889E-18, 0.0004616409723689751383 ),
 .UNSPECIFIED. ) ;
#32551 = CIRCLE ( 'NONE', #26003, 0.01499999999999999424 ) ;
#32552 = CARTESIAN_POINT ( 'NONE',  ( -0.05464101615137763324, -2.183180860297908144, -0.4937760292030871079 ) ) ;
#32553 = ADVANCED_FACE ( 'NONE', ( #12041 ), #31934, .F. ) ;
#32554 = CARTESIAN_POINT ( 'NONE',  ( -0.003124719664520040317, -0.8057675726412020234, 0.1293934913668264852 ) ) ;
#32555 = B_SPLINE_CURVE_WITH_KNOTS ( 'NONE', 3,
 ( #10637, #7547, #7753, #26704, #7942, #23817, #23617, #20319, #20517, #8156 ),
 .UNSPECIFIED., .F., .F.,
 ( 4, 2, 2, 2, 4 ),
 ( 7.269816092100765919E-18, 0.0003553525228749304958, 0.0007107050457498537274, 0.001066057568624777067, 0.001421410091499700299 ),
 .UNSPECIFIED. ) ;
#32556 = CARTESIAN_POINT ( 'NONE',  ( 0.4473065160884135416, -1.054428903401835704, 0.6531518022732211159 ) ) ;
#32557 = EDGE_CURVE ( 'NONE', #24814, #38935, #25767, .T. ) ;
#32558 = APPROVAL_ROLE ( '' ) ;
#32559 = LOCAL_TIME ( 0, 53, 7.000000000000000000, #9401 ) ;
#32560 = EDGE_CURVE ( 'NONE', #17501, #22855, #32838, .T. ) ;
#32561 = DIRECTION ( 'NONE',  ( 0.000000000000000000, 0.000000000000000000, -1.000000000000000000 ) ) ;
#32562 = ADVANCED_FACE ( 'NONE', ( #38290 ), #16491, .T. ) ;
#32563 = AXIS2_PLACEMENT_3D ( 'NONE', #12940, #16834, #25488 ) ;
#32564 = DIRECTION ( 'NONE',  ( 1.000000000000000000, 0.000000000000000000, 1.517693329813469311E-15 ) ) ;
#32565 = ORIENTED_EDGE ( 'NONE', *, *, #4694, .F. ) ;
#32566 = CARTESIAN_POINT ( 'NONE',  ( 0.2117601568378603694, -1.293150266309827101, -0.7462941026102624109 ) ) ;
#32567 = CARTESIAN_POINT ( 'NONE',  ( 0.01056005445531711488, -0.5296673602274948323, 0.1478910490635437502 ) ) ;
#32568 = CARTESIAN_POINT ( 'NONE',  ( 0.1736343712300759123, -1.255284373594809155, 0.4365611478178134663 ) ) ;
#32569 = ORIENTED_EDGE ( 'NONE', *, *, #8878, .T. ) ;
#32570 = CARTESIAN_POINT ( 'NONE',  ( -0.2600000000000003419, 0.5182417262804733804, 0.3749999999999999445 ) ) ;
#32571 = CARTESIAN_POINT ( 'NONE',  ( 0.5016144086874707586, -1.117686766064061255, 0.8075564334577929326 ) ) ;
#32573 = ORIENTED_EDGE ( 'NONE', *, *, #1554, .T. ) ;
#32572 = ORIENTED_EDGE ( 'NONE', *, *, #24981, .T. ) ;
#32574 = CARTESIAN_POINT ( 'NONE',  ( -2.120170153832874165E-14, -2.097675824466503691, -0.6968677163258657492 ) ) ;
#32575 = ORIENTED_EDGE ( 'NONE', *, *, #3993, .F. ) ;
#32576 = CARTESIAN_POINT ( 'NONE',  ( 0.3560973459019345921, -1.892274349130671274, -0.5076868541395752610 ) ) ;
#32577 = EDGE_CURVE ( 'NONE', #24493, #20049, #2423, .T. ) ;
#32578 = CARTESIAN_POINT ( 'NONE',  ( 0.4434829238260091233, -1.227582997348585447, 0.5913743549708686542 ) ) ;
#32579 = CLOSED_SHELL ( 'NONE', ( #17521, #22345, #39848, #33466, #6475, #40084, #5414, #8973, #17102, #16248, #21105, #9259, #7201, #10766, #8994, #19982, #25526, #40385, #7619, #39188, #37961, #1732, #25030, #2753, #13701, #27091, #8694, #22136, #15925, #20727, #24781, #13188, #24039, #28116, #33270, #23366, #4179, #1360, #9937 ) ) ;
#32580 = CARTESIAN_POINT ( 'NONE',  ( -0.04308449196698830447, 0.4845747790794809329, -0.09763455429601648750 ) ) ;
#32581 = ORIENTED_EDGE ( 'NONE', *, *, #24513, .T. ) ;
#32582 = CARTESIAN_POINT ( 'NONE',  ( 0.1718750000000003608, -0.4565580874172215364, 0.1457185332388697130 ) ) ;
#32583 = CARTESIAN_POINT ( 'NONE',  ( 0.1108361821491160165, -0.7252665196136722781, 0.3985623511072731717 ) ) ;
#32584 = B_SPLINE_CURVE_WITH_KNOTS ( 'NONE', 3,
 ( #2959, #323, #18804, #37491, #18998, #9312, #35024, #21678, #16322, #34816 ),
 .UNSPECIFIED., .F., .F.,
 ( 4, 2, 2, 2, 4 ),
 ( 0.0002266766535735069562, 0.0007552434839518312520, 0.001283810314330155683, 0.001812377144708480006, 0.002340943975086804112 ),
 .UNSPECIFIED. ) ;
#32585 = CARTESIAN_POINT ( 'NONE',  ( 0.1162424483802486364, -0.9470763074633095080, 0.9119154921836929439 ) ) ;
#32586 = CARTESIAN_POINT ( 'NONE',  ( 0.08646685978301947573, -0.5613322375003841902, 0.2349906393216993905 ) ) ;
#32588 = CARTESIAN_POINT ( 'NONE',  ( 0.3172206172883819120, -1.646250959826369709, 0.6002829085295777745 ) ) ;
#32587 = CARTESIAN_POINT ( 'NONE',  ( 0.1787384279610586268, -1.322427451166070300, 0.9491502850971088590 ) ) ;
#32589 = CARTESIAN_POINT ( 'NONE',  ( 0.04687500000000023592, -0.9399235171994245741, 0.1623004675701537336 ) ) ;
#32590 = LOCAL_TIME ( 0, 53, 7.000000000000000000, #29141 ) ;
#32591 = ORIENTED_EDGE ( 'NONE', *, *, #6908, .F. ) ;
#32592 = VERTEX_POINT ( 'NONE', #37518 ) ;
#32593 = CARTESIAN_POINT ( 'NONE',  ( 0.6593903862521710568, -1.512843973183619850, -0.6186210669918369431 ) ) ;
#32594 = B_SPLINE_CURVE_WITH_KNOTS ( 'NONE', 3,
 ( #3846, #3451, #618, #38612, #13713, #25673, #22993, #38208, #10030, #32433, #35134, #6935, #808, #13316 ),
 .UNSPECIFIED., .F., .F.,
 ( 4, 2, 2, 2, 2, 2, 4 ),
 ( 0.001790297533228681851, 0.002478079898554628058, 0.003165862263880574699, 0.004541426994532467981, 0.005916991725184360396, 0.006604774090510308338, 0.007292556455836254545 ),
 .UNSPECIFIED. ) ;
#32595 = CARTESIAN_POINT ( 'NONE',  ( 0.2498664206433944546, -0.6480277882228060449, 0.5700154607156771025 ) ) ;
#32596 = CIRCLE ( 'NONE', #1772, 0.03000000000000000583 ) ;
#32597 = CARTESIAN_POINT ( 'NONE',  ( -0.05491348488830476854, 0.2511509903618529549, -0.3886212643843935943 ) ) ;
#32598 = CARTESIAN_POINT ( 'NONE',  ( -0.05252049209742622876, -0.4432254733698156590, -0.1535896008539242019 ) ) ;
#32599 = CARTESIAN_POINT ( 'NONE',  ( -0.01548846960707504251, -0.09319974324248665731, 0.5318964258758798191 ) ) ;
#32600 = CARTESIAN_POINT ( 'NONE',  ( 0.4065730081747980229, -1.089323883707587370, 0.5182417262812423209 ) ) ;
#32601 = CARTESIAN_POINT ( 'NONE',  ( 0.4594195809631357874, -1.060066247262113182, 0.7450334795338161564 ) ) ;
#32602 = ADVANCED_FACE ( 'NONE', ( #9140 ), #19397, .T. ) ;
#32603 = DIRECTION ( 'NONE',  ( 0.000000000000000000, 0.000000000000000000, -1.000000000000000000 ) ) ;
#32604 = CARTESIAN_POINT ( 'NONE',  ( 0.0004377143710694352875, -0.8614844325866355401, 0.3723279202124662457 ) ) ;
#32605 = EDGE_CURVE ( 'NONE', #9809, #23695, #8778, .T. ) ;
#32606 = AXIS2_PLACEMENT_3D ( 'NONE', #27949, #27348, #8807 ) ;
#32607 = CARTESIAN_POINT ( 'NONE',  ( 0.5503547679451166186, -1.661547860700446799, -0.5401600205605633365 ) ) ;
#32608 = ORIENTED_EDGE ( 'NONE', *, *, #32098, .F. ) ;
#32609 = CARTESIAN_POINT ( 'NONE',  ( 0.2994521289839266465, -1.048896011437137510, 0.7355833716002573297 ) ) ;
#32610 = FACE_OUTER_BOUND ( 'NONE', #40407, .T. ) ;
#32611 = EDGE_CURVE ( 'NONE', #32971, #25148, #12080, .T. ) ;
#32612 = CARTESIAN_POINT ( 'NONE',  ( -0.04760454375021574980, -0.2475296122118676723, -0.4138634427292607887 ) ) ;
#32613 = ORGANIZATION ( 'NAUO-ORG15', 'UNSPECIFIED', 'UNSPECIFIED' ) ;
#32614 = ORIENTED_EDGE ( 'NONE', *, *, #32004, .T. ) ;
#32615 = CARTESIAN_POINT ( 'NONE',  ( 0.2059273467974226113, -1.283046334493782359, -0.7137159211901564770 ) ) ;
#32616 = ORIENTED_EDGE ( 'NONE', *, *, #22000, .T. ) ;
#32617 = CARTESIAN_POINT ( 'NONE',  ( 0.4974456442574050619, -1.184401136727558868, 0.4224083929475309640 ) ) ;
#32618 = CARTESIAN_POINT ( 'NONE',  ( 0.3585037315287261661, -1.733294065422876784, -0.4968629709071194500 ) ) ;
#32619 = FACE_OUTER_BOUND ( 'NONE', #18068, .T. ) ;
#32620 = AXIS2_PLACEMENT_3D ( 'NONE', #33250, #23809, #1810 ) ;
#32621 = CARTESIAN_POINT ( 'NONE',  ( 0.2791220714032660588, -1.321220139306267694, 0.5799651797159807165 ) ) ;
#32622 = ORIENTED_EDGE ( 'NONE', *, *, #488, .T. ) ;
#32623 = CARTESIAN_POINT ( 'NONE',  ( -0.1642263571684461076, 0.5103503754387049840, 0.3032895567580806140 ) ) ;
#32624 = EDGE_CURVE ( 'NONE', #20049, #22416, #13179, .T. ) ;
#32625 = CARTESIAN_POINT ( 'NONE',  ( 0.6530643362242376515, -1.539305493024291094, -0.4161285573133042814 ) ) ;
#32626 = CARTESIAN_POINT ( 'NONE',  ( 0.1252902061131786204, -1.410433472168242552, 0.4751538658811860216 ) ) ;
#32627 = EDGE_CURVE ( 'NONE', #34235, #24591, #4824, .T. ) ;
#32628 = DIRECTION ( 'NONE',  ( 0.5000000000000009992, -0.7308273574226400449, -0.4646411234949396341 ) ) ;
#32629 = CARTESIAN_POINT ( 'NONE',  ( 0.3636433330243779016, -1.102202853961738782, 0.7268133992109953034 ) ) ;
#32631 = CARTESIAN_POINT ( 'NONE',  ( 0.3229289876128840775, -1.169687821100875658, 0.5631135379446852163 ) ) ;
#32630 = DIRECTION ( 'NONE',  ( -0.4999551463232377313, 0.8660512985181132439, -0.000000000000000000 ) ) ;
#32632 = CARTESIAN_POINT ( 'NONE',  ( 0.1947294528115406376, -0.9190940877486376559, 0.2754987677893815934 ) ) ;
#32633 = ORIENTED_EDGE ( 'NONE', *, *, #12329, .F. ) ;
#32634 = EDGE_CURVE ( 'NONE', #23647, #34438, #7211, .T. ) ;
#32635 = CARTESIAN_POINT ( 'NONE',  ( 0.4368279861777725204, -1.677667223885754844, 0.4182417262808776903 ) ) ;
#32636 = VERTEX_POINT ( 'NONE', #34239 ) ;
#32637 = EDGE_CURVE ( 'NONE', #3269, #35263, #19951, .T. ) ;
#32638 = CARTESIAN_POINT ( 'NONE',  ( 0.4141285076484039207, -1.589661339031622322, 0.5810052816111468399 ) ) ;
#32640 = CARTESIAN_POINT ( 'NONE',  ( 0.1949235715289977799, -0.7262771972565351675, 0.3260392721664385762 ) ) ;
#32639 = CARTESIAN_POINT ( 'NONE',  ( 0.06694291677841214538, -0.6774102696622015252, -0.001900350697965435751 ) ) ;
#32641 = DIRECTION ( 'NONE',  ( 1.000000000000000000, 1.131052719138050089E-31, -7.771561172376107616E-16 ) ) ;
#32642 = EDGE_LOOP ( 'NONE', ( #18579, #40570, #11233, #32161 ) ) ;
#32643 = ORIENTED_EDGE ( 'NONE', *, *, #32509, .T. ) ;
#32644 = AXIS2_PLACEMENT_3D ( 'NONE', #22511, #31960, #22923 ) ;
#32645 = CARTESIAN_POINT ( 'NONE',  ( 0.5602801778932028354, -1.505597814391692824, 0.5212860325390119565 ) ) ;
#32646 = CARTESIAN_POINT ( 'NONE',  ( 0.1192883206712807842, -0.5593364352323437760, 0.2090905374237496672 ) ) ;
#32647 = ORIENTED_EDGE ( 'NONE', *, *, #25092, .T. ) ;
#32648 = DIRECTION ( 'NONE',  ( -1.000000000000000000, 0.000000000000000000, 0.000000000000000000 ) ) ;
#32649 = CARTESIAN_POINT ( 'NONE',  ( 0.3984114568195522010, -1.599003643269838904, -0.5155029497116575543 ) ) ;
#32650 = CARTESIAN_POINT ( 'NONE',  ( 0.4111143676683018389, -1.741928728223572920, -0.4339933128339369950 ) ) ;
#32651 = CARTESIAN_POINT ( 'NONE',  ( 0.2211874525952635950, -1.239324575930034644, 0.4870531881579039934 ) ) ;
#32652 = CARTESIAN_POINT ( 'NONE',  ( 0.3265224326933078847, -1.121055775672392452, -0.5155029497116575543 ) ) ;
#32653 = CARTESIAN_POINT ( 'NONE',  ( -0.05464101615137770263, -2.183180860297908144, -0.3317586832283064280 ) ) ;
#32654 = CARTESIAN_POINT ( 'NONE',  ( 0.4045891740076953402, -0.9484829520717948936, 0.8148132024759134895 ) ) ;
#32655 = CARTESIAN_POINT ( 'NONE',  ( -0.05464101615137768181, -2.367354784411275670, -0.3586747285825516718 ) ) ;
#32656 = CARTESIAN_POINT ( 'NONE',  ( 0.04155248107635917121, -0.2623121065566118570, -0.3903559784317167658 ) ) ;
#32657 = APPLICATION_PROTOCOL_DEFINITION ( 'international standard', 'automotive_design', 2000, #3232 ) ;
#32658 = ADVANCED_FACE ( 'NONE', ( #6049 ), #22695, .F. ) ;
#32659 = CARTESIAN_POINT ( 'NONE',  ( 0.6596696466511408063, -1.414650502503907559, -0.6114726203884881528 ) ) ;
#32660 = CARTESIAN_POINT ( 'NONE',  ( 0.02238826743733428673, 0.3549908576167664087, 0.3695531484129505051 ) ) ;
#32661 = CARTESIAN_POINT ( 'NONE',  ( 0.1845448093765023889, -0.6265762398594633131, -0.02094390412501702034 ) ) ;
#32662 = EDGE_CURVE ( 'NONE', #10881, #6598, #11428, .T. ) ;
#32663 = FACE_OUTER_BOUND ( 'NONE', #34645, .T. ) ;
#32664 = CARTESIAN_POINT ( 'NONE',  ( 0.1255475574219608592, -1.293490214176332254, 0.4290848500164155532 ) ) ;
#32665 = CARTESIAN_POINT ( 'NONE',  ( 0.0003293075040918708759, -0.6974492147978401668, 0.2474296275395909961 ) ) ;
#32666 = CARTESIAN_POINT ( 'NONE',  ( 0.5859173466656659723, -1.569541677886773012, -0.5263893777432389065 ) ) ;
#32667 = CARTESIAN_POINT ( 'NONE',  ( 0.4806378395295556882, -1.105637800341302102, -0.6194292131661300882 ) ) ;
#32668 = CARTESIAN_POINT ( 'NONE',  ( 0.3048238845683336473, -1.756859000771363366, 0.5688729523718247805 ) ) ;
#32669 = CARTESIAN_POINT ( 'NONE',  ( -0.04140212552917707511, -0.2627138686861280048, 0.3904233130033950561 ) ) ;
#32670 =( REPRESENTATION_RELATIONSHIP ('NONE','NONE', #27514, #8026 ) REPRESENTATION_RELATIONSHIP_WITH_TRANSFORMATION ( #14266 )SHAPE_REPRESENTATION_RELATIONSHIP( ) );
#32671 = ORIENTED_EDGE ( 'NONE', *, *, #32041, .F. ) ;
#32672 = ORIENTED_EDGE ( 'NONE', *, *, #28525, .F. ) ;
#32673 =( BOUNDED_SURFACE ( )  B_SPLINE_SURFACE ( 3, 2, ( 
 ( #3214, #27711, #2616 ),
 ( #6301, #15154, #40245 ),
 ( #12082, #36962, #9597 ),
 ( #15974, #37176, #21744 ),
 ( #27923, #40040, #24643 ),
 ( #34687, #11863, #30993 ) ),
 .UNSPECIFIED., .F., .F., .F. ) 
 B_SPLINE_SURFACE_WITH_KNOTS ( ( 4, 2, 4 ),
 ( 3, 3 ),
 ( -2.108773225484306124E-17, 0.0002308790202334583513, 0.0004617580404669377903 ),
 ( 0.000000000000000000, 1.000000000000000000 ),
 .UNSPECIFIED. ) 
 GEOMETRIC_REPRESENTATION_ITEM ( )  RATIONAL_B_SPLINE_SURFACE ( (
 ( 1.000000000000000000, 0.9183064432839348479, 1.000000000000000000),
 ( 1.000000000000000000, 0.9259132747140148556, 1.000000000000000000),
 ( 1.000000000000000000, 0.9308516525543161224, 1.000000000000000000),
 ( 1.000000000000000000, 0.9333900639176514469, 1.000000000000000000),
 ( 1.000000000000000000, 0.9310108186281401688, 1.000000000000000000),
 ( 1.000000000000000000, 0.9252764552858380176, 1.000000000000000000) ) ) 
 REPRESENTATION_ITEM ( '' )  SURFACE ( )  );
#32674 = CARTESIAN_POINT ( 'NONE',  ( 0.4971920908461615607, -1.080069027881642052, 0.4687417262808780127 ) ) ;
#32675 = EDGE_LOOP ( 'NONE', ( #17261, #14002, #15883, #2480, #5137 ) ) ;
#32676 = CARTESIAN_POINT ( 'NONE',  ( 0.4887921365776448090, -1.679766821171225999, -0.4193976862638449377 ) ) ;
#32677 = CARTESIAN_POINT ( 'NONE',  ( 0.6952357793749982529, -1.543270793921424744, 0.4282417262808777547 ) ) ;
#32678 = CARTESIAN_POINT ( 'NONE',  ( 0.5497128959811709015, -1.376878964193947397, 0.6508683836033526404 ) ) ;
#32680 = VERTEX_POINT ( 'NONE', #19776 ) ;
#32679 = DIRECTION ( 'NONE',  ( -2.276539994720217574E-15, 1.000000000000000000, -2.162712994984206616E-14 ) ) ;
#32681 = CARTESIAN_POINT ( 'NONE',  ( 0.3071794164948500327, -0.9095699098325729093, 0.5987596725107463547 ) ) ;
#32682 = AXIS2_PLACEMENT_3D ( 'NONE', #5956, #31287, #12545 ) ;
#32683 = DIRECTION ( 'NONE',  ( 8.881784197001246407E-16, -2.361472542561082612E-16, 1.000000000000000000 ) ) ;
#32684 = EDGE_LOOP ( 'NONE', ( #5094, #21463, #40228, #34151 ) ) ;
#32685 = CARTESIAN_POINT ( 'NONE',  ( 0.4572526883583915014, -1.685933642108535357, -0.4119903234399788228 ) ) ;
#32686 = EDGE_LOOP ( 'NONE', ( #23351, #9907, #13835, #9954 ) ) ;
#32687 = CARTESIAN_POINT ( 'NONE',  ( 0.02886328582901781167, -0.5951803392457304387, 0.3522513419751048258 ) ) ;
#32689 = CARTESIAN_POINT ( 'NONE',  ( 0.1112482850659993472, -0.9162505102043612126, 0.06796212585817107410 ) ) ;
#32688 = CARTESIAN_POINT ( 'NONE',  ( 0.6892485586469115910, -1.501120256590844360, 0.4658724615422447646 ) ) ;
#32690 = CYLINDRICAL_SURFACE ( 'NONE', #26706, 0.5756329413417603513 ) ;
#32691 = CARTESIAN_POINT ( 'NONE',  ( 0.1317419978059748698, -1.353679905699192831, -0.3213817580603143265 ) ) ;
#32692 = EDGE_LOOP ( 'NONE', ( #36767, #566, #36517, #34808 ) ) ;
#32693 = DIRECTION ( 'NONE',  ( 0.000000000000000000, 0.000000000000000000, -1.000000000000000000 ) ) ;
#32694 = CARTESIAN_POINT ( 'NONE',  ( 0.1586721817899592324, -1.274732504449104242, 0.4246823382044858097 ) ) ;
#32695 = DIRECTION ( 'NONE',  ( 0.000000000000000000, 0.000000000000000000, -1.000000000000000000 ) ) ;
#32696 = CARTESIAN_POINT ( 'NONE',  ( 0.4388835414683294744, -1.230108148053269401, 0.5775320749789016883 ) ) ;
#32697 = CARTESIAN_POINT ( 'NONE',  ( 0.5980972052530336702, -1.476321197844801647, 0.6100096754393737886 ) ) ;
#32698 = CARTESIAN_POINT ( 'NONE',  ( 0.4719477840738105501, -1.167887988919352749, 0.4182417262808778013 ) ) ;
#32699 = DIRECTION ( 'NONE',  ( -1.000000000000000000, -0.000000000000000000, -0.000000000000000000 ) ) ;
#32700 = CARTESIAN_POINT ( 'NONE',  ( 0.6605589060724770256, -1.466964374737534937, 0.4224021371703464145 ) ) ;
#32701 = FACE_OUTER_BOUND ( 'NONE', #26212, .T. ) ;
#32702 = CARTESIAN_POINT ( 'NONE',  ( 0.3183193540680943623, -1.763265185351239106, 0.5161083673949912187 ) ) ;
#32703 = DIRECTION ( 'NONE',  ( 0.8660512985181129109, 0.4999551463232381199, 0.000000000000000000 ) ) ;
#32704 = CALENDAR_DATE ( 2026, 13, 10 ) ;
#32705 = CARTESIAN_POINT ( 'NONE',  ( 0.04291294112961202556, -1.197002576549752284, 0.6781355655905598745 ) ) ;
#32706 = CARTESIAN_POINT ( 'NONE',  ( 0.1802568680720616767, -0.4967246651221558507, 0.1220688697886482543 ) ) ;
#32707 = PRODUCT_DEFINITION_CONTEXT ( 'detailed design', #30042, 'design' ) ;
#32708 = DIRECTION ( 'NONE',  ( 5.551115123125799958E-17, -4.553079989440443628E-16, -1.000000000000000000 ) ) ;
#32709 = DIRECTION ( 'NONE',  ( 1.000000000000000000, 0.000000000000000000, 0.000000000000000000 ) ) ;
#32710 = DIRECTION ( 'NONE',  ( -1.000000000000000000, -2.280301054154495132E-31, 1.664003471950577689E-31 ) ) ;
#32711 = CARTESIAN_POINT ( 'NONE',  ( 0.2035125522712091239, -1.312695684735130097, 1.024845729304089126 ) ) ;
#32712 = DIRECTION ( 'NONE',  ( 0.000000000000000000, 0.000000000000000000, -1.000000000000000000 ) ) ;
#32713 = ORIENTED_EDGE ( 'NONE', *, *, #19299, .F. ) ;
#32714 = ORIENTED_EDGE ( 'NONE', *, *, #5418, .T. ) ;
#32715 = CARTESIAN_POINT ( 'NONE',  ( 0.1755442188764480826, -0.5359865673549585319, 0.2258108374879264080 ) ) ;
#32716 = ORIENTED_EDGE ( 'NONE', *, *, #1875, .T. ) ;
#32717 = CARTESIAN_POINT ( 'NONE',  ( 0.2059273467974226113, -1.283046334493782803, -0.3194715457588298557 ) ) ;
#32718 = CARTESIAN_POINT ( 'NONE',  ( 0.6023664826634441694, -1.483121557002085478, 0.5812678940365340052 ) ) ;
#32720 = VERTEX_POINT ( 'NONE', #32315 ) ;
#32719 = CARTESIAN_POINT ( 'NONE',  ( -0.001119162526905346329, -0.7995298731302591388, 0.02018642203061219928 ) ) ;
#32722 = ORIENTED_EDGE ( 'NONE', *, *, #9934, .T. ) ;
#32721 = ORIENTED_EDGE ( 'NONE', *, *, #12922, .T. ) ;
#32723 = CARTESIAN_POINT ( 'NONE',  ( 0.1689060685570120401, -0.6335038543973973146, 0.5777283047956938145 ) ) ;
#32724 = VERTEX_POINT ( 'NONE', #15113 ) ;
#32725 = CARTESIAN_POINT ( 'NONE',  ( -0.01296308306156608581, -0.5559130093646982296, 0.2739470918511063280 ) ) ;
#32727 = CARTESIAN_POINT ( 'NONE',  ( -0.2399999999999999079, -1.906460133321048911, -0.3231213194042101278 ) ) ;
#32726 = CARTESIAN_POINT ( 'NONE',  ( 0.03478556507499377948, 0.4639967941987065969, 0.2267627654641998503 ) ) ;
#32728 = DIRECTION ( 'NONE',  ( 5.551115123125868984E-17, -5.531779426422974156E-16, -1.000000000000000000 ) ) ;
#32729 = APPROVAL_ROLE ( '' ) ;
#32730 = DIRECTION ( 'NONE',  ( -0.8660512985181135770, -0.4999551463232371207, 0.000000000000000000 ) ) ;
#32732 = ORIENTED_EDGE ( 'NONE', *, *, #8003, .T. ) ;
#32731 = EDGE_LOOP ( 'NONE', ( #22681, #28427, #21808, #5388 ) ) ;
#32733 = CARTESIAN_POINT ( 'NONE',  ( 0.08507626058706437011, -0.7891241300377983547, 0.1457185332388674370 ) ) ;
#32734 = AXIS2_PLACEMENT_3D ( 'NONE', #7586, #1254, #22858 ) ;
#32735 = CARTESIAN_POINT ( 'NONE',  ( 0.09571612354954127377, -1.278066085047872669, 0.7427547889169190398 ) ) ;
#32736 = CARTESIAN_POINT ( 'NONE',  ( 0.07229973480053927815, -0.5685354101550715855, 0.2638894623840417064 ) ) ;
#32737 = CARTESIAN_POINT ( 'NONE',  ( 0.5391388180847991318, -1.519055229545304586, 0.5740328089454040938 ) ) ;
#32738 = CARTESIAN_POINT ( 'NONE',  ( 0.1931892079297521658, -0.5558303771799478765, 0.2996417238165024477 ) ) ;
#32739 = CARTESIAN_POINT ( 'NONE',  ( 0.5974135625431907792, -1.483567655257939544, 0.6235288986217942808 ) ) ;
#32740 = CARTESIAN_POINT ( 'NONE',  ( 0.6808109290445034656, -1.529880038401493447, 0.4663894423524581057 ) ) ;
#32741 = CARTESIAN_POINT ( 'NONE',  ( 0.3904547891981581254, -1.730724516036661331, 0.6095245837950131751 ) ) ;
#32742 = CARTESIAN_POINT ( 'NONE',  ( -0.1399999999999997358, 0.000000000000000000, 0.000000000000000000 ) ) ;
#32743 = CARTESIAN_POINT ( 'NONE',  ( 0.4815782007885943128, -1.590841155114501193, -0.5855112036560438105 ) ) ;
#32744 = CARTESIAN_POINT ( 'NONE',  ( -0.3000000000000000999, -3.758594918004649621, -0.06617323996463200797 ) ) ;
#32745 = CARTESIAN_POINT ( 'NONE',  ( 0.01548846960707497486, -0.2372406987223574237, 0.4850946823762633531 ) ) ;
#32746 = CARTESIAN_POINT ( 'NONE',  ( -1.332134553831062102E-05, -0.8481898185222114250, -0.06042459179974628974 ) ) ;
#32747 = CARTESIAN_POINT ( 'NONE',  ( 0.06931620475622646271, -0.5411911513605178747, 0.1654370273737149066 ) ) ;
#32748 = SHAPE_REPRESENTATION_RELATIONSHIP ( 'NONE' , 'NONE' ,  #30390, #16697 ) ;
#32749 = CARTESIAN_POINT ( 'NONE',  ( -0.2746410161513776482, -3.941790907013290823, -0.2762780017083287243 ) ) ;
#32750 = LINE ( 'NONE', #1515, #17935 ) ;
#32751 = CARTESIAN_POINT ( 'NONE',  ( -0.001163483333746527255, -0.8281092574587937127, 0.3345003353200291518 ) ) ;
#32752 = CARTESIAN_POINT ( 'NONE',  ( 0.4130926557567901058, -1.028576094973266963, 0.6508837067575374835 ) ) ;
#32753 = PERSON_AND_ORGANIZATION_ROLE ( 'classification_officer' ) ;
#32754 = CARTESIAN_POINT ( 'NONE',  ( 0.2622253439111549289, -0.6837502657356347990, 0.6133988000875116864 ) ) ;
#32755 = EDGE_CURVE ( 'NONE', #9503, #1137, #24572, .T. ) ;
#32756 = APPROVAL ( #33579, 'UNKNOWN' ) ;
#32757 = DIRECTION ( 'NONE',  ( 0.8660512985181134660, 0.4999551463232371762, 0.000000000000000000 ) ) ;
#32758 = CARTESIAN_POINT ( 'NONE',  ( 0.3048535705585853073, -1.756846727098643868, 0.5694515197924591154 ) ) ;
#32759 = EDGE_LOOP ( 'NONE', ( #39494, #31430, #13252, #30761 ) ) ;
#32760 = CARTESIAN_POINT ( 'NONE',  ( 0.3389453752120347718, -1.642550427334032337, -0.5887789075332919841 ) ) ;
#32761 = CARTESIAN_POINT ( 'NONE',  ( 0.01243718341181578382, -0.5782126198877061141, 0.3200173145254873730 ) ) ;
#32762 = DIRECTION ( 'NONE',  ( -0.8660254037844402619, 0.4079706259167340532, 0.2890674114961865326 ) ) ;
#32763 = ORIENTED_EDGE ( 'NONE', *, *, #14285, .F. ) ;
#32764 = DIRECTION ( 'NONE',  ( 0.000000000000000000, 0.000000000000000000, -1.000000000000000000 ) ) ;
#32765 = CARTESIAN_POINT ( 'NONE',  ( 0.3979743647030599130, -0.9582897341353557863, 0.7577590062044536889 ) ) ;
#32767 = ORIENTED_EDGE ( 'NONE', *, *, #25287, .F. ) ;
#32766 = ORIENTED_EDGE ( 'NONE', *, *, #34569, .F. ) ;
#32768 = CARTESIAN_POINT ( 'NONE',  ( -3.340522353737697295E-05, -2.021039392244021737, -0.7047055906517447621 ) ) ;
#32769 = EDGE_CURVE ( 'NONE', #13144, #29455, #15150, .T. ) ;
#32770 = VERTEX_POINT ( 'NONE', #1104 ) ;
#32771 = FACE_OUTER_BOUND ( 'NONE', #19237, .T. ) ;
#32772 = PRODUCT_DEFINITION_SHAPE ( 'NONE', 'NONE',  #6386 ) ;
#32773 = CARTESIAN_POINT ( 'NONE',  ( 0.5748924173612297572, -1.497770436704561225, 0.5496990462718794879 ) ) ;
#32774 = CARTESIAN_POINT ( 'NONE',  ( -0.04085667396267504692, 0.4547700361314930273, -0.1255037944140887374 ) ) ;
#32775 = ORIENTED_EDGE ( 'NONE', *, *, #2652, .T. ) ;
#32776 = DIRECTION ( 'NONE',  ( 0.01455087616121368381, 0.9998941303972840311, 0.000000000000000000 ) ) ;
#32777 = EDGE_CURVE ( 'NONE', #14064, #28382, #38698, .T. ) ;
#32778 = CARTESIAN_POINT ( 'NONE',  ( 0.1016264643281319241, -0.7104890642553463032, 0.3444698009293519214 ) ) ;
#32779 = ADVANCED_FACE ( 'NONE', ( #23086 ), #8378, .T. ) ;
#32780 = CARTESIAN_POINT ( 'NONE',  ( 0.2384583617500354302, -1.436931818112165304, 1.018057733393896713 ) ) ;
#32781 = CARTESIAN_POINT ( 'NONE',  ( 0.1197289683102586016, -0.7024797939781459721, 0.5140782378632711147 ) ) ;
#32782 = CARTESIAN_POINT ( 'NONE',  ( 0.1147219897069867295, -0.4787606155756814474, 0.02504200487939481010 ) ) ;
#32783 = CARTESIAN_POINT ( 'NONE',  ( 0.09405652007159635841, -0.9320331711797807950, 0.1940232244174328602 ) ) ;
#32784 = ORIENTED_EDGE ( 'NONE', *, *, #4228, .T. ) ;
#32785 = EDGE_CURVE ( 'NONE', #23204, #36736, #17533, .T. ) ;
#32786 = EDGE_CURVE ( 'NONE', #18607, #1427, #21959, .T. ) ;
#32787 = CARTESIAN_POINT ( 'NONE',  ( 0.6505833821421317387, -1.551223176788856017, -0.6117998873676726568 ) ) ;
#32788 = CARTESIAN_POINT ( 'NONE',  ( 0.1928073709365069055, -0.5609073072382156910, 0.2588347484435389867 ) ) ;
#32789 = EDGE_CURVE ( 'NONE', #21211, #32720, #27853, .T. ) ;
#32790 = CARTESIAN_POINT ( 'NONE',  ( 2.372745691485074899E-32, -7.971802777789931753E-17, -0.1749999999999999889 ) ) ;
#32791 = CARTESIAN_POINT ( 'NONE',  ( 0.4409062655693438137, -1.690090444797295977, -0.2869361388274795921 ) ) ;
#32792 = CARTESIAN_POINT ( 'NONE',  ( 0.1909286924077255587, -1.257064795538239022, -0.6702538898043716165 ) ) ;
#32793 = PLANE ( 'NONE',  #11949 ) ;
#32794 = CARTESIAN_POINT ( 'NONE',  ( 0.6149708076787919753, -1.290796914294373154, 0.6294291921256529587 ) ) ;
#32795 = CARTESIAN_POINT ( 'NONE',  ( 0.02999999999997886302, -2.183180860297921466, -0.4937760292030871079 ) ) ;
#32796 = ADVANCED_FACE ( 'NONE', ( #38916 ), #20015, .T. ) ;
#32797 = APPLIED_PERSON_AND_ORGANIZATION_ASSIGNMENT ( #14191, #4322, ( #7895 ) ) ;
#32798 = CARTESIAN_POINT ( 'NONE',  ( 0.04100175935075398709, -1.705062125326649580, -0.3379690677246707242 ) ) ;
#32799 = CARTESIAN_POINT ( 'NONE',  ( 0.5284743900675886730, -1.670479918469192970, -0.5846305483259907065 ) ) ;
#32800 = CARTESIAN_POINT ( 'NONE',  ( 0.4137847586607279471, -1.167177869783954769, 0.7350384739651065757 ) ) ;
#32801 = DIRECTION ( 'NONE',  ( 0.8660254037844378194, -0.4079706259167369953, -0.2890674114961894747 ) ) ;
#32802 = CARTESIAN_POINT ( 'NONE',  ( -0.05634490452573009955, -0.2738187358595995380, -0.3682637492038659532 ) ) ;
#32803 = ORIENTED_EDGE ( 'NONE', *, *, #35438, .T. ) ;
#32804 = CARTESIAN_POINT ( 'NONE',  ( 0.5382321766149029685, -1.161161941655082241, 0.5682417262808779901 ) ) ;
#32805 = CARTESIAN_POINT ( 'NONE',  ( 0.09270007612672712116, -0.5904679391847083014, 0.2514941034432642275 ) ) ;
#32806 = CARTESIAN_POINT ( 'NONE',  ( 0.3645450313092892247, -1.732400383701045543, -0.4756653114284276063 ) ) ;
#32807 = CARTESIAN_POINT ( 'NONE',  ( 0.4190933895477946258, -1.125838976618574794, 0.5206150500282121785 ) ) ;
#32808 = EDGE_CURVE ( 'NONE', #17096, #26041, #2888, .T. ) ;
#32809 = CARTESIAN_POINT ( 'NONE',  ( 0.03443964932668500817, -0.8458729558187815245, 0.2864153933819110764 ) ) ;
#32810 = ORIENTED_EDGE ( 'NONE', *, *, #18193, .F. ) ;
#32811 = CARTESIAN_POINT ( 'NONE',  ( -0.01548846960721252282, 0.3688619771570396666, 0.3775276577325177296 ) ) ;
#32812 = DIRECTION ( 'NONE',  ( -1.000000000000000000, -0.000000000000000000, -0.000000000000000000 ) ) ;
#32813 = CARTESIAN_POINT ( 'NONE',  ( 0.1294752625188461959, -1.408006024206290618, 0.4661737917874986259 ) ) ;
#32814 = DIRECTION ( 'NONE',  ( 1.000000000000000000, -0.000000000000000000, -0.000000000000000000 ) ) ;
#32815 = CARTESIAN_POINT ( 'NONE',  ( 0.4413656098955364149, -1.203038416578624537, 0.7052521412975559789 ) ) ;
#32817 = CARTESIAN_POINT ( 'NONE',  ( -0.2399999999999999079, -3.285933380171606188, -0.6294744526254046901 ) ) ;
#32816 = LINE ( 'NONE', #33238, #30509 ) ;
#32818 = CARTESIAN_POINT ( 'NONE',  ( 0.5749221830005468714, -1.540359961810453759, -0.4819944042435657661 ) ) ;
#32819 = ORIENTED_EDGE ( 'NONE', *, *, #20999, .F. ) ;
#32820 = ORIENTED_EDGE ( 'NONE', *, *, #1664, .F. ) ;
#32821 = ADVANCED_FACE ( 'NONE', ( #39137 ), #6957, .T. ) ;
#32822 = CARTESIAN_POINT ( 'NONE',  ( 0.1905024329569575126, -0.5477411782657776174, 0.05501147976861575639 ) ) ;
#32823 = CARTESIAN_POINT ( 'NONE',  ( 0.05799458868365583303, -0.6184633329593671736, 0.3905354639499808433 ) ) ;
#32825 = CARTESIAN_POINT ( 'NONE',  ( 0.08512636967132125587, -0.7679112480786964845, 0.1451308451931132282 ) ) ;
#32824 = CARTESIAN_POINT ( 'NONE',  ( 0.08980247528055333717, -0.5441805327445274898, 0.1299383132500184224 ) ) ;
#32826 = CARTESIAN_POINT ( 'NONE',  ( -0.2399999999999999079, -3.941790907013290823, -0.4084369376873030477 ) ) ;
#32827 = EDGE_LOOP ( 'NONE', ( #34454, #24944, #32672, #26095, #15832, #20998 ) ) ;
#32828 = EDGE_CURVE ( 'NONE', #38406, #19999, #29167, .T. ) ;
#32829 = ORIENTED_EDGE ( 'NONE', *, *, #1662, .T. ) ;
#32830 = DIRECTION ( 'NONE',  ( 1.000000000000000000, -0.000000000000000000, -0.000000000000000000 ) ) ;
#32831 = ADVANCED_FACE ( 'NONE', ( #1122 ), #4365, .F. ) ;
#32832 = CARTESIAN_POINT ( 'NONE',  ( 0.5748742142425384838, -1.498333522039650978, 0.6063947612278407506 ) ) ;
#32833 = VERTEX_POINT ( 'NONE', #32745 ) ;
#32834 = DIRECTION ( 'NONE',  ( -1.000000000000000000, -6.779273404243070203E-32, -4.314083075427408311E-32 ) ) ;
#32835 = CARTESIAN_POINT ( 'NONE',  ( 0.05279755784604210633, -0.4315508301037762617, 0.1821553064136585132 ) ) ;
#32836 = CARTESIAN_POINT ( 'NONE',  ( 0.3811932541547525810, -1.750588582039273033, -0.4368655358042922709 ) ) ;
#32837 = CARTESIAN_POINT ( 'NONE',  ( 0.2095916371365568465, -1.234515458870462989, 0.4716905264182155721 ) ) ;
#32838 = CIRCLE ( 'NONE', #36863, 0.1000000000000000194 ) ;
#32839 = CARTESIAN_POINT ( 'NONE',  ( 0.3925301276612734314, -1.756377271995030576, -0.4843757382520814114 ) ) ;
#32840 = DIRECTION ( 'NONE',  ( -1.000000000000000000, 0.000000000000000000, 0.000000000000000000 ) ) ;
#32841 = MANIFOLD_SOLID_BREP ( 'Extrude-Thin1', #9588 ) ;
#32842 = CARTESIAN_POINT ( 'NONE',  ( 0.1875419504463087250, -0.4620869884079685241, 0.1831780322516418646 ) ) ;
#32843 = CIRCLE ( 'NONE', #32941, 0.01499999999999994740 ) ;
#32844 = CARTESIAN_POINT ( 'NONE',  ( 0.07556315841227359553, -1.331191507351498160, 0.4849083929475443422 ) ) ;
#32845 = ADVANCED_FACE ( 'NONE', ( #26988 ), #1910, .T. ) ;
#32846 = CARTESIAN_POINT ( 'NONE',  ( -0.01548846960707477016, 0.4770632572900446178, -0.2530032579707474083 ) ) ;
#32847 = EDGE_CURVE ( 'NONE', #14101, #16124, #14421, .T. ) ;
#32848 = CARTESIAN_POINT ( 'NONE',  ( 0.6016870789291266508, -1.595135992794870727, -0.4985500141948422947 ) ) ;
#32849 = EDGE_CURVE ( 'NONE', #34885, #37816, #10107, .T. ) ;
#32850 = CARTESIAN_POINT ( 'NONE',  ( 0.05561375719525510353, 0.2871676730027915569, 0.3605331597494266793 ) ) ;
#32851 = CARTESIAN_POINT ( 'NONE',  ( -0.1126900943574667691, -0.5191528599708477021, 0.3032895567580773388 ) ) ;
#32852 = CARTESIAN_POINT ( 'NONE',  ( 0.4039331521932674751, -1.711434328629108714, 0.5182417262808777236 ) ) ;
#32853 = LINE ( 'NONE', #4656, #6123 ) ;
#32854 = CARTESIAN_POINT ( 'NONE',  ( -0.1399999999999997358, 0.000000000000000000, 0.000000000000000000 ) ) ;
#32855 = CARTESIAN_POINT ( 'NONE',  ( 0.5714446559762420552, -1.545268339499498378, -0.5210154178133508118 ) ) ;
#32856 = CARTESIAN_POINT ( 'NONE',  ( -0.1499999999999996336, 4.163336342344336410E-17, 0.1249999999999999584 ) ) ;
#32857 = CARTESIAN_POINT ( 'NONE',  ( 0.3047917418918154042, -1.756872425756282219, 0.5682432986887175907 ) ) ;
#32858 = CARTESIAN_POINT ( 'NONE',  ( -0.05252359774140241688, -0.2683439431814180764, 0.3847367734645306125 ) ) ;
#32859 = ORIENTED_EDGE ( 'NONE', *, *, #11943, .F. ) ;
#32860 = ORIENTED_EDGE ( 'NONE', *, *, #30240, .F. ) ;
#32861 = CARTESIAN_POINT ( 'NONE',  ( 0.1626176757286639796, -0.6782218769987641283, 0.05683303076865411224 ) ) ;
#32862 = CARTESIAN_POINT ( 'NONE',  ( -0.3000000000000000999, -1.874946189051298617, -0.07947534077849525980 ) ) ;
#32863 = ORIENTED_EDGE ( 'NONE', *, *, #2720, .T. ) ;
#32864 = DIRECTION ( 'NONE',  ( -1.000000000000000000, -7.857794173099924470E-32, -8.628166150854818811E-32 ) ) ;
#32865 = CARTESIAN_POINT ( 'NONE',  ( 0.01548846960707514486, -0.4638115001430951345, 0.2459753896937915962 ) ) ;
#32866 = CARTESIAN_POINT ( 'NONE',  ( 0.4872548453982092354, -1.278504979452121937, 0.7792526119054953293 ) ) ;
#32867 = AXIS2_PLACEMENT_3D ( 'NONE', #35313, #7102, #21968 ) ;
#32869 = ORIENTED_EDGE ( 'NONE', *, *, #38600, .F. ) ;
#32868 = CARTESIAN_POINT ( 'NONE',  ( -0.1524980003306027898, 0.4722686132664294933, 0.1089215716291629665 ) ) ;
#32870 = CARTESIAN_POINT ( 'NONE',  ( 0.1843752803354802017, -0.7900634509218507073, 0.1541083617713018827 ) ) ;
#32871 = DIRECTION ( 'NONE',  ( 1.000000000000000000, 0.000000000000000000, 7.906745362128971688E-16 ) ) ;
#32872 = ORIENTED_EDGE ( 'NONE', *, *, #11507, .T. ) ;
#32873 = FACE_OUTER_BOUND ( 'NONE', #39450, .T. ) ;
#32874 = AXIS2_PLACEMENT_3D ( 'NONE', #19767, #38688, #32304 ) ;
#32875 = CARTESIAN_POINT ( 'NONE',  ( 0.02413263538073280590, -0.5564134470917985187, 0.2552522691244957787 ) ) ;
#32877 = CARTESIAN_POINT ( 'NONE',  ( 0.1150181919530900154, -0.4575939575325503328, 0.07184729873914598441 ) ) ;
#32876 = CARTESIAN_POINT ( 'NONE',  ( 0.7037767268368668727, -1.494333256273129074, 0.5114234088782623200 ) ) ;
#32878 = CARTESIAN_POINT ( 'NONE',  ( 0.4089992519647981384, -1.131314579718122992, 0.3157417262808777658 ) ) ;
#32879 = AXIS2_PLACEMENT_3D ( 'NONE', #29046, #914, #9305 ) ;
#32880 = EDGE_CURVE ( 'NONE', #12872, #8583, #11150, .T. ) ;
#32881 = CARTESIAN_POINT ( 'NONE',  ( 0.3999999999999787059, -2.097675824466503691, -0.4937760292030871079 ) ) ;
#32882 = VERTEX_POINT ( 'NONE', #8261 ) ;
#32883 = CARTESIAN_POINT ( 'NONE',  ( 0.4262438152663738933, -1.592651821845863402, -0.6151431148613257793 ) ) ;
#32884 = CARTESIAN_POINT ( 'NONE',  ( 0.1742696185895059313, -1.268084925919871431, 0.4182417262808778013 ) ) ;
#32885 = DIRECTION ( 'NONE',  ( 0.000000000000000000, 0.4393346272634469085, 0.8983234858820557944 ) ) ;
#32886 = CARTESIAN_POINT ( 'NONE',  ( 0.1284000471068089122, -0.8566673793669413728, 0.4510511576820184776 ) ) ;
#32887 = CARTESIAN_POINT ( 'NONE',  ( 0.5985082606850495868, -1.473464502187743941, 0.6023744451300401259 ) ) ;
#32888 = DIRECTION ( 'NONE',  ( -0.8660512985181135770, -0.4999551463232371207, 0.000000000000000000 ) ) ;
#32889 = CARTESIAN_POINT ( 'NONE',  ( 0.1343890788881223208, -0.9415398979786367972, 0.3700653858661135387 ) ) ;
#32890 = DIRECTION ( 'NONE',  ( -1.000000000000000000, -2.280301054154495132E-31, 1.664003471950577689E-31 ) ) ;
#32891 = CARTESIAN_POINT ( 'NONE',  ( 0.1399999999999994582, -4.527947890665460015E-17, -0.2150000000000000244 ) ) ;
#32892 = DIRECTION ( 'NONE',  ( 7.771561172376107616E-16, -7.170354002788761615E-17, 1.000000000000000000 ) ) ;
#32893 = CARTESIAN_POINT ( 'NONE',  ( 0.2755305116007160104, -1.669965222996684151, 0.4753282117146875874 ) ) ;
#32894 = DIRECTION ( 'NONE',  ( 2.181870543673301168E-16, 0.2799043398077594724, -0.9600278957180266026 ) ) ;
#32895 = EDGE_CURVE ( 'NONE', #6931, #16637, #32443, .T. ) ;
#32896 = VECTOR ( 'NONE', #33798, 39.37007874015748143 ) ;
#32897 = APPLIED_DATE_AND_TIME_ASSIGNMENT ( #24299, #20609, ( #20163 ) ) ;
#32898 = EDGE_CURVE ( 'NONE', #40308, #36434, #37240, .T. ) ;
#32899 = CARTESIAN_POINT ( 'NONE',  ( 0.4136407012227684699, -1.144011212594888027, 0.4262611942485852734 ) ) ;
#32900 = DIRECTION ( 'NONE',  ( -0.4999551463232372317, 0.8660512985181135770, -0.000000000000000000 ) ) ;
#32901 = DIRECTION ( 'NONE',  ( -0.4999551463232372317, 0.8660512985181135770, -0.000000000000000000 ) ) ;
#32902 =( BOUNDED_SURFACE ( )  B_SPLINE_SURFACE ( 3, 2, ( 
 ( #26497, #32851, #32450 ),
 ( #19707, #6953, #29173 ),
 ( #13727, #4654, #39032 ),
 ( #4059, #28959, #17033 ) ),
 .UNSPECIFIED., .F., .F., .F. ) 
 B_SPLINE_SURFACE_WITH_KNOTS ( ( 4, 4 ),
 ( 3, 3 ),
 ( 0.001168341556843763198, 0.001551611072815416289 ),
 ( 0.000000000000000000, 1.000000000000000000 ),
 .UNSPECIFIED. ) 
 GEOMETRIC_REPRESENTATION_ITEM ( )  RATIONAL_B_SPLINE_SURFACE ( (
 ( 1.000000000000000000, 0.8989970956543047453, 1.000000000000000000),
 ( 1.000000000000000000, 0.8989738193133397504, 1.000000000000000000),
 ( 1.000000000000000000, 0.9033319494950228234, 1.000000000000000000),
 ( 1.000000000000000000, 0.9117915798252440585, 1.000000000000000000) ) ) 
 REPRESENTATION_ITEM ( '' )  SURFACE ( )  );
#32903 = EDGE_CURVE ( 'NONE', #31663, #3174, #20563, .T. ) ;
#32904 = CIRCLE ( 'NONE', #26346, 0.02999999999999996073 ) ;
#32905 = DIRECTION ( 'NONE',  ( 0.000000000000000000, 0.000000000000000000, -1.000000000000000000 ) ) ;
#32906 = CARTESIAN_POINT ( 'NONE',  ( 0.3752374054691312577, -1.754338789473355087, -0.5850131874919822783 ) ) ;
#32907 = AXIS2_PLACEMENT_3D ( 'NONE', #17215, #27086, #4452 ) ;
#32908 = CARTESIAN_POINT ( 'NONE',  ( -0.02000000000000000042, -2.183180860297908144, -0.3317586832283064280 ) ) ;
#32909 = CARTESIAN_POINT ( 'NONE',  ( 0.3699999999999786793, -2.183180860297921466, -0.4937760292030871079 ) ) ;
#32910 = ORIENTED_EDGE ( 'NONE', *, *, #5936, .F. ) ;
#32911 = EDGE_LOOP ( 'NONE', ( #36729, #36867, #21459, #3243 ) ) ;
#32912 = CARTESIAN_POINT ( 'NONE',  ( 0.1805708897690167514, -0.4954670953086038887, 0.09376884823743399100 ) ) ;
#32913 = EDGE_LOOP ( 'NONE', ( #24292, #37471, #2477, #23201, #26664 ) ) ;
#32914 = DIRECTION ( 'NONE',  ( -0.8132816101496389560, -0.4694921964796399116, -0.3437296903631308909 ) ) ;
#32915 = CARTESIAN_POINT ( 'NONE',  ( 0.1348549594756914827, -0.5515731166344398639, 0.1457185332388696020 ) ) ;
#32917 = VERTEX_POINT ( 'NONE', #27201 ) ;
#32916 = CARTESIAN_POINT ( 'NONE',  ( 0.006527597169688036625, -0.8304684498530628955, 0.07759244090682963779 ) ) ;
#32918 = VECTOR ( 'NONE', #39776, 39.37007874015748143 ) ;
#32919 = ORIENTED_EDGE ( 'NONE', *, *, #23932, .T. ) ;
#32920 = CARTESIAN_POINT ( 'NONE',  ( 0.2545402541793244100, -0.8054584187335094292, 0.7501033274436699205 ) ) ;
#32921 = ORIENTED_EDGE ( 'NONE', *, *, #39578, .T. ) ;
#32922 = CARTESIAN_POINT ( 'NONE',  ( 0.02304533052768314300, -0.7671398829736530978, 0.6375630150525929407 ) ) ;
#32924 = FACE_OUTER_BOUND ( 'NONE', #21974, .T. ) ;
#32923 = CARTESIAN_POINT ( 'NONE',  ( -0.01895884884825181985, -0.4667865995382943223, -0.2292744456225760119 ) ) ;
#32925 = DIRECTION ( 'NONE',  ( 0.000000000000000000, 0.000000000000000000, -1.000000000000000000 ) ) ;
#32926 = CONTEXT_DEPENDENT_SHAPE_REPRESENTATION ( #27941, #20657 ) ;
#32927 = AXIS2_PLACEMENT_3D ( 'NONE', #6510, #25466, #22380 ) ;
#32928 = EDGE_CURVE ( 'NONE', #23647, #8779, #34419, .T. ) ;
#32929 = ADVANCED_FACE ( 'NONE', ( #21022 ), #20637, .T. ) ;
#32930 = CARTESIAN_POINT ( 'NONE',  ( 0.05999999999999990757, 0.2165002077672316116, -0.1331859471648322857 ) ) ;
#32932 = ORIENTED_EDGE ( 'NONE', *, *, #12679, .F. ) ;
#32931 = ORIENTED_EDGE ( 'NONE', *, *, #32898, .T. ) ;
#32933 = AXIS2_PLACEMENT_3D ( 'NONE', #28156, #35136, #34719 ) ;
#32934 = CARTESIAN_POINT ( 'NONE',  ( 0.1042439066782299417, -0.8091407591346367889, 0.3631625727402441051 ) ) ;
#32935 = CARTESIAN_POINT ( 'NONE',  ( 0.1186935531864466153, -1.414102003872103275, 0.5711544693646362081 ) ) ;
#32936 = CARTESIAN_POINT ( 'NONE',  ( 0.1345564120588943480, -0.7468426462781448949, 0.5714576363270958970 ) ) ;
#32937 = VECTOR ( 'NONE', #36108, 39.37007874015748143 ) ;
#32938 = CARTESIAN_POINT ( 'NONE',  ( 0.1162496453231299381, -0.5482924977647862796, 0.1457185332388695187 ) ) ;
#32939 = CARTESIAN_POINT ( 'NONE',  ( 0.03811508589225207772, -1.111219027208512289, 0.6472413928917138959 ) ) ;
#32940 = DIRECTION ( 'NONE',  ( 1.000000000000000000, 0.000000000000000000, 0.000000000000000000 ) ) ;
#32941 = AXIS2_PLACEMENT_3D ( 'NONE', #20990, #33321, #36201 ) ;
#32942 = CARTESIAN_POINT ( 'NONE',  ( 0.3211351646105950475, -1.297358875900399999, 0.4290006342139815465 ) ) ;
#32943 = CONICAL_SURFACE ( 'NONE', #19792, 0.1600000000000000588, 1.047197551196602738 ) ;
#32944 = CARTESIAN_POINT ( 'NONE',  ( -1.920743219377653022, -2.938248161666755287, 0.6057417262804746239 ) ) ;
#32945 = DIRECTION ( 'NONE',  ( 0.000000000000000000, 3.330669073875470114E-16, 1.000000000000000000 ) ) ;
#32946 = CARTESIAN_POINT ( 'NONE',  ( 0.5057508247701024695, -1.620212811793598107, -0.5782665205887309590 ) ) ;
#32947 = PLANE ( 'NONE',  #883 ) ;
#32948 = CARTESIAN_POINT ( 'NONE',  ( -2.070754768975509474, -0.09959325338431662678, 0.3750000000000004996 ) ) ;
#32949 = CARTESIAN_POINT ( 'NONE',  ( -5.815845300111390967E-05, -0.7445727859702501172, -0.09684046364400783480 ) ) ;
#32950 = CARTESIAN_POINT ( 'NONE',  ( 0.06925724349164365246, -0.5402022796555754347, 0.1536732814500230693 ) ) ;
#32951 = CARTESIAN_POINT ( 'NONE',  ( 0.006952085198512917251, -0.8063998755378689598, 0.04117179503985820416 ) ) ;
#32952 = CARTESIAN_POINT ( 'NONE',  ( -0.01548846960707524721, -0.4638115001430989648, 0.2459753896937853235 ) ) ;
#32953 = CARTESIAN_POINT ( 'NONE',  ( -0.003124719664520048124, -0.8057675726412016903, 0.1457185332388697963 ) ) ;
#32954 = CARTESIAN_POINT ( 'NONE',  ( 0.2179926414509053834, -0.8923039640295803432, 0.4033837261968737375 ) ) ;
#32955 = APPROVAL_STATUS ( 'not_yet_approved' ) ;
#32956 = CARTESIAN_POINT ( 'NONE',  ( 0.1952857665188987568, -0.5148003437455072051, 0.3467747870930740217 ) ) ;
#32957 = AXIS2_PLACEMENT_3D ( 'NONE', #32422, #14114, #1589 ) ;
#32958 = EDGE_CURVE ( 'NONE', #4624, #23581, #16687, .T. ) ;
#32959 = CARTESIAN_POINT ( 'NONE',  ( -0.02000000000000000042, -2.179113517810423062, -0.3318097452986852880 ) ) ;
#32960 = CARTESIAN_POINT ( 'NONE',  ( 0.3061685498075335521, -1.759171299767175567, 0.5690271169898788450 ) ) ;
#32961 = CIRCLE ( 'NONE', #17838, 0.5400000000000015898 ) ;
#32962 = CIRCLE ( 'NONE', #35612, 0.1000000000000000194 ) ;
#32963 = ORIENTED_EDGE ( 'NONE', *, *, #39910, .F. ) ;
#32964 = DIRECTION ( 'NONE',  ( -1.000000000000000000, 0.000000000000000000, 0.000000000000000000 ) ) ;
#32965 = CARTESIAN_POINT ( 'NONE',  ( 0.03078253484063611309, -0.7501471350750349432, 0.6269559300169642579 ) ) ;
#32966 = CIRCLE ( 'NONE', #17843, 0.5302738246768088359 ) ;
#32967 = DIRECTION ( 'NONE',  ( 8.881784197001246407E-16, -2.361472542561082612E-16, 1.000000000000000000 ) ) ;
#32968 = ORIENTED_EDGE ( 'NONE', *, *, #5019, .T. ) ;
#32969 = LINE ( 'NONE', #30099, #23237 ) ;
#32970 = CARTESIAN_POINT ( 'NONE',  ( 0.1896879205916190136, -0.5058468364965200692, 0.1731371019803292222 ) ) ;
#32972 = ORIENTED_EDGE ( 'NONE', *, *, #15008, .F. ) ;
#32971 = VERTEX_POINT ( 'NONE', #39939 ) ;
#32973 = CARTESIAN_POINT ( 'NONE',  ( 0.1153287684445949701, -1.330270486660940277, -0.7080039676230125423 ) ) ;
#32974 = CARTESIAN_POINT ( 'NONE',  ( 0.3595108577967162100, -1.929697767679888987, -0.4979555812093512390 ) ) ;
#32975 = CARTESIAN_POINT ( 'NONE',  ( -0.02000000000000000042, -2.196071624283071788, -1.002400088386023791 ) ) ;
#32976 = PERSON_AND_ORGANIZATION_ROLE ( 'classification_officer' ) ;
#32977 = DIRECTION ( 'NONE',  ( 0.4999551463232372317, -0.8660512985181135770, 0.000000000000000000 ) ) ;
#32978 = VERTEX_POINT ( 'NONE', #14630 ) ;
#32979 = AXIS2_PLACEMENT_3D ( 'NONE', #21717, #28284, #24999 ) ;
#32980 = FACE_OUTER_BOUND ( 'NONE', #31179, .T. ) ;
#32981 = CARTESIAN_POINT ( 'NONE',  ( 0.09897633131546774987, -0.6690318149839973305, 0.3230829238930963410 ) ) ;
#32982 = CARTESIAN_POINT ( 'NONE',  ( 0.1481019126683178200, -1.101867350517807154, 0.9906736688113091382 ) ) ;
#32983 = CARTESIAN_POINT ( 'NONE',  ( 0.4971680109405678394, -1.542412852845005622, 0.5685800135497441898 ) ) ;
#32985 = CARTESIAN_POINT ( 'NONE',  ( 0.3405242896115074913, -1.744906522954273731, 0.4484829386636806081 ) ) ;
#32984 = CARTESIAN_POINT ( 'NONE',  ( 0.2638148871170554743, -1.623480815898712848, 0.8273393273315299279 ) ) ;
#32986 = CARTESIAN_POINT ( 'NONE',  ( 0.1421613555067215151, -0.9980800295453481352, 0.5465807779430843505 ) ) ;
#32987 = ORIENTED_EDGE ( 'NONE', *, *, #39666, .T. ) ;
#32988 = ORIENTED_EDGE ( 'NONE', *, *, #8922, .F. ) ;
#32989 = CARTESIAN_POINT ( 'NONE',  ( 0.05562144613422614903, -0.4316454521248588860, -0.1615915407302030427 ) ) ;
#32990 = CARTESIAN_POINT ( 'NONE',  ( 0.1888885414493101933, -0.4614316578175808314, 0.1777954161997660487 ) ) ;
#32991 = DIRECTION ( 'NONE',  ( -2.465190328815661892E-32, -1.000000000000000000, -6.656013887802287108E-31 ) ) ;
#32992 = AXIS2_PLACEMENT_3D ( 'NONE', #34425, #22504, #40596 ) ;
#32993 = CARTESIAN_POINT ( 'NONE',  ( -0.03171893264487282704, -0.5171391213725057279, -0.08825218502846603197 ) ) ;
#32994 = CIRCLE ( 'NONE', #27758, 0.08830708661417341343 ) ;
#32995 = CARTESIAN_POINT ( 'NONE',  ( 0.07002615672170085792, -1.325404962382359830, 0.5075059737783654823 ) ) ;
#32996 = CARTESIAN_POINT ( 'NONE',  ( 0.4409062655693434807, -1.690090444797295532, -0.5318766032425230605 ) ) ;
#32997 = LINE ( 'NONE', #4803, #21860 ) ;
#32998 = CARTESIAN_POINT ( 'NONE',  ( 0.6014934134068773419, -1.267756190114700976, 0.6768762346975223387 ) ) ;
#32999 = CARTESIAN_POINT ( 'NONE',  ( -0.02000000000000000042, -1.614234636154356251, 0.1774087976708900172 ) ) ;
#33000 = CARTESIAN_POINT ( 'NONE',  ( 0.03256515207864835171, -1.845689418459394826, -0.3210198295332938323 ) ) ;
#33001 = CARTESIAN_POINT ( 'NONE',  ( 0.5260376822698199506, -1.642293686627224414, -0.5683488690136782040 ) ) ;
#33002 = VERTEX_POINT ( 'NONE', #21450 ) ;
#33003 = ADVANCED_FACE ( 'NONE', ( #5780 ), #27599, .F. ) ;
#33004 = CARTESIAN_POINT ( 'NONE',  ( 0.4544434295504399812, -1.214367261269359233, 0.6181573591564563097 ) ) ;
#33005 = DIRECTION ( 'NONE',  ( 0.4999999999999973910, -0.6123724356957970238, 0.6123724356957940262 ) ) ;
#33006 = ADVANCED_FACE ( 'NONE', ( #34369 ), #37677, .F. ) ;
#33007 = CARTESIAN_POINT ( 'NONE',  ( 0.000000000000000000, 0.000000000000000000, 0.000000000000000000 ) ) ;
#33008 = ADVANCED_FACE ( 'NONE', ( #11957 ), #11678, .F. ) ;
#33009 = VERTEX_POINT ( 'NONE', #10090 ) ;
#33010 = CARTESIAN_POINT ( 'NONE',  ( 0.4145682426820113120, -1.006442754038745724, 0.7096782495508600075 ) ) ;
#33011 = CARTESIAN_POINT ( 'NONE',  ( 2.372745691485074352E-32, -3.685538980774211798E-17, -0.1749999999999999889 ) ) ;
#33012 = EDGE_CURVE ( 'NONE', #37890, #11376, #19104, .T. ) ;
#33013 = CIRCLE ( 'NONE', #24488, 0.009999999999999996739 ) ;
#33014 = FACE_OUTER_BOUND ( 'NONE', #37014, .T. ) ;
#33015 = EDGE_CURVE ( 'NONE', #15711, #39260, #38064, .T. ) ;
#33016 = CARTESIAN_POINT ( 'NONE',  ( 0.2057862311405771472, -1.177123548154546562, 0.7473132801419769544 ) ) ;
#33017 = ORIENTED_EDGE ( 'NONE', *, *, #31377, .F. ) ;
#33018 = CARTESIAN_POINT ( 'NONE',  ( -0.04230188431063483523, 0.2683773510969766352, 0.3842417364743013763 ) ) ;
#33019 = CIRCLE ( 'NONE', #33664, 0.02999999999999997113 ) ;
#33020 = SHAPE_REPRESENTATION ( 'pulley subassembly', ( #31163, #39050, #29189, #20656, #33115, #2271 ), #11460 ) ;
#33021 = AXIS2_PLACEMENT_3D ( 'NONE', #35905, #4811, #20897 ) ;
#33022 = DIRECTION ( 'NONE',  ( 2.532366176626898926E-12, -0.8090169943749432324, 0.5877852522924789103 ) ) ;
#33023 = CARTESIAN_POINT ( 'NONE',  ( 0.02953079040095537774, -0.5250338024619286559, -0.07436286310882828099 ) ) ;
#33024 = DIRECTION ( 'NONE',  ( 1.093267065177649503E-16, -0.4506112020353472136, 0.8927203059190820245 ) ) ;
#33025 = AXIS2_PLACEMENT_3D ( 'NONE', #37026, #30459, #15438 ) ;
#33026 = CARTESIAN_POINT ( 'NONE',  ( 0.4471179260400731659, -1.207645768960549093, 0.6708866534528135084 ) ) ;
#33028 = CARTESIAN_POINT ( 'NONE',  ( -0.05464101615137762630, -1.968175500587574067, -0.6048844944454191408 ) ) ;
#33027 = CARTESIAN_POINT ( 'NONE',  ( 2.048885995248197414E-16, 0.2900000000000004796, -5.122214988120493288E-16 ) ) ;
#33029 = DIRECTION ( 'NONE',  ( -1.000000000000000000, 0.000000000000000000, 0.000000000000000000 ) ) ;
#33030 = ORIENTED_EDGE ( 'NONE', *, *, #34164, .F. ) ;
#33031 = CARTESIAN_POINT ( 'NONE',  ( 0.5959315179729184342, -1.587052097778459236, 0.4182417262808776903 ) ) ;
#33032 = ORIENTED_EDGE ( 'NONE', *, *, #14788, .T. ) ;
#33033 = DIRECTION ( 'NONE',  ( -8.881784197001245421E-16, 2.361472542561082612E-16, -1.000000000000000000 ) ) ;
#33034 = CARTESIAN_POINT ( 'NONE',  ( 0.4136966911965741511, -1.589565852169850135, 0.5748244833461771952 ) ) ;
#33035 = CIRCLE ( 'NONE', #18598, 0.06250000000000001388 ) ;
#33036 = ADVANCED_FACE ( 'NONE', ( #37876 ), #34770, .T. ) ;
#33038 = CARTESIAN_POINT ( 'NONE',  ( 0.08873781644304089278, -0.6437611796408930775, 0.1460192843988557254 ) ) ;
#33037 = CARTESIAN_POINT ( 'NONE',  ( 0.08957455089030209872, -0.5701463690649801741, 0.1081760157455312760 ) ) ;
#33039 = DIRECTION ( 'NONE',  ( -1.000000000000000000, 0.000000000000000000, -0.000000000000000000 ) ) ;
#33040 = APPROVAL ( #38529, 'UNSPECIFIED' ) ;
#33041 = VERTEX_POINT ( 'NONE', #35199 ) ;
#33042 = DIRECTION ( 'NONE',  ( 0.8660512985181135770, 0.4999551463232370652, 0.000000000000000000 ) ) ;
#33043 = CARTESIAN_POINT ( 'NONE',  ( 0.5742732429853925069, -1.495958998523723382, 0.6323022671693150354 ) ) ;
#33044 = ORIENTED_EDGE ( 'NONE', *, *, #35326, .F. ) ;
#33045 = CARTESIAN_POINT ( 'NONE',  ( 0.3135981152340067135, -1.763401867015618185, 0.5450985680089832641 ) ) ;
#33046 = CARTESIAN_POINT ( 'NONE',  ( 0.02242828275839356053, -0.5043161982043002922, 0.09034400517546492537 ) ) ;
#33047 = CARTESIAN_POINT ( 'NONE',  ( 0.6449624452930813323, -1.552575692319365652, 0.4182417262808776348 ) ) ;
#33048 = CARTESIAN_POINT ( 'NONE',  ( 0.2120822108312993837, -1.233077460334429443, 0.4766410756411681438 ) ) ;
#33049 = AXIS2_PLACEMENT_3D ( 'NONE', #19522, #19320, #20131 ) ;
#33050 = CARTESIAN_POINT ( 'NONE',  ( 0.08058916068514494768, -1.309220013881624123, 0.4727703015479320370 ) ) ;
#33051 = CARTESIAN_POINT ( 'NONE',  ( 0.01548846960707524721, 0.4770632572900446178, -0.2530032579707474083 ) ) ;
#33052 = CARTESIAN_POINT ( 'NONE',  ( 0.2803613453953150980, -0.7205873319272890765, 0.6521004353453685454 ) ) ;
#33053 = VECTOR ( 'NONE', #37414, 39.37007874015748143 ) ;
#33054 = VECTOR ( 'NONE', #14897, 39.37007874015748854 ) ;
#33055 = FACE_OUTER_BOUND ( 'NONE', #1693, .T. ) ;
#33056 = CARTESIAN_POINT ( 'NONE',  ( 0.01548846960712797240, -0.3688619771571953754, -0.3775276577326278082 ) ) ;
#33057 = CARTESIAN_POINT ( 'NONE',  ( 0.6080071089777098203, -1.584981494572885730, -0.5642241644406634782 ) ) ;
#33058 = CARTESIAN_POINT ( 'NONE',  ( 0.2325938614944302874, -1.347997356825076487, 0.5182417262812506475 ) ) ;
#33059 = DIRECTION ( 'NONE',  ( 0.4999551463232372317, -0.8660512985181135770, 0.000000000000000000 ) ) ;
#33060 = AXIS2_PLACEMENT_3D ( 'NONE', #3262, #31652, #822 ) ;
#33061 = CARTESIAN_POINT ( 'NONE',  ( -0.02000000000000000042, -1.761115123485013534, -0.1975702831323159492 ) ) ;
#33062 = EDGE_CURVE ( 'NONE', #25706, #3269, #13393, .T. ) ;
#33063 =( GEOMETRIC_REPRESENTATION_CONTEXT ( 3 ) GLOBAL_UNCERTAINTY_ASSIGNED_CONTEXT ( ( #13265 ) ) GLOBAL_UNIT_ASSIGNED_CONTEXT ( ( #925, #9530, #28246 ) ) REPRESENTATION_CONTEXT ( 'NONE', 'WORKASPACE' ) );
#33064 = CARTESIAN_POINT ( 'NONE',  ( 0.3149693831142335032, -1.765269515322325899, 0.6420921437412323574 ) ) ;
#33065 = CARTESIAN_POINT ( 'NONE',  ( 0.5697212493628158736, -1.577360437427027806, -0.5635484681258001727 ) ) ;
#33066 = ADVANCED_FACE ( 'NONE', ( #3298 ), #3528, .T. ) ;
#33067 = CARTESIAN_POINT ( 'NONE',  ( 0.1211641685807053614, -1.296837725294725407, 0.5378582170338975788 ) ) ;
#33068 = CARTESIAN_POINT ( 'NONE',  ( 0.6835481475269313822, -1.411548362123609790, 0.5857417262805110214 ) ) ;
#33069 = CARTESIAN_POINT ( 'NONE',  ( -0.02881302694830073854, -0.3393464602395944163, 0.3647504210684007764 ) ) ;
#33070 = ADVANCED_FACE ( 'NONE', ( #9876 ), #22875, .F. ) ;
#33071 = VERTEX_POINT ( 'NONE', #16463 ) ;
#33072 = ORIENTED_EDGE ( 'NONE', *, *, #30335, .F. ) ;
#33073 = CARTESIAN_POINT ( 'NONE',  ( 0.4247531631588282730, -1.110879369639613756, 0.6102655838170102376 ) ) ;
#33074 = DIRECTION ( 'NONE',  ( -1.000000000000000000, -0.000000000000000000, -0.000000000000000000 ) ) ;
#33075 = ORIENTED_EDGE ( 'NONE', *, *, #32627, .T. ) ;
#33076 = FACE_OUTER_BOUND ( 'NONE', #22269, .T. ) ;
#33077 = DIRECTION ( 'NONE',  ( 1.000000000000000000, 2.280301054154495132E-31, -1.664003471950577689E-31 ) ) ;
#33078 = AXIS2_PLACEMENT_3D ( 'NONE', #30288, #3484, #6551 ) ;
#33079 = CARTESIAN_POINT ( 'NONE',  ( 0.5317449915470191524, -1.346863324614599344, 0.6223190780326449678 ) ) ;
#33081 = ORIENTED_EDGE ( 'NONE', *, *, #6182, .F. ) ;
#33080 = CARTESIAN_POINT ( 'NONE',  ( -0.1646294012188420086, 0.5114631038222653414, 0.1176773486970827121 ) ) ;
#33082 = CARTESIAN_POINT ( 'NONE',  ( 0.5137780172988268834, -1.118801028709976109, 0.5682417262808779901 ) ) ;
#33083 = CARTESIAN_POINT ( 'NONE',  ( -1.019575837292305609, -0.04310840302198148261, 0.08500000000000004774 ) ) ;
#33084 = ORIENTED_EDGE ( 'NONE', *, *, #34396, .F. ) ;
#33085 = FACE_OUTER_BOUND ( 'NONE', #29298, .T. ) ;
#33086 = AXIS2_PLACEMENT_3D ( 'NONE', #33007, #33224, #38766 ) ;
#33087 = AXIS2_PLACEMENT_3D ( 'NONE', #23031, #6972, #34954 ) ;
#33088 = CARTESIAN_POINT ( 'NONE',  ( 0.2277887942778757668, -1.330934816884134841, 0.9229718230307302207 ) ) ;
#33089 = EDGE_CURVE ( 'NONE', #36909, #12111, #34979, .T. ) ;
#33091 = CARTESIAN_POINT ( 'NONE',  ( 0.1144408672107467828, -0.5040670884152405051, -0.01142007189417859440 ) ) ;
#33090 = CARTESIAN_POINT ( 'NONE',  ( 0.6747034693327369492, -1.517398054291565046, 0.4407624208754166162 ) ) ;
#33092 = CARTESIAN_POINT ( 'NONE',  ( 0.2322138788700108258, -1.233113307957229177, 0.3157417262808777658 ) ) ;
#33093 = FACE_OUTER_BOUND ( 'NONE', #5767, .T. ) ;
#33094 = ORIENTED_EDGE ( 'NONE', *, *, #22549, .F. ) ;
#33095 = AXIS2_PLACEMENT_3D ( 'NONE', #18303, #15419, #37416 ) ;
#33096 = CARTESIAN_POINT ( 'NONE',  ( 0.09514782613886782481, -1.363928122608234927, -0.6711990196306176770 ) ) ;
#33097 = CARTESIAN_POINT ( 'NONE',  ( -0.02000000000000000042, -2.616518742763782601, -0.2555225440839158924 ) ) ;
#33098 = AXIS2_PLACEMENT_3D ( 'NONE', #39735, #8655, #11568 ) ;
#33099 = CARTESIAN_POINT ( 'NONE',  ( 0.3319403630591543641, -1.291129383779237472, 0.5791928922408521307 ) ) ;
#33100 = LINE ( 'NONE', #29611, #27067 ) ;
#33101 = CARTESIAN_POINT ( 'NONE',  ( -0.3000000000000000999, -4.056386786973173564, -0.6915988348251679296 ) ) ;
#33102 = LINE ( 'NONE', #17482, #28443 ) ;
#33103 = FACE_OUTER_BOUND ( 'NONE', #30092, .T. ) ;
#33104 = DIRECTION ( 'NONE',  ( 0.000000000000000000, 0.000000000000000000, -1.000000000000000000 ) ) ;
#33105 = CARTESIAN_POINT ( 'NONE',  ( -0.3000000000000000999, -3.237612445311622622, -0.5419983935656527141 ) ) ;
#33106 = DIRECTION ( 'NONE',  ( -0.5077740042737255433, 0.8614903136912374082, 0.000000000000000000 ) ) ;
#33107 = APPROVAL_STATUS ( 'not_yet_approved' ) ;
#33108 = AXIS2_PLACEMENT_3D ( 'NONE', #28789, #4075, #26309 ) ;
#33109 = CARTESIAN_POINT ( 'NONE',  ( 0.3669024016988304271, -1.145827175174834123, 0.4338469531130782486 ) ) ;
#33110 = CARTESIAN_POINT ( 'NONE',  ( 0.03158843595483465383, -0.4819971762524432601, 0.09920191295802863185 ) ) ;
#33111 = FACE_OUTER_BOUND ( 'NONE', #8247, .T. ) ;
#33112 = VECTOR ( 'NONE', #28681, 39.37007874015748143 ) ;
#33113 = ADVANCED_FACE ( 'NONE', ( #28816 ), #2222, .F. ) ;
#33114 = CIRCLE ( 'NONE', #37723, 0.06000000000000021289 ) ;
#33115 = AXIS2_PLACEMENT_3D ( 'NONE', #39738, #33768, #30485 ) ;
#33116 = PRODUCT_DEFINITION_SHAPE ( 'NONE', 'NONE',  #40649 ) ;
#33117 = DIRECTION ( 'NONE',  ( 0.4999551463232372317, -0.8660512985181135770, 0.000000000000000000 ) ) ;
#33118 = CARTESIAN_POINT ( 'NONE',  ( 0.3695849881062516218, -1.765902858937650199, -0.5832748682907470394 ) ) ;
#33119 = EDGE_CURVE ( 'NONE', #29847, #37277, #16023, .T. ) ;
#33120 = CARTESIAN_POINT ( 'NONE',  ( -0.1142670043590668094, -0.4723146173917492918, 0.3382895567580812557 ) ) ;
#33121 = CARTESIAN_POINT ( 'NONE',  ( 0.03158843595483495220, 0.05459869295506127734, -0.4890616322892840651 ) ) ;
#33122 = VECTOR ( 'NONE', #7290, 39.37007874015748143 ) ;
#33123 = ORIENTED_EDGE ( 'NONE', *, *, #22536, .T. ) ;
#33124 = ORIENTED_EDGE ( 'NONE', *, *, #21002, .F. ) ;
#33125 = AXIS2_PLACEMENT_3D ( 'NONE', #5734, #30214, #36605 ) ;
#33126 = CARTESIAN_POINT ( 'NONE',  ( 0.3980468560452211646, -1.724211293688185487, 0.4257487098170510409 ) ) ;
#33127 = EDGE_LOOP ( 'NONE', ( #19781, #8577, #39456 ) ) ;
#33128 = CARTESIAN_POINT ( 'NONE',  ( 0.1499999999999996059, -0.2450655194479835486, -0.4674710490749285907 ) ) ;
#33129 = CARTESIAN_POINT ( 'NONE',  ( 0.1693691421777691608, -0.7003464674209329832, 0.4928941103632852871 ) ) ;
#33131 = ORIENTED_EDGE ( 'NONE', *, *, #21482, .F. ) ;
#33130 = CARTESIAN_POINT ( 'NONE',  ( 9.985549626383408877E-05, -0.6770222147840202487, -0.01371064749713882085 ) ) ;
#33132 = ORIENTED_EDGE ( 'NONE', *, *, #14836, .F. ) ;
#33133 = LINE ( 'NONE', #17693, #5409 ) ;
#33134 = VERTEX_POINT ( 'NONE', #3723 ) ;
#33135 = EDGE_CURVE ( 'NONE', #38375, #16750, #33817, .T. ) ;
#33136 = CARTESIAN_POINT ( 'NONE',  ( 0.2675939308526570914, -1.646160075673759993, 0.7657054049786949923 ) ) ;
#33138 = CARTESIAN_POINT ( 'NONE',  ( 0.5195836351326650338, -1.602777390882857533, -0.4212996487385544109 ) ) ;
#33137 = DIRECTION ( 'NONE',  ( 1.000000000000000000, 7.194105162071894010E-14, 7.847494366974321282E-16 ) ) ;
#33139 = CARTESIAN_POINT ( 'NONE',  ( 0.3534309663918363542, -1.740588291835677870, -0.3303540215336857044 ) ) ;
#33140 = EDGE_CURVE ( 'NONE', #4078, #5225, #31785, .T. ) ;
#33141 = APPROVAL_DATE_TIME ( #39925, #1494 ) ;
#33142 = CARTESIAN_POINT ( 'NONE',  ( 0.6985364634159124675, -1.438850461896725275, 0.5682400285031795617 ) ) ;
#33144 = ORIENTED_EDGE ( 'NONE', *, *, #3735, .F. ) ;
#33143 = ORIENTED_EDGE ( 'NONE', *, *, #6498, .T. ) ;
#33145 = EDGE_CURVE ( 'NONE', #17298, #28471, #16614, .T. ) ;
#33146 = AXIS2_PLACEMENT_3D ( 'NONE', #28806, #19741, #28997 ) ;
#33147 = CARTESIAN_POINT ( 'NONE',  ( 0.01163423095162381508, -0.7864269613462812059, -0.09388360016666105756 ) ) ;
#33148 = CARTESIAN_POINT ( 'NONE',  ( 0.1175647116005374415, -1.401988507280150120, 0.6256832329251384994 ) ) ;
#33149 = AXIS2_PLACEMENT_3D ( 'NONE', #16192, #4425, #29123 ) ;
#33150 = CARTESIAN_POINT ( 'NONE',  ( 0.1608696483632978125, -0.7559743210487993581, 0.5743405515187776089 ) ) ;
#33151 = AXIS2_PLACEMENT_3D ( 'NONE', #16260, #10675, #25516 ) ;
#33152 = CARTESIAN_POINT ( 'NONE',  ( 0.1161508510350168916, -0.5536193762935293083, 0.1892461907774328489 ) ) ;
#33153 = CARTESIAN_POINT ( 'NONE',  ( 0.3112311390139286815, -1.649331203103300059, -0.3389060930261176829 ) ) ;
#33154 = CARTESIAN_POINT ( 'NONE',  ( -2.128280327564064936E-14, -2.097675824466503691, -0.6968677163258657492 ) ) ;
#33155 = SECURITY_CLASSIFICATION ( '', '', #12328 ) ;
#33156 = CARTESIAN_POINT ( 'NONE',  ( 0.06517543881758507129, -1.341089537907319551, 0.5527912483730096360 ) ) ;
#33157 = CARTESIAN_POINT ( 'NONE',  ( 0.3854651929502717067, -1.696813303095609404, -0.4100924813245869216 ) ) ;
#33158 = CARTESIAN_POINT ( 'NONE',  ( 0.4048428100840241184, -1.714396146459797654, 0.4257347495283832495 ) ) ;
#33159 = VECTOR ( 'NONE', #11563, 39.37007874015748854 ) ;
#33160 = DIRECTION ( 'NONE',  ( -1.000000000000000000, -0.000000000000000000, -0.000000000000000000 ) ) ;
#33161 = DIRECTION ( 'NONE',  ( 0.000000000000000000, -0.8834504764630435325, 0.4685245517976845409 ) ) ;
#33162 = DIRECTION ( 'NONE',  ( 1.000000000000000000, 1.443840457432242888E-15, -8.250516899612815800E-16 ) ) ;
#33163 =( BOUNDED_SURFACE ( )  B_SPLINE_SURFACE ( 3, 2, ( 
 ( #13217, #34813, #3557 ),
 ( #19413, #16125, #28664 ),
 ( #34207, #532, #13029 ),
 ( #35020, #25784, #10138 ),
 ( #6018, #15510, #4362 ),
 ( #13426, #7042, #32743 ),
 ( #20013, #7226, #38520 ),
 ( #19611, #32946, #23319 ),
 ( #19796, #16922, #32144 ),
 ( #22710, #10352, #13625 ),
 ( #4749, #29052, #14235 ),
 ( #16512, #35242, #1119 ) ),
 .UNSPECIFIED., .F., .F., .F. ) 
 B_SPLINE_SURFACE_WITH_KNOTS ( ( 4, 2, 2, 2, 2, 4 ),
 ( 3, 3 ),
 ( 1.507041019754851163E-16, 0.0009292827807487099570, 0.001858565561497269210, 0.002323206951871548999, 0.002787848342245828354, 0.003717131122994387499 ),
 ( 0.000000000000000000, 1.000000000000000000 ),
 .UNSPECIFIED. ) 
 GEOMETRIC_REPRESENTATION_ITEM ( )  RATIONAL_B_SPLINE_SURFACE ( (
 ( 1.000000000000000000, 0.5022121722253957143, 1.000000000000000000),
 ( 1.000000000000000000, 0.5252469407714646099, 1.000000000000000000),
 ( 1.000000000000000000, 0.5463897451926625903, 1.000000000000000000),
 ( 1.000000000000000000, 0.5861329644067504452, 1.000000000000000000),
 ( 1.000000000000000000, 0.6040810576437375401, 1.000000000000000000),
 ( 1.000000000000000000, 0.6289914906242201065, 1.000000000000000000),
 ( 1.000000000000000000, 0.6370577570986643012, 1.000000000000000000),
 ( 1.000000000000000000, 0.6525045360464006849, 1.000000000000000000),
 ( 1.000000000000000000, 0.6598645560874571991, 1.000000000000000000),
 ( 1.000000000000000000, 0.6813382805142172982, 1.000000000000000000),
 ( 1.000000000000000000, 0.6952409275468639516, 1.000000000000000000),
 ( 1.000000000000000000, 0.7071067811865489050, 1.000000000000000000) ) ) 
 REPRESENTATION_ITEM ( '' )  SURFACE ( )  );
#33164 = CARTESIAN_POINT ( 'NONE',  ( 0.4534726104141680314, -1.109102898972393225, 0.5733675676254303966 ) ) ;
#33165 = LINE ( 'NONE', #24134, #20040 ) ;
#33166 = LENGTH_MEASURE_WITH_UNIT ( LENGTH_MEASURE( 0.02539999999999999897 ), #22917 );
#33167 = CARTESIAN_POINT ( 'NONE',  ( 0.6184088846978791354, -1.609314212450322357, -0.4711275932451951531 ) ) ;
#33168 = CARTESIAN_POINT ( 'NONE',  ( 0.1873045545006853108, -1.548079183614573306, 0.6123590530682133659 ) ) ;
#33169 = CARTESIAN_POINT ( 'NONE',  ( 0.3074110389119673048, -0.9534851582863556052, 0.5796648297427198226 ) ) ;
#33170 = COORDINATED_UNIVERSAL_TIME_OFFSET ( 0, 0, .AHEAD. ) ;
#33171 = CARTESIAN_POINT ( 'NONE',  ( 0.2256281918571345080, -0.6025195051315143102, 0.5087991896564706407 ) ) ;
#33172 = EDGE_CURVE ( 'NONE', #29483, #892, #37028, .T. ) ;
#33173 = TOROIDAL_SURFACE ( 'NONE', #13477, 0.04749999999977547877, 0.01000000000000000021 ) ;
#33174 = CARTESIAN_POINT ( 'NONE',  ( 0.3935098752428118352, -1.601833234276202056, -0.6187469409402625020 ) ) ;
#33175 = EDGE_CURVE ( 'NONE', #26668, #14931, #18753, .T. ) ;
#33176 = CARTESIAN_POINT ( 'NONE',  ( 0.04285427992853951124, 0.07198917448059898028, -0.4895546022328390312 ) ) ;
#33177 = AXIS2_PLACEMENT_3D ( 'NONE', #13498, #16577, #38582 ) ;
#33178 = EDGE_LOOP ( 'NONE', ( #29244, #25263, #25353, #36879 ) ) ;
#33179 = CARTESIAN_POINT ( 'NONE',  ( 0.4159916692016358830, -1.069406866067976081, -0.5155029497116575543 ) ) ;
#33180 = LOCAL_TIME ( 0, 53, 7.000000000000000000, #24886 ) ;
#33181 = CARTESIAN_POINT ( 'NONE',  ( 0.08045902273983134012, -0.9874980346209583093, 0.8248919155433931394 ) ) ;
#33182 = DIRECTION ( 'NONE',  ( 1.000000000000000000, 1.450080480853946466E-15, -8.359287477863926836E-16 ) ) ;
#33184 = ORIENTED_EDGE ( 'NONE', *, *, #38566, .F. ) ;
#33183 = CARTESIAN_POINT ( 'NONE',  ( 0.1626176757286639796, -0.6782218769987641283, 0.05683303076865411224 ) ) ;
#33185 = LINE ( 'NONE', #33381, #2204 ) ;
#33186 = CIRCLE ( 'NONE', #10851, 0.04330708661417343591 ) ;
#33187 = CARTESIAN_POINT ( 'NONE',  ( 0.5591717342432651616, -1.201875270489466407, 0.7301083282254506868 ) ) ;
#33189 = EDGE_LOOP ( 'NONE', ( #15393, #1654, #25642, #16036, #4568, #17200, #22143 ) ) ;
#33188 = ORIENTED_EDGE ( 'NONE', *, *, #4704, .F. ) ;
#33190 = CARTESIAN_POINT ( 'NONE',  ( 0.009551370979964050878, -1.736475153700349550, -0.6662139729480507366 ) ) ;
#33191 = ORIENTED_EDGE ( 'NONE', *, *, #18179, .F. ) ;
#33192 = CARTESIAN_POINT ( 'NONE',  ( 0.6620678144876760429, -1.446799780631947252, -0.4151272395384200675 ) ) ;
#33193 = CARTESIAN_POINT ( 'NONE',  ( 0.3484677573834971120, -1.177852168535778565, 0.4182417262808778013 ) ) ;
#33194 = COORDINATED_UNIVERSAL_TIME_OFFSET ( 0, 0, .AHEAD. ) ;
#33195 = DIRECTION ( 'NONE',  ( 1.000000000000000000, 0.000000000000000000, 0.000000000000000000 ) ) ;
#33196 = ORIENTED_EDGE ( 'NONE', *, *, #36675, .T. ) ;
#33197 = FACE_OUTER_BOUND ( 'NONE', #8136, .T. ) ;
#33198 = CARTESIAN_POINT ( 'NONE',  ( 0.09038474980893905497, -0.6484375426880288895, 0.2188470046619405418 ) ) ;
#33199 = CARTESIAN_POINT ( 'NONE',  ( 0.2982782193571763552, -1.650121741622242899, 0.9210486992908254456 ) ) ;
#33200 = CARTESIAN_POINT ( 'NONE',  ( 0.1070046036752630297, -0.6117146700487942068, 0.3554384173735813390 ) ) ;
#33202 = DIRECTION ( 'NONE',  ( 0.01265474379914247223, 0.8659329421511292590, -0.4999999971568669932 ) ) ;
#33201 = CARTESIAN_POINT ( 'NONE',  ( 0.1152231430944956614, -0.4481617324789591295, 0.1139065117562511747 ) ) ;
#33203 = CARTESIAN_POINT ( 'NONE',  ( 0.1516750352782837430, -1.012591555047931413, 0.5723390026005544806 ) ) ;
#33204 = EDGE_LOOP ( 'NONE', ( #18829, #9131, #16741, #13685 ) ) ;
#33205 = ORIENTED_EDGE ( 'NONE', *, *, #930, .T. ) ;
#33206 = VECTOR ( 'NONE', #2542, 39.37007874015748854 ) ;
#33207 = DIRECTION ( 'NONE',  ( 0.000000000000000000, -0.9901182710308955581, 0.1402348365092997984 ) ) ;
#33208 = CARTESIAN_POINT ( 'NONE',  ( 0.1890114826851027052, -0.4630349058840709797, 0.1881648106416238253 ) ) ;
#33209 = DIRECTION ( 'NONE',  ( 0.8660512985181135770, 0.4999551463232369541, 0.000000000000000000 ) ) ;
#33210 = CARTESIAN_POINT ( 'NONE',  ( 0.03309060444528783701, -0.4608881774262347242, 0.2425132784556429388 ) ) ;
#33211 = LOCAL_TIME ( 0, 53, 7.000000000000000000, #24739 ) ;
#33212 = CARTESIAN_POINT ( 'NONE',  ( -0.03877220711930347286, -0.4622141677842752649, -0.1152577684344557041 ) ) ;
#33213 = CARTESIAN_POINT ( 'NONE',  ( 0.08060092049549716364, -1.315521956732087716, 0.4779325244181578114 ) ) ;
#33214 = CARTESIAN_POINT ( 'NONE',  ( 0.4080314874273783254, -1.727341531470994562, -0.4910957289382530400 ) ) ;
#33215 = AXIS2_PLACEMENT_3D ( 'NONE', #26942, #39680, #33714 ) ;
#33216 = CARTESIAN_POINT ( 'NONE',  ( 0.3591498995103406533, -1.737620376665804933, -0.5147966178037263196 ) ) ;
#33217 = CARTESIAN_POINT ( 'NONE',  ( 0.3484275328463246058, -0.9131724924592886650, 0.6749714385622568313 ) ) ;
#33218 = CARTESIAN_POINT ( 'NONE',  ( -0.02000000000000000042, -1.910390638264138685, -0.8820407338378629669 ) ) ;
#33219 = CARTESIAN_POINT ( 'NONE',  ( 0.1995529058109158649, -2.050896138459939344, -0.3054326997595754878 ) ) ;
#33220 = DIRECTION ( 'NONE',  ( -1.000000000000000000, -0.000000000000000000, -0.000000000000000000 ) ) ;
#33221 = ORIENTED_EDGE ( 'NONE', *, *, #20111, .T. ) ;
#33222 = CARTESIAN_POINT ( 'NONE',  ( 0.4226803827459378327, -1.212955488335365706, 0.6549176275605582687 ) ) ;
#33223 = DIRECTION ( 'NONE',  ( 0.4999551463232372317, -0.8660512985181133550, 0.000000000000000000 ) ) ;
#33224 = DIRECTION ( 'NONE',  ( -1.000000000000000000, -2.280301054154495132E-31, 1.664003471950577689E-31 ) ) ;
#33225 = ORIENTED_EDGE ( 'NONE', *, *, #38663, .F. ) ;
#33226 = CARTESIAN_POINT ( 'NONE',  ( 0.2570033106424722824, -0.8827906082398013776, 0.5132624092235830160 ) ) ;
#33227 = DIRECTION ( 'NONE',  ( -0.8660512985181131329, -0.4999551463232375648, -0.000000000000000000 ) ) ;
#33228 = CLOSED_SHELL ( 'NONE', ( #538, #719, #29324, #39397, #31904, #31138, #21746, #16682, #25865, #27109, #23874, #32831, #16300, #32658, #2208, #18756, #27511, #4882, #24736, #16838, #4410, #5092, #23582, #2452, #11542, #12677, #40353, #36184, #5332, #31830, #5869, #22, #10690, #8623, #4097, #31527, #21582, #11195, #29934, #29612, #38672, #27598, #34111, #6404, #33760, #7951, #404, #7187, #15879, #11827, #30277, #22084, #32059, #24830, #40588, #39062, #20734, #31156, #27775, #29337, #37066, #3391, #24492, #6938, #5189, #5212, #27857, #35127, #10955, #23753, #26032, #27611, #12787, #9424, #32929, #37868, #15804, #20838, #28241, #40171, #15929, #12754, #16440, #30083, #12674, #26042 ) ) ;
#33229 = VECTOR ( 'NONE', #23160, 39.37007874015748143 ) ;
#33230 = CARTESIAN_POINT ( 'NONE',  ( 0.05896163446183822626, -0.9045474224942531283, 0.5580107087153096668 ) ) ;
#33231 = ORIENTED_EDGE ( 'NONE', *, *, #30108, .F. ) ;
#33232 = CARTESIAN_POINT ( 'NONE',  ( -0.03868264068766689295, 0.2522289290439786447, 0.4043438810462527955 ) ) ;
#33233 = CARTESIAN_POINT ( 'NONE',  ( 0.05561310505366609536, -0.02041094169099977318, 0.4604718309744721405 ) ) ;
#33234 = APPLIED_APPROVAL_ASSIGNMENT ( #25245, ( #39149 ) ) ;
#33235 = CARTESIAN_POINT ( 'NONE',  ( 0.03303737228521689412, -0.5155559760688823712, -0.07470078032051498396 ) ) ;
#33236 = CARTESIAN_POINT ( 'NONE',  ( 0.1793546593917179355, -1.785823421859094706, -0.3235890279080452236 ) ) ;
#33237 = CARTESIAN_POINT ( 'NONE',  ( 0.4562328291855674012, -1.220725676369126766, 0.6612685506176263495 ) ) ;
#33239 = DIRECTION ( 'NONE',  ( 0.000000000000000000, 0.000000000000000000, -1.000000000000000000 ) ) ;
#33238 = CARTESIAN_POINT ( 'NONE',  ( -0.3000000000000000999, -2.891403747035983240, -0.7012825271972917829 ) ) ;
#33240 = CARTESIAN_POINT ( 'NONE',  ( 0.5725052286446696836, -1.544230605290505931, -0.5333758322335983015 ) ) ;
#33241 = EDGE_LOOP ( 'NONE', ( #29682, #6987, #30105, #40305, #25107 ) ) ;
#33242 = CIRCLE ( 'NONE', #15515, 0.03000000000000006481 ) ;
#33243 = DIRECTION ( 'NONE',  ( 0.9378410757839558132, -0.2807814858886552578, 0.2039996905746457034 ) ) ;
#33244 = ORIENTED_EDGE ( 'NONE', *, *, #32785, .T. ) ;
#33245 = CARTESIAN_POINT ( 'NONE',  ( 0.1924928095266713046, -0.6407273034312881421, 0.1479976049341028554 ) ) ;
#33246 = CARTESIAN_POINT ( 'NONE',  ( 0.07850612262371522987, -0.6528207494238292830, 0.4497086622102388631 ) ) ;
#33248 = CARTESIAN_POINT ( 'NONE',  ( 0.000000000000000000, 0.000000000000000000, 0.000000000000000000 ) ) ;
#33247 = CARTESIAN_POINT ( 'NONE',  ( 0.7062175672384829461, -1.525603138082098686, 0.5668970561574433464 ) ) ;
#33249 = VERTEX_POINT ( 'NONE', #31304 ) ;
#33250 = CARTESIAN_POINT ( 'NONE',  ( -2.070754768975509474, -0.09959325338431655739, 0.08500000000000142164 ) ) ;
#33251 = CARTESIAN_POINT ( 'NONE',  ( 0.5737068280812576138, -1.499206715230487319, 0.5693098563960987679 ) ) ;
#33252 = ORIENTED_EDGE ( 'NONE', *, *, #13180, .F. ) ;
#33253 = CARTESIAN_POINT ( 'NONE',  ( 0.3273010810244016966, -1.767032151526223505, 0.5424958386988285586 ) ) ;
#33254 = CARTESIAN_POINT ( 'NONE',  ( 0.01899496522503697424, -0.4667215747137393733, 0.2292237458735815747 ) ) ;
#33255 = DIRECTION ( 'NONE',  ( -0.4999999999999991673, 0.000000000000000000, 0.8660254037844391517 ) ) ;
#33256 = CARTESIAN_POINT ( 'NONE',  ( 0.2162048916983708990, -1.230695052506779241, 0.4870512237330100191 ) ) ;
#33257 = CARTESIAN_POINT ( 'NONE',  ( 0.3969700875655671202, -1.750093955434230741, -0.5306525527941791109 ) ) ;
#33258 = DIRECTION ( 'NONE',  ( 0.000000000000000000, -0.5914787413272157846, -0.8063205929144887651 ) ) ;
#33259 = CIRCLE ( 'NONE', #30655, 0.1600000000000006140 ) ;
#33260 = CARTESIAN_POINT ( 'NONE',  ( 0.7227036224969136669, -1.477504586156484612, 0.6121051687398550989 ) ) ;
#33261 = CARTESIAN_POINT ( 'NONE',  ( 0.000000000000000000, 0.000000000000000000, 0.000000000000000000 ) ) ;
#33262 = CARTESIAN_POINT ( 'NONE',  ( 0.02869942827333502033, -0.3396431753871653192, -0.3648167270360652692 ) ) ;
#33263 = LOCAL_TIME ( 0, 53, 7.000000000000000000, #6414 ) ;
#33264 = CARTESIAN_POINT ( 'NONE',  ( 0.6028087430831944316, -1.593422650548542485, -0.5410972547399238719 ) ) ;
#33265 = CARTESIAN_POINT ( 'NONE',  ( 0.03171861681796823984, 0.2437378752574358431, 0.4645579091361449753 ) ) ;
#33266 = LINE ( 'NONE', #11859, #22129 ) ;
#33267 = CARTESIAN_POINT ( 'NONE',  ( 0.01548846960721252282, 0.3688619771570336159, -0.3775276577325234473 ) ) ;
#33268 = CIRCLE ( 'NONE', #15545, 0.1000000000000000194 ) ;
#33269 = CARTESIAN_POINT ( 'NONE',  ( -0.03654364704248880963, 0.4542255574219845049, -0.2354487068768210956 ) ) ;
#33270 = ADVANCED_FACE ( 'NONE', ( #69 ), #24050, .T. ) ;
#33271 = APPROVAL ( #19618, 'UNSPECIFIED' ) ;
#33272 = CARTESIAN_POINT ( 'NONE',  ( 0.1249840844849290228, -1.018512954913863844, 0.9570223520903572423 ) ) ;
#33273 = CARTESIAN_POINT ( 'NONE',  ( 0.5762035759104484622, -1.538322682916094308, -0.5547479506342967159 ) ) ;
#33274 = CARTESIAN_POINT ( 'NONE',  ( 0.4317026225184690813, -1.612351040652626466, -0.6637038356405958739 ) ) ;
#33275 = CARTESIAN_POINT ( 'NONE',  ( 0.5909188805876246509, -1.601585752074789148, 0.4182417262808776903 ) ) ;
#33276 = ORIENTED_EDGE ( 'NONE', *, *, #30362, .T. ) ;
#33277 = CARTESIAN_POINT ( 'NONE',  ( 0.3965913301904470112, -1.111811593118468666, 0.6217369508112339238 ) ) ;
#33278 = CARTESIAN_POINT ( 'NONE',  ( 0.4092450614235220163, -1.131740385117829817, 0.4687417262808780127 ) ) ;
#33279 = CARTESIAN_POINT ( 'NONE',  ( 0.05999999999999990757, 0.000000000000000000, 0.000000000000000000 ) ) ;
#33280 = CARTESIAN_POINT ( 'NONE',  ( 0.02953079040095673430, -0.5250338024619269905, -0.07436286310882420092 ) ) ;
#33281 = CARTESIAN_POINT ( 'NONE',  ( 0.5227806196671862526, -1.332469647702360094, 0.5985616508300974914 ) ) ;
#33283 = ORIENTED_EDGE ( 'NONE', *, *, #5147, .F. ) ;
#33282 = CARTESIAN_POINT ( 'NONE',  ( -0.05561176441985811458, 0.4316390549698259083, 0.1616802657107478947 ) ) ;
#33284 = CARTESIAN_POINT ( 'NONE',  ( 0.1843752803354802849, -0.7900634509218503743, 0.1457185332388700461 ) ) ;
#33285 = AXIS2_PLACEMENT_3D ( 'NONE', #2322, #20235, #24742 ) ;
#33286 = CARTESIAN_POINT ( 'NONE',  ( 0.5669405059600367558, -1.627145089617755058, 0.5182417262812432091 ) ) ;
#33287 = ORIENTED_EDGE ( 'NONE', *, *, #11779, .T. ) ;
#33288 = CARTESIAN_POINT ( 'NONE',  ( 0.3604126524395246944, -1.757925354409644925, -0.5278718762441512169 ) ) ;
#33289 = CARTESIAN_POINT ( 'NONE',  ( 0.2800739882076511700, -1.402756909172277577, 0.9018012001688786583 ) ) ;
#33291 = CARTESIAN_POINT ( 'NONE',  ( 0.1772207660457670864, -0.4584906788804246625, 0.1194733215096158291 ) ) ;
#33290 = CARTESIAN_POINT ( 'NONE',  ( 0.7078192764890761657, -1.501499620364393106, 0.5258185712464616968 ) ) ;
#33292 = DIRECTION ( 'NONE',  ( 1.000000000000000000, 6.779273404243070203E-32, 4.314083075427408311E-32 ) ) ;
#33293 = APPLIED_SECURITY_CLASSIFICATION_ASSIGNMENT ( #24771, ( #40661 ) ) ;
#33294 = CARTESIAN_POINT ( 'NONE',  ( 0.1371161371553715480, -1.302047841212754964, -0.3409434894749658329 ) ) ;
#33295 = ORIENTED_EDGE ( 'NONE', *, *, #20966, .T. ) ;
#33296 = AXIS2_PLACEMENT_3D ( 'NONE', #28197, #18523, #34360 ) ;
#33297 = ORIENTED_EDGE ( 'NONE', *, *, #15982, .T. ) ;
#33298 = LINE ( 'NONE', #5106, #39042 ) ;
#33299 = ADVANCED_FACE ( 'NONE', ( #1268 ), #32473, .F. ) ;
#33300 = CARTESIAN_POINT ( 'NONE',  ( 0.3699999999999786793, -2.097675824466503691, -0.5196396315034578217 ) ) ;
#33301 = CARTESIAN_POINT ( 'NONE',  ( 0.1013622771692264529, -0.8626241053983823015, 0.4561048637332515421 ) ) ;
#33302 = CARTESIAN_POINT ( 'NONE',  ( 0.3363290849198692367, -1.747766234461343604, 0.4536831844799349978 ) ) ;
#33303 = EDGE_CURVE ( 'NONE', #36573, #4130, #9490, .T. ) ;
#33304 = DIRECTION ( 'NONE',  ( -0.9390634835782838419, -0.2947238591715443667, 0.1769113355465114223 ) ) ;
#33305 = EDGE_CURVE ( 'NONE', #6106, #23675, #12115, .T. ) ;
#33306 = EDGE_CURVE ( 'NONE', #7581, #27128, #19977, .T. ) ;
#33307 = CARTESIAN_POINT ( 'NONE',  ( 0.3368016641934968303, -1.066382448447511289, 0.6377147322532498164 ) ) ;
#33308 = DIRECTION ( 'NONE',  ( 0.000000000000000000, 1.776356839400250465E-15, -1.000000000000000000 ) ) ;
#33309 = CARTESIAN_POINT ( 'NONE',  ( 0.04293317454820629736, 0.4432234940308290017, 0.2195257349118415469 ) ) ;
#33310 = CARTESIAN_POINT ( 'NONE',  ( -0.2399999999999999079, -2.945416957892569521, -0.4639726661791638840 ) ) ;
#33311 = CARTESIAN_POINT ( 'NONE',  ( -0.2299999999999999267, 0.5182417262804744906, 0.09999999999999989453 ) ) ;
#33312 = APPROVAL_DATE_TIME ( #5305, #31049 ) ;
#33313 = AXIS2_PLACEMENT_3D ( 'NONE', #32112, #23070, #29234 ) ;
#33314 = CARTESIAN_POINT ( 'NONE',  ( 0.3590698163857336533, -1.160211858102977445, 0.4287992454472202009 ) ) ;
#33315 = CARTESIAN_POINT ( 'NONE',  ( 0.5624624041831085552, -1.181422097061986864, 0.6057417262809811076 ) ) ;
#33316 = DIRECTION ( 'NONE',  ( 1.000000000000000000, 0.000000000000000000, 0.000000000000000000 ) ) ;
#33317 = ADVANCED_FACE ( 'NONE', ( #39083 ), #10140, .T. ) ;
#33318 = CARTESIAN_POINT ( 'NONE',  ( 0.01189099588732479666, -0.5490168688727182777, -0.07334142730708625990 ) ) ;
#33319 = CARTESIAN_POINT ( 'NONE',  ( 0.3920598280443489680, -1.752928556019227591, -0.5830366350881619475 ) ) ;
#33320 = CARTESIAN_POINT ( 'NONE',  ( 0.1043520668920405597, -0.9555303118660302131, 0.9080984478619723577 ) ) ;
#33321 = DIRECTION ( 'NONE',  ( -0.3468893892380672250, 0.2594111197898656962, -0.9013177145509837507 ) ) ;
#33322 = ORIENTED_EDGE ( 'NONE', *, *, #16515, .T. ) ;
#33323 = ORIENTED_EDGE ( 'NONE', *, *, #24480, .F. ) ;
#33324 = LINE ( 'NONE', #5130, #25667 ) ;
#33325 = ORIENTED_EDGE ( 'NONE', *, *, #4281, .T. ) ;
#33326 = DIRECTION ( 'NONE',  ( 0.4999551463232372317, -0.8660512985181135770, 0.000000000000000000 ) ) ;
#33327 = DIRECTION ( 'NONE',  ( 1.000000000000000000, -0.000000000000000000, -0.000000000000000000 ) ) ;
#33329 = ORIENTED_EDGE ( 'NONE', *, *, #37441, .F. ) ;
#33328 = CARTESIAN_POINT ( 'NONE',  ( 0.008960703219233765240, -0.6168145289279985954, 0.004056642792912171745 ) ) ;
#33330 = ORIENTED_EDGE ( 'NONE', *, *, #23245, .T. ) ;
#33331 = CARTESIAN_POINT ( 'NONE',  ( 0.3082516761123384463, -1.189542454948390615, 0.5190639696864913777 ) ) ;
#33332 = VERTEX_POINT ( 'NONE', #7799 ) ;
#33333 = CARTESIAN_POINT ( 'NONE',  ( -0.001584010976415890478, -0.5275152449236482077, 0.1550235232006954844 ) ) ;
#33335 = CARTESIAN_POINT ( 'NONE',  ( 0.5313892105359160345, -1.599996326799270951, -0.4392153793885997248 ) ) ;
#33334 = CARTESIAN_POINT ( 'NONE',  ( -0.04155248107635943489, -0.4523094957185400666, -0.1288470070525131739 ) ) ;
#33336 = CARTESIAN_POINT ( 'NONE',  ( 0.6312476157716652159, -1.614849939179139993, -0.4878779670507682464 ) ) ;
#33337 = PERSON_AND_ORGANIZATION_ROLE ( 'classification_officer' ) ;
#33338 = CARTESIAN_POINT ( 'NONE',  ( -0.1617138679863628359, 0.4681656832120535405, 0.3382895567580768703 ) ) ;
#33340 = ORIENTED_EDGE ( 'NONE', *, *, #26556, .F. ) ;
#33339 = ORIENTED_EDGE ( 'NONE', *, *, #28582, .T. ) ;
#33341 = FACE_OUTER_BOUND ( 'NONE', #24372, .T. ) ;
#33342 = DIRECTION ( 'NONE',  ( 0.000000000000000000, 0.000000000000000000, 1.000000000000000000 ) ) ;
#33343 = PRODUCT_DEFINITION_SHAPE ( 'NONE', 'NONE',  #7895 ) ;
#33344 = EDGE_CURVE ( 'NONE', #30897, #25449, #20369, .T. ) ;
#33345 = CARTESIAN_POINT ( 'NONE',  ( 0.1546160709011058509, -0.7880494215839132233, 0.6157047316182207020 ) ) ;
#33346 = CARTESIAN_POINT ( 'NONE',  ( 0.1864468077516607813, -0.7589597239772698511, 0.04357516743049526936 ) ) ;
#33347 = CARTESIAN_POINT ( 'NONE',  ( -6.834804016303107315E-15, -2.091147721901837286, -0.7263522089647810320 ) ) ;
#33348 = CARTESIAN_POINT ( 'NONE',  ( 0.3331689678465135640, -1.752618680477372015, -0.5145915016017981181 ) ) ;
#33349 = EDGE_CURVE ( 'NONE', #32833, #2287, #13429, .T. ) ;
#33350 = CARTESIAN_POINT ( 'NONE',  ( 0.3696071792890020524, -1.752960286906630527, -0.4262381047308068660 ) ) ;
#33351 = DIRECTION ( 'NONE',  ( 0.9998941247116546194, -0.01455087607601020239, 0.0001066420868422379362 ) ) ;
#33352 = EDGE_CURVE ( 'NONE', #4242, #15491, #29826, .T. ) ;
#33353 = AXIS2_PLACEMENT_3D ( 'NONE', #6562, #3099, #15642 ) ;
#33354 = DIRECTION ( 'NONE',  ( 0.000000000000000000, -3.330669073875470114E-16, -1.000000000000000000 ) ) ;
#33355 = CARTESIAN_POINT ( 'NONE',  ( 0.1625982857068778153, -0.6782215948270849948, 0.2386756342038218459 ) ) ;
#33356 = CARTESIAN_POINT ( 'NONE',  ( -0.1211772861969197951, -0.5069185045468647122, 0.1468025672055963127 ) ) ;
#33357 = CARTESIAN_POINT ( 'NONE',  ( 0.4104553069130719711, -1.122406575547196361, 0.6026975231386706433 ) ) ;
#33358 = DIRECTION ( 'NONE',  ( -0.8660512985181134660, -0.4999551463232372317, -0.000000000000000000 ) ) ;
#33359 =( NAMED_UNIT ( * ) PLANE_ANGLE_UNIT ( ) SI_UNIT ( $, .RADIAN. ) );
#33360 = CARTESIAN_POINT ( 'NONE',  ( -0.2666757540196706411, 0.4921670437878968851, 0.08500000000000004774 ) ) ;
#33361 = CARTESIAN_POINT ( 'NONE',  ( 0.1023011615166706662, -1.050388104772951969, 0.8771683563204210055 ) ) ;
#33362 = CARTESIAN_POINT ( 'NONE',  ( 0.4678749147552476173, -1.068959612060700115, 0.6229948197350051453 ) ) ;
#33363 = CARTESIAN_POINT ( 'NONE',  ( 0.06469670161903409711, -1.338666824997349236, 0.5872657038676230012 ) ) ;
#33364 = DATE_AND_TIME ( #37458, #37174 ) ;
#33365 = CARTESIAN_POINT ( 'NONE',  ( 0.1875419504463087250, -0.4620869884079685241, 0.1831780322516418646 ) ) ;
#33366 = EDGE_CURVE ( 'NONE', #27977, #7075, #25233, .T. ) ;
#33367 = ADVANCED_FACE ( 'NONE', ( #33103 ), #4507, .T. ) ;
#33368 = EDGE_CURVE ( 'NONE', #30000, #14919, #17570, .T. ) ;
#33369 = EDGE_CURVE ( 'NONE', #26070, #5313, #35097, .T. ) ;
#33370 = CARTESIAN_POINT ( 'NONE',  ( 0.3544525855955824589, -1.628498139902171848, -0.6593841416021899438 ) ) ;
#33371 = CARTESIAN_POINT ( 'NONE',  ( 0.03170953572518742797, 0.05433194795445773356, -0.4888234031312626016 ) ) ;
#33372 = ADVANCED_BREP_SHAPE_REPRESENTATION ( '', ( #19265, #27819 ), #3510 ) ;
#33373 = EDGE_CURVE ( 'NONE', #35103, #11876, #35740, .T. ) ;
#33374 = ORIENTED_EDGE ( 'NONE', *, *, #4170, .F. ) ;
#33375 = CARTESIAN_POINT ( 'NONE',  ( 0.3579995238153922399, -1.735700120908051147, -0.5200972866788388105 ) ) ;
#33376 = CARTESIAN_POINT ( 'NONE',  ( 0.008477321368347218514, -0.6246571256772747160, 0.4284521230191858931 ) ) ;
#33377 = CARTESIAN_POINT ( 'NONE',  ( 0.4947650380838903850, -1.353202518180897318, 0.8084467676771096567 ) ) ;
#33378 = CARTESIAN_POINT ( 'NONE',  ( 0.3111947872004536819, -1.649353374317168441, 0.4306238479843111366 ) ) ;
#33380 = EDGE_LOOP ( 'NONE', ( #17701, #208, #36366, #6549 ) ) ;
#33379 = CARTESIAN_POINT ( 'NONE',  ( 0.3875836258550495184, -1.829270650397434306, -0.5020249712731550407 ) ) ;
#33381 = CARTESIAN_POINT ( 'NONE',  ( -0.2746410161513779258, -2.423474325126674156, -0.5576739111151495232 ) ) ;
#33382 = CARTESIAN_POINT ( 'NONE',  ( 0.6181559592477333664, -1.299230524387357866, 0.5730398182776358373 ) ) ;
#33384 = ORIENTED_EDGE ( 'NONE', *, *, #33510, .F. ) ;
#33383 = VERTEX_POINT ( 'NONE', #27553 ) ;
#33385 = CARTESIAN_POINT ( 'NONE',  ( 0.02978343732698200338, -2.020922945396928849, -0.7048595805910107259 ) ) ;
#33386 = VERTEX_POINT ( 'NONE', #12119 ) ;
#33387 = DIRECTION ( 'NONE',  ( -1.000000000000000000, -2.341930812374887555E-31, 1.664003471950578127E-31 ) ) ;
#33388 = CARTESIAN_POINT ( 'NONE',  ( 0.4650894839780398415, -1.233502665152375721, 0.6057417262809881020 ) ) ;
#33389 = PERSON_AND_ORGANIZATION ( #35352, #36526 ) ;
#33390 = DIRECTION ( 'NONE',  ( 1.000000000000000000, 0.000000000000000000, 0.000000000000000000 ) ) ;
#33391 = VERTEX_POINT ( 'NONE', #39678 ) ;
#33392 = CARTESIAN_POINT ( 'NONE',  ( 0.1692070155042805502, -1.239154833823281621, 0.5978573722032971549 ) ) ;
#33393 = CARTESIAN_POINT ( 'NONE',  ( 0.08699155097204941400, -0.7258079871161503549, 0.1901423733659434456 ) ) ;
#33394 = CARTESIAN_POINT ( 'NONE',  ( 0.2714330136670746185, -1.557485186306450942, 0.9773871042817656729 ) ) ;
#33395 = CARTESIAN_POINT ( 'NONE',  ( 0.4988887069359189685, -1.539164871451035976, 0.6394187024492539173 ) ) ;
#33397 = DIRECTION ( 'NONE',  ( -1.000000000000000000, -7.857794173099924470E-32, -8.628166150854818811E-32 ) ) ;
#33396 = CARTESIAN_POINT ( 'NONE',  ( 0.3390251969953095301, -1.754624289129053993, 0.4617338307200986591 ) ) ;
#33398 = CARTESIAN_POINT ( 'NONE',  ( 0.01562499999999997571, -0.9454337353465637195, 0.1457185332388702959 ) ) ;
#33399 = ORIENTED_EDGE ( 'NONE', *, *, #40116, .F. ) ;
#33400 = ORIENTED_EDGE ( 'NONE', *, *, #27552, .T. ) ;
#33401 = ADVANCED_FACE ( 'NONE', ( #36789 ), #17589, .F. ) ;
#33402 = DIRECTION ( 'NONE',  ( 1.000000000000000000, 2.341930812374887555E-31, -1.664003471950578127E-31 ) ) ;
#33403 = CARTESIAN_POINT ( 'NONE',  ( 0.3275534972937365064, -0.8611932717542801763, 0.6716240152411563358 ) ) ;
#33404 = ADVANCED_FACE ( 'NONE', ( #24080 ), #39026, .T. ) ;
#33405 = CARTESIAN_POINT ( 'NONE',  ( 0.4291849790131893050, -1.119523916798046859, -0.6481113851292223949 ) ) ;
#33406 = LINE ( 'NONE', #37103, #2851 ) ;
#33407 = CARTESIAN_POINT ( 'NONE',  ( 0.02953079040095728247, 0.000000000000000000, 0.000000000000000000 ) ) ;
#33408 = CARTESIAN_POINT ( 'NONE',  ( -0.3000000000000000999, -4.250025578259899461, -0.8852376261118949374 ) ) ;
#33409 = CARTESIAN_POINT ( 'NONE',  ( 0.1909286924077254199, -1.257064795538238577, -0.7137147910238503812 ) ) ;
#33410 = FACE_OUTER_BOUND ( 'NONE', #13568, .T. ) ;
#33411 = CARTESIAN_POINT ( 'NONE',  ( 0.2882448896600493526, -0.8342145444298804113, 0.5948296420995525802 ) ) ;
#33412 = APPLICATION_PROTOCOL_DEFINITION ( 'international standard', 'automotive_design', 2000, #38439 ) ;
#33413 = FACE_OUTER_BOUND ( 'NONE', #19384, .T. ) ;
#33414 = CARTESIAN_POINT ( 'NONE',  ( -2.112273405726188513E-14, -2.183180860297921466, -0.2737760292030870235 ) ) ;
#33415 = CARTESIAN_POINT ( 'NONE',  ( 0.3686425856813914104, -2.055607201583817378, -0.5118490229217781406 ) ) ;
#33416 = ORIENTED_EDGE ( 'NONE', *, *, #15503, .F. ) ;
#33417 = EDGE_CURVE ( 'NONE', #40610, #31712, #18293, .T. ) ;
#33418 = CARTESIAN_POINT ( 'NONE',  ( 1.694818351060767277E-32, -2.632527843410151064E-17, -0.1249999999999999584 ) ) ;
#33419 = CARTESIAN_POINT ( 'NONE',  ( -0.05634304521267782806, -2.731847993664263218E-15, -0.4588823192046729837 ) ) ;
#33420 = CARTESIAN_POINT ( 'NONE',  ( -0.05078493045284371288, -0.3164574661091665853, -0.3525385122722523024 ) ) ;
#33421 = EDGE_CURVE ( 'NONE', #15168, #38375, #35204, .T. ) ;
#33422 = VERTEX_POINT ( 'NONE', #8409 ) ;
#33423 = FACE_OUTER_BOUND ( 'NONE', #21987, .T. ) ;
#33424 = PLANE ( 'NONE',  #35758 ) ;
#33425 = CARTESIAN_POINT ( 'NONE',  ( 0.05616483301611079754, -0.8972638835280528635, 0.5395877283156539361 ) ) ;
#33426 = ORIENTED_EDGE ( 'NONE', *, *, #22503, .F. ) ;
#33427 = CARTESIAN_POINT ( 'NONE',  ( 0.3245308759113119113, -1.295391163961464365, 0.5682442948123348492 ) ) ;
#33428 = CARTESIAN_POINT ( 'NONE',  ( 0.05634206451479407962, 0.01034894336415898355, 0.4588844674656195610 ) ) ;
#33429 = CARTESIAN_POINT ( 'NONE',  ( 0.04285427992854141249, -0.4433482162102910240, -0.2197464652568942856 ) ) ;
#33430 = DIRECTION ( 'NONE',  ( 1.000000000000000000, 0.000000000000000000, 0.000000000000000000 ) ) ;
#33431 = CARTESIAN_POINT ( 'NONE',  ( 0.4176213340141963770, -1.167371637102367687, 0.6772357243189727205 ) ) ;
#33433 = PLANE ( 'NONE',  #29951 ) ;
#33432 = DIRECTION ( 'NONE',  ( 0.8308509739180691689, 0.4796346601509333119, 0.2822007298383447660 ) ) ;
#33434 = CARTESIAN_POINT ( 'NONE',  ( -0.2746410161513776482, -3.730063144961804245, -0.1064410973704724706 ) ) ;
#33435 = VERTEX_POINT ( 'NONE', #12324 ) ;
#33436 = ORIENTED_EDGE ( 'NONE', *, *, #28577, .F. ) ;
#33437 = LINE ( 'NONE', #36931, #16523 ) ;
#33438 = EDGE_LOOP ( 'NONE', ( #18108, #38230, #14657, #24246, #14595, #1534, #20382, #300, #2646, #37248, #24605, #30012, #3788, #39794 ) ) ;
#33439 = CARTESIAN_POINT ( 'NONE',  ( 0.1893217774032603107, -0.5477411782657776174, 0.008518417185872213804 ) ) ;
#33440 = CARTESIAN_POINT ( 'NONE',  ( 0.06689121793234006907, -0.5986300435503874029, 0.3429109681586494096 ) ) ;
#33442 = CARTESIAN_POINT ( 'NONE',  ( 0.4291849790131893050, -1.119523916798046859, -0.6481113851292223949 ) ) ;
#33441 = CARTESIAN_POINT ( 'NONE',  ( 0.06863494493474814329, -0.5581937468183988393, 0.07394117948283039643 ) ) ;
#33443 = CARTESIAN_POINT ( 'NONE',  ( 0.5842233870797494122, -1.491766587394369736, 0.4817266676845166629 ) ) ;
#33444 = ORIENTED_EDGE ( 'NONE', *, *, #2953, .T. ) ;
#33445 = EDGE_CURVE ( 'NONE', #20959, #14789, #37736, .T. ) ;
#33446 = DIRECTION ( 'NONE',  ( 1.000000000000000000, 1.113825344428167933E-31, -7.771561172376107616E-16 ) ) ;
#33447 = CARTESIAN_POINT ( 'NONE',  ( 0.3604753679111668552, -1.128369292247676903, 0.8103591614715777158 ) ) ;
#33448 = DIRECTION ( 'NONE',  ( 0.000000000000000000, 0.000000000000000000, 1.000000000000000000 ) ) ;
#33449 = DIRECTION ( 'NONE',  ( 0.000000000000000000, 0.000000000000000000, -1.000000000000000000 ) ) ;
#33450 = CARTESIAN_POINT ( 'NONE',  ( 0.6372068045576322337, -1.562167934798605939, 0.4182417262808776903 ) ) ;
#33451 = PRODUCT ( 'pulley screw_short', 'pulley screw_short', '', ( #13724 ) ) ;
#33452 = CARTESIAN_POINT ( 'NONE',  ( 0.1522398948605527824, -1.279186700788397024, 0.4305827652437771436 ) ) ;
#33453 = DIRECTION ( 'NONE',  ( 1.000000000000000000, 6.779273404243070203E-32, 4.314083075427408311E-32 ) ) ;
#33454 = CARTESIAN_POINT ( 'NONE',  ( 0.3812071769896454021, -1.763750790280050440, -0.4536492913030992780 ) ) ;
#33455 = CARTESIAN_POINT ( 'NONE',  ( 0.2170862770790429608, -0.5809856703168675418, 0.4747658466717744608 ) ) ;
#33456 = DIRECTION ( 'NONE',  ( 1.000000000000000000, 1.517693329813464577E-15, -1.517693329813464577E-15 ) ) ;
#33457 = CARTESIAN_POINT ( 'NONE',  ( 0.0009067107390556438567, -0.9454806478692553418, 0.3203524331525413604 ) ) ;
#33458 = CARTESIAN_POINT ( 'NONE',  ( 0.6021587300967877754, -1.594267875390501299, -0.4941518814792995040 ) ) ;
#33459 = CARTESIAN_POINT ( 'NONE',  ( 0.6290530482886385055, -1.474716711548147874, 0.5182417262812423209 ) ) ;
#33460 = DIRECTION ( 'NONE',  ( -1.000000000000000000, -0.000000000000000000, -0.000000000000000000 ) ) ;
#33461 = CARTESIAN_POINT ( 'NONE',  ( 0.6984807982178791175, -1.438753897344778432, 0.5682417262808779901 ) ) ;
#33462 = CARTESIAN_POINT ( 'NONE',  ( -0.2399999999999999079, -2.289343986263487896, -0.7686455968847020204 ) ) ;
#33463 = CARTESIAN_POINT ( 'NONE',  ( -6.552157794917040043E-17, -0.4262518876079541830, 0.1106581735831166785 ) ) ;
#33464 = CARTESIAN_POINT ( 'NONE',  ( 0.5483671017596566388, -1.512491453477940784, 0.5432759641508111415 ) ) ;
#33465 = DIRECTION ( 'NONE',  ( 0.000000000000000000, 0.000000000000000000, -1.000000000000000000 ) ) ;
#33466 = ADVANCED_FACE ( 'NONE', ( #20976 ), #36415, .T. ) ;
#33467 = CARTESIAN_POINT ( 'NONE',  ( 0.5908959048872565178, -1.601544548465854145, 0.4282886817583845818 ) ) ;
#33468 = ORIENTED_EDGE ( 'NONE', *, *, #14177, .F. ) ;
#33469 = CARTESIAN_POINT ( 'NONE',  ( 0.4313479286575270244, -1.111437664270688241, 0.6062354644816806415 ) ) ;
#33470 = CARTESIAN_POINT ( 'NONE',  ( 0.3752269303716003757, -1.114063827499609305, 0.6058347348966837131 ) ) ;
#33471 = DIRECTION ( 'NONE',  ( 1.000000000000000000, 1.138269997360102476E-15, -8.881784197001243449E-16 ) ) ;
#33472 = CARTESIAN_POINT ( 'NONE',  ( -0.2043922129835731294, -0.5166151207188712791, 0.3750000000000001110 ) ) ;
#33473 = CARTESIAN_POINT ( 'NONE',  ( 0.3873111840515663373, -1.130537909310332489, 0.7530708704260813402 ) ) ;
#33475 = ORIENTED_EDGE ( 'NONE', *, *, #16230, .F. ) ;
#33474 = CARTESIAN_POINT ( 'NONE',  ( -0.02000000000000000042, -2.196071624283071788, -1.002400088386023791 ) ) ;
#33476 = CARTESIAN_POINT ( 'NONE',  ( 0.4898164652207312453, -1.090206986453526872, 0.6335228833721541220 ) ) ;
#33477 = ORIENTED_EDGE ( 'NONE', *, *, #40140, .T. ) ;
#33478 = CARTESIAN_POINT ( 'NONE',  ( 0.1870594268264934579, -1.259298449876196546, -0.3210044779109010871 ) ) ;
#33479 = ORIENTED_EDGE ( 'NONE', *, *, #21830, .T. ) ;
#33480 = CARTESIAN_POINT ( 'NONE',  ( 0.3316932917563030214, -1.670249455300529373, -0.6321824137348459605 ) ) ;
#33481 = EDGE_LOOP ( 'NONE', ( #39349, #29036, #37806, #4380 ) ) ;
#33482 = CARTESIAN_POINT ( 'NONE',  ( 0.3533442921551203653, -1.594940975894655111, 0.7477099863953585723 ) ) ;
#33484 = CARTESIAN_POINT ( 'NONE',  ( 0.1769134874695769410, -0.4794902306152409865, 0.04633223984654367966 ) ) ;
#33483 = CARTESIAN_POINT ( 'NONE',  ( 0.6671001712924167215, -1.531666483480435215, 0.4356495569555794423 ) ) ;
#33485 = CARTESIAN_POINT ( 'NONE',  ( 1.997133008241153135E-16, 0.2981948553318907180, 0.06819284191469529577 ) ) ;
#33486 = VERTEX_POINT ( 'NONE', #30433 ) ;
#33487 = EDGE_LOOP ( 'NONE', ( #32409, #10284 ) ) ;
#33488 = DIRECTION ( 'NONE',  ( 0.8660512985181134660, 0.4999551463232372872, 0.000000000000000000 ) ) ;
#33489 = DIRECTION ( 'NONE',  ( 0.9591734532964094617, 0.2828184691483933699, 5.691349986800551823E-16 ) ) ;
#33490 = CARTESIAN_POINT ( 'NONE',  ( 0.3263515015897640037, -1.281719106140628117, 0.6270899215385365988 ) ) ;
#33491 = CARTESIAN_POINT ( 'NONE',  ( -0.2746410161513782033, -2.294529520598973082, -0.6534431116140350104 ) ) ;
#33492 = CARTESIAN_POINT ( 'NONE',  ( 0.1890965627226634804, -1.347655541994686068, 0.5182417262812423209 ) ) ;
#33493 = CARTESIAN_POINT ( 'NONE',  ( 0.01548846960721238578, -0.2450655194478977839, -0.4674710490746283864 ) ) ;
#33494 = CARTESIAN_POINT ( 'NONE',  ( 0.3943456310756559002, -1.717985633627846287, 0.3157417262808776548 ) ) ;
#33495 =( BOUNDED_SURFACE ( )  B_SPLINE_SURFACE ( 3, 2, ( 
 ( #29465, #35429, #3948 ),
 ( #4748, #39325, #36035 ),
 ( #20011, #35841, #29877 ),
 ( #14233, #16510, #10743 ) ),
 .UNSPECIFIED., .F., .F., .F. ) 
 B_SPLINE_SURFACE_WITH_KNOTS ( ( 4, 4 ),
 ( 3, 3 ),
 ( -8.673617379884035472E-19, 0.002131800461895017127 ),
 ( 0.2677726292740011393, 0.6617067281966368952 ),
 .UNSPECIFIED. ) 
 GEOMETRIC_REPRESENTATION_ITEM ( )  RATIONAL_B_SPLINE_SURFACE ( (
 ( 0.8842712169365705144, 0.8302746405399135110, 0.8678740401095079715),
 ( 0.8848617173956563331, 0.8311406558908633890, 0.8685482063619062165),
 ( 0.8851481433175512059, 0.8315607220253672383, 0.8688752148974330236),
 ( 0.8851445905748156484, 0.8315555116488135834, 0.8688711587799162750) ) ) 
 REPRESENTATION_ITEM ( '' )  SURFACE ( )  );
#33496 = DIRECTION ( 'NONE',  ( -0.000000000000000000, 0.3090169943749569437, 0.9510565162951504226 ) ) ;
#33497 = CYLINDRICAL_SURFACE ( 'NONE', #18096, 0.04330708661417322775 ) ;
#33498 = CARTESIAN_POINT ( 'NONE',  ( 0.006497850577614296130, -0.9898846675935381034, 0.4770811589384994500 ) ) ;
#33499 = PRODUCT_CONTEXT ( 'NONE', #12985, 'mechanical' ) ;
#33500 = CARTESIAN_POINT ( 'NONE',  ( 0.4878678730304148448, -1.127350573924966071, 0.5059297001645776115 ) ) ;
#33501 = CARTESIAN_POINT ( 'NONE',  ( 0.01895884884825056391, -0.4667865995382994293, 0.2292744456225715155 ) ) ;
#33502 = DIRECTION ( 'NONE',  ( -0.1858595909941333224, -0.1072932506077245995, 0.9767007580674449407 ) ) ;
#33503 = CARTESIAN_POINT ( 'NONE',  ( 0.0001552339697111116302, -0.5543275554542274053, -0.06489989973435746073 ) ) ;
#33504 = FACE_OUTER_BOUND ( 'NONE', #39560, .T. ) ;
#33505 = FACE_OUTER_BOUND ( 'NONE', #29230, .T. ) ;
#33506 = VECTOR ( 'NONE', #35808, 39.37007874015748143 ) ;
#33507 = CARTESIAN_POINT ( 'NONE',  ( 0.01548846960712797240, -0.07651041855115535417, -0.5222379212567069828 ) ) ;
#33508 = EDGE_CURVE ( 'NONE', #38131, #33071, #33726, .T. ) ;
#33509 = VERTEX_POINT ( 'NONE', #24269 ) ;
#33510 = EDGE_CURVE ( 'NONE', #7743, #4952, #3071, .T. ) ;
#33511 = ORIENTED_EDGE ( 'NONE', *, *, #26995, .T. ) ;
#33512 = AXIS2_PLACEMENT_3D ( 'NONE', #5753, #33732, #11924 ) ;
#33513 = CARTESIAN_POINT ( 'NONE',  ( 0.3484677573834994435, -1.177852168535778565, 0.4182417262808778013 ) ) ;
#33514 = ORIENTED_EDGE ( 'NONE', *, *, #17594, .F. ) ;
#33515 = DIRECTION ( 'NONE',  ( 0.8660512985181135770, 0.4999551463232372317, 0.000000000000000000 ) ) ;
#33516 = EDGE_CURVE ( 'NONE', #17214, #32251, #1407, .T. ) ;
#33517 = DIRECTION ( 'NONE',  ( -0.8660254037844427044, -0.4079706259167306115, -0.2890674114961839236 ) ) ;
#33519 = EDGE_LOOP ( 'NONE', ( #39464, #346, #4729, #34515, #39831 ) ) ;
#33518 = CARTESIAN_POINT ( 'NONE',  ( 0.009380176198049450589, -0.5822127350993825390, 0.02749488402267697210 ) ) ;
#33520 = EDGE_CURVE ( 'NONE', #22416, #2187, #18688, .T. ) ;
#33521 = ORIENTED_EDGE ( 'NONE', *, *, #21065, .T. ) ;
#33522 = CYLINDRICAL_SURFACE ( 'NONE', #13969, 0.2149999999999999967 ) ;
#33523 = ORIENTED_EDGE ( 'NONE', *, *, #3166, .T. ) ;
#33524 = CARTESIAN_POINT ( 'NONE',  ( 0.03758983668052903043, -0.7652432842712353356, 0.6299102424528236766 ) ) ;
#33526 = CARTESIAN_POINT ( 'NONE',  ( 0.4996500228059882476, -1.606261977825028442, -0.4006985388676789217 ) ) ;
#33525 = CARTESIAN_POINT ( 'NONE',  ( -0.01895494625228063071, -0.5124113341948476341, -0.08888305413160664525 ) ) ;
#33527 = CARTESIAN_POINT ( 'NONE',  ( -0.2399999999999999079, -3.268524983732796318, -0.6433364877554561545 ) ) ;
#33528 = COORDINATED_UNIVERSAL_TIME_OFFSET ( 0, 0, .AHEAD. ) ;
#33529 = CARTESIAN_POINT ( 'NONE',  ( 0.5382312210666780894, -1.161160286399032238, 0.5682417267075779987 ) ) ;
#33531 = ORIENTED_EDGE ( 'NONE', *, *, #10922, .F. ) ;
#33530 = ORIENTED_EDGE ( 'NONE', *, *, #15583, .F. ) ;
#33532 = CARTESIAN_POINT ( 'NONE',  ( 0.02999999999997886302, -2.183180860297921466, -0.2737760292030870235 ) ) ;
#33533 = CARTESIAN_POINT ( 'NONE',  ( 0.2163934667642251342, -1.230460931614065112, 0.5491515737641515793 ) ) ;
#33534 = CARTESIAN_POINT ( 'NONE',  ( 0.3370383036578078473, -1.050006858144904909, 0.7785456481707841991 ) ) ;
#33535 = CARTESIAN_POINT ( 'NONE',  ( 0.1874330190944655250, -0.6911990066440627523, 0.04234871480744431538 ) ) ;
#33536 = ADVANCED_FACE ( 'NONE', ( #34318 ), #6131, .F. ) ;
#33537 = DIRECTION ( 'NONE',  ( 0.4999551463232372317, -0.8660512985181134660, 0.000000000000000000 ) ) ;
#33538 = CARTESIAN_POINT ( 'NONE',  ( 0.5446897993962578344, -1.168310332749241898, 0.4402873239467990918 ) ) ;
#33539 = APPLIED_PERSON_AND_ORGANIZATION_ASSIGNMENT ( #26493, #29170, ( #19635 ) ) ;
#33540 = CIRCLE ( 'NONE', #20428, 0.2149999999999999967 ) ;
#33541 = CARTESIAN_POINT ( 'NONE',  ( 0.01220488718634634047, -0.4284039509524131817, 0.1484612068426492959 ) ) ;
#33542 = CARTESIAN_POINT ( 'NONE',  ( 0.4104015424280102464, -1.716720069944782656, 0.4259487396392561687 ) ) ;
#33543 = CARTESIAN_POINT ( 'NONE',  ( -0.3000000000000000999, -2.183180860297908144, -0.4937760292030871079 ) ) ;
#33544 = CARTESIAN_POINT ( 'NONE',  ( 0.3699999999999797895, -2.143572916703662123, -0.4549832530184109713 ) ) ;
#33545 = AXIS2_PLACEMENT_3D ( 'NONE', #15375, #3222, #474 ) ;
#33546 = CARTESIAN_POINT ( 'NONE',  ( 0.3055995149173200143, -1.768272766478771185, 0.5197417262808792238 ) ) ;
#33547 = DIRECTION ( 'NONE',  ( -1.000000000000000000, -2.341930812374887555E-31, 1.664003471950578127E-31 ) ) ;
#33548 = CARTESIAN_POINT ( 'NONE',  ( 0.3398838260239651077, -1.651575993044620771, -0.3838325942033110061 ) ) ;
#33549 =( CONVERSION_BASED_UNIT ( 'INCH', #8264 ) LENGTH_UNIT ( ) NAMED_UNIT ( #26531 ) );
#33550 = CIRCLE ( 'NONE', #7941, 0.05000000000000000971 ) ;
#33551 = CARTESIAN_POINT ( 'NONE',  ( -0.1196588179077745229, -0.4996288669916953418, 0.3264677846082036927 ) ) ;
#33552 = CARTESIAN_POINT ( 'NONE',  ( 0.1492358308521446464, -1.145521527551625951, 0.9752184947445524665 ) ) ;
#33553 = CARTESIAN_POINT ( 'NONE',  ( -0.002362956543387900038, -0.8470628362243999288, 0.1457185332388702959 ) ) ;
#33554 = PERSON_AND_ORGANIZATION ( #28500, #32463 ) ;
#33555 = CARTESIAN_POINT ( 'NONE',  ( 0.3073438066573006555, -0.7730596496961650299, 0.7003458109913517360 ) ) ;
#33556 = CARTESIAN_POINT ( 'NONE',  ( 0.05201782277453716880, 0.01807851807932257804, -0.4701313241416041344 ) ) ;
#33557 = B_SPLINE_CURVE_WITH_KNOTS ( 'NONE', 3,
 ( #38104, #27848, #9309, #25381 ),
 .UNSPECIFIED., .F., .F.,
 ( 4, 4 ),
 ( 2.698596413362738298E-17, 0.0007105667304030845177 ),
 .UNSPECIFIED. ) ;
#33558 = ADVANCED_FACE ( 'NONE', ( #12719 ), #19106, .T. ) ;
#33559 = DIRECTION ( 'NONE',  ( 0.000000000000000000, 0.000000000000000000, -1.000000000000000000 ) ) ;
#33560 = ORIENTED_EDGE ( 'NONE', *, *, #32319, .T. ) ;
#33561 = CARTESIAN_POINT ( 'NONE',  ( 0.4567505080237029280, -1.144430849087659352, -0.6312584490681862892 ) ) ;
#33562 = CARTESIAN_POINT ( 'NONE',  ( 0.04086830232926540879, -0.7705385959941278839, 0.6340295093763037571 ) ) ;
#33563 = EDGE_CURVE ( 'NONE', #21137, #19197, #3559, .T. ) ;
#33564 = AXIS2_PLACEMENT_3D ( 'NONE', #4996, #8684, #40157 ) ;
#33565 = CARTESIAN_POINT ( 'NONE',  ( 0.1327793517848841753, -0.5956663927647375401, 0.3057313821641756135 ) ) ;
#33566 = CARTESIAN_POINT ( 'NONE',  ( 0.3449116085746372629, -1.629888100695539688, 0.4182417262808778569 ) ) ;
#33568 = VERTEX_POINT ( 'NONE', #37602 ) ;
#33567 = CARTESIAN_POINT ( 'NONE',  ( 0.3870357883928292608, -1.780379272394887913, -0.5270016673789699180 ) ) ;
#33569 = AXIS2_PLACEMENT_3D ( 'NONE', #431, #6525, #25675 ) ;
#33570 = EDGE_CURVE ( 'NONE', #11702, #20753, #16410, .T. ) ;
#33571 = CARTESIAN_POINT ( 'NONE',  ( 0.5761226916817485666, -1.227707429964641328, 0.7155794456320599961 ) ) ;
#33573 = ORIENTED_EDGE ( 'NONE', *, *, #18232, .T. ) ;
#33572 = EDGE_LOOP ( 'NONE', ( #9963, #2581 ) ) ;
#33574 = CARTESIAN_POINT ( 'NONE',  ( 0.07465030803409943017, -1.408573555510644892, -0.6612025271909880431 ) ) ;
#33575 = AXIS2_PLACEMENT_3D ( 'NONE', #12045, #11643, #5442 ) ;
#33576 = DIRECTION ( 'NONE',  ( 0.000000000000000000, -0.9510565162951529761, 0.3090169943749491166 ) ) ;
#33577 = AXIS2_PLACEMENT_3D ( 'NONE', #27217, #20032, #10768 ) ;
#33578 = LINE ( 'NONE', #15278, #332 ) ;
#33579 = APPROVAL_STATUS ( 'not_yet_approved' ) ;
#33581 = B_SPLINE_CURVE_WITH_KNOTS ( 'NONE', 3,
 ( #17338, #38726, #29067, #10362, #39343, #20028 ),
 .UNSPECIFIED., .F., .F.,
 ( 4, 2, 4 ),
 ( 0.003196928911404663034, 0.004123443478206876948, 0.005049958045009090429 ),
 .UNSPECIFIED. ) ;
#33580 = AXIS2_PLACEMENT_3D ( 'NONE', #18561, #5995, #6207 ) ;
#33582 = CARTESIAN_POINT ( 'NONE',  ( -0.03171102739523483371, 0.4481073524712024247, -0.2027236177532017181 ) ) ;
#33583 = ORIENTED_EDGE ( 'NONE', *, *, #11931, .F. ) ;
#33584 = DIRECTION ( 'NONE',  ( 0.000000000000000000, 0.000000000000000000, 1.000000000000000000 ) ) ;
#33585 = CARTESIAN_POINT ( 'NONE',  ( 0.2754527148808368353, -0.9793155036609090258, 0.7096650894199401094 ) ) ;
#33586 = CARTESIAN_POINT ( 'NONE',  ( 0.1677963985810169978, -1.186112715867778888, 1.005752358474822028 ) ) ;
#33587 = CARTESIAN_POINT ( 'NONE',  ( 0.2358021257645211977, -0.9592120825771568438, 0.7505977746809007201 ) ) ;
#33589 = CARTESIAN_POINT ( 'NONE',  ( -0.0006941592203410161229, -0.7620002068169634546, -0.005094063534273165009 ) ) ;
#33588 = DIRECTION ( 'NONE',  ( 1.000000000000000000, 0.000000000000000000, 0.000000000000000000 ) ) ;
#33590 = ADVANCED_FACE ( 'NONE', ( #31645 ), #9425, .F. ) ;
#33591 = CARTESIAN_POINT ( 'NONE',  ( 0.09409306777181461467, -1.290726425726503201, 0.6139492122977521227 ) ) ;
#33592 = ORIENTED_EDGE ( 'NONE', *, *, #1739, .F. ) ;
#33593 = ORIENTED_EDGE ( 'NONE', *, *, #6498, .F. ) ;
#33594 = CARTESIAN_POINT ( 'NONE',  ( 0.01548846960707524721, 0.5198120922912204955, -0.07362328916738319906 ) ) ;
#33595 = CARTESIAN_POINT ( 'NONE',  ( 0.6243188685325448128, -1.312786121592256938, 0.8640797252984854238 ) ) ;
#33596 = DIRECTION ( 'NONE',  ( 0.000000000000000000, 0.000000000000000000, -1.000000000000000000 ) ) ;
#33597 = CARTESIAN_POINT ( 'NONE',  ( 0.3699999999999786793, -2.080243653848455665, -0.5192469000150281566 ) ) ;
#33598 = AXIS2_PLACEMENT_3D ( 'NONE', #5349, #39935, #24309 ) ;
#33599 = DIRECTION ( 'NONE',  ( 0.8660254037844383745, 0.1781528605886715799, 0.4671847153579342660 ) ) ;
#33600 = CARTESIAN_POINT ( 'NONE',  ( 0.1251191340379213812, -1.316096326284950324, -0.6814256523839956614 ) ) ;
#33601 = FACE_OUTER_BOUND ( 'NONE', #15107, .T. ) ;
#33602 = CARTESIAN_POINT ( 'NONE',  ( 0.5553494029534283838, -1.189621637772522389, 0.5881472999875582142 ) ) ;
#33603 = APPROVAL_DATE_TIME ( #9319, #20757 ) ;
#33604 = CIRCLE ( 'NONE', #7310, 0.2500000000000000000 ) ;
#33605 = AXIS2_PLACEMENT_3D ( 'NONE', #14422, #33547, #5357 ) ;
#33606 = CARTESIAN_POINT ( 'NONE',  ( -0.1157923916715200702, -0.5295015842444287246, 0.3181161673586325178 ) ) ;
#33607 = AXIS2_PLACEMENT_3D ( 'NONE', #2325, #13182, #25968 ) ;
#33608 = CARTESIAN_POINT ( 'NONE',  ( 0.3610211414937801733, -1.953816409086856609, -0.6684869201605642131 ) ) ;
#33609 = CARTESIAN_POINT ( 'NONE',  ( -0.01548846960712810944, 0.3688619771571925998, -0.3775276577326300287 ) ) ;
#33610 = DIRECTION ( 'NONE',  ( 0.8660512985181132439, 0.4999551463232379533, 4.610901147014540750E-15 ) ) ;
#33611 = CARTESIAN_POINT ( 'NONE',  ( -0.1669433606228567790, 0.5138636982738122860, 0.3749999999999991673 ) ) ;
#33612 = ADVANCED_FACE ( 'NONE', ( #15806 ), #1614, .F. ) ;
#33613 = ORIENTED_EDGE ( 'NONE', *, *, #4228, .F. ) ;
#33614 = DIRECTION ( 'NONE',  ( -1.000000000000000000, -2.276539994720197063E-15, 0.000000000000000000 ) ) ;
#33615 = ADVANCED_FACE ( 'NONE', ( #25280 ), #32185, .T. ) ;
#33616 = CARTESIAN_POINT ( 'NONE',  ( 0.1130068117282509443, -0.8274064342018203622, 0.4102281928929959465 ) ) ;
#33617 = CARTESIAN_POINT ( 'NONE',  ( -0.05543910610525118465, 0.02035452233660139595, -0.4608669713610835106 ) ) ;
#33618 = CARTESIAN_POINT ( 'NONE',  ( 0.1665889528249037688, -1.217160154129576455, 0.7453979173672002911 ) ) ;
#33619 = ORIENTED_EDGE ( 'NONE', *, *, #33373, .F. ) ;
#33620 = CARTESIAN_POINT ( 'NONE',  ( -0.1157923916714455881, -0.5295015842440863318, 0.1380392329925437811 ) ) ;
#33621 = CARTESIAN_POINT ( 'NONE',  ( 0.03647060353175621272, -0.08366884794402436321, 0.5049308971818872172 ) ) ;
#33622 = CARTESIAN_POINT ( 'NONE',  ( 0.05076679145661966430, -0.4632958555242867593, -0.09915135732236152188 ) ) ;
#33623 = EDGE_CURVE ( 'NONE', #23421, #27179, #429, .T. ) ;
#33624 = CARTESIAN_POINT ( 'NONE',  ( 0.1985601496691580814, -2.023190444054567383, -0.2819993563027929917 ) ) ;
#33625 = CARTESIAN_POINT ( 'NONE',  ( 0.4014432137977476667, -1.148788978479662326, 0.6861530365891023164 ) ) ;
#33626 = AXIS2_PLACEMENT_3D ( 'NONE', #18952, #40542, #37447 ) ;
#33628 = CARTESIAN_POINT ( 'NONE',  ( 0.4835406691325078166, -1.674675384168304415, 0.5338177255081320016 ) ) ;
#33627 = CARTESIAN_POINT ( 'NONE',  ( 0.04760454375021537510, 0.4700983808485068027, 0.1075238135162369518 ) ) ;
#33629 = CARTESIAN_POINT ( 'NONE',  ( 0.1266021694322588820, -1.239399129679921829, 0.5182417262812423209 ) ) ;
#33630 = ORIENTED_EDGE ( 'NONE', *, *, #22513, .F. ) ;
#33631 = VERTEX_POINT ( 'NONE', #2360 ) ;
#33632 = CARTESIAN_POINT ( 'NONE',  ( 0.2418900393794059245, -0.8808406326854840707, 0.7271447531890425919 ) ) ;
#33633 = ORIENTED_EDGE ( 'NONE', *, *, #33445, .T. ) ;
#33634 = AXIS2_PLACEMENT_3D ( 'NONE', #2502, #40119, #8865 ) ;
#33635 = CARTESIAN_POINT ( 'NONE',  ( -0.02000000000000000042, -2.049319608666233528, -0.3639547633631710633 ) ) ;
#33636 = AXIS2_PLACEMENT_3D ( 'NONE', #1080, #38864, #26546 ) ;
#33637 = CARTESIAN_POINT ( 'NONE',  ( 0.4439955536442621864, -1.572094061263507925, 0.6295494919070759865 ) ) ;
#33639 = DIRECTION ( 'NONE',  ( 5.551115123125788865E-17, -3.676620095425087221E-16, -1.000000000000000000 ) ) ;
#33638 = CARTESIAN_POINT ( 'NONE',  ( -0.04293317454820552020, -0.4432234940308336646, 0.2195257349118416856 ) ) ;
#33640 = CARTESIAN_POINT ( 'NONE',  ( -0.08000000000000000167, -1.598492537578166672, -0.1971380022280825872 ) ) ;
#33641 = ADVANCED_FACE ( 'NONE', ( #34423 ), #6239, .F. ) ;
#33642 = EDGE_LOOP ( 'NONE', ( #30236, #1049, #11812, #34784 ) ) ;
#33643 = AXIS2_PLACEMENT_3D ( 'NONE', #12431, #5837, #15323 ) ;
#33644 = DIRECTION ( 'NONE',  ( 1.000000000000000000, 0.000000000000000000, 0.000000000000000000 ) ) ;
#33645 = VERTEX_POINT ( 'NONE', #5628 ) ;
#33646 = ADVANCED_FACE ( 'NONE', ( #11802 ), #18254, .T. ) ;
#33647 = CARTESIAN_POINT ( 'NONE',  ( 0.3912351814900760227, -1.953326783438015468, -0.4997197400164905545 ) ) ;
#33648 = CARTESIAN_POINT ( 'NONE',  ( 0.1251904040544656038, -0.5863800375748553506, 0.2858950053321839824 ) ) ;
#33649 = CARTESIAN_POINT ( 'NONE',  ( 0.4830736825586152139, -1.664257883331242693, 0.5549537226658294298 ) ) ;
#33650 = FACE_OUTER_BOUND ( 'NONE', #22568, .T. ) ;
#33651 = CARTESIAN_POINT ( 'NONE',  ( -0.05464101615137766793, -2.548345659627495596, -0.2263512047145338768 ) ) ;
#33652 = CARTESIAN_POINT ( 'NONE',  ( 0.02999999999997886302, -2.097675824466503691, -0.6968677163258658602 ) ) ;
#33653 = DIRECTION ( 'NONE',  ( 0.4999551463232372317, -0.8660512985181135770, 0.000000000000000000 ) ) ;
#33654 = CARTESIAN_POINT ( 'NONE',  ( 0.2225889308918536924, -1.238345268919997855, 0.5682417262808776570 ) ) ;
#33655 = CARTESIAN_POINT ( 'NONE',  ( 0.5517781715537678489, -1.195290833855036983, 0.8540039827052086086 ) ) ;
#33656 = CARTESIAN_POINT ( 'NONE',  ( 0.07690341661973157383, -1.324345918287141322, 0.4736064436466723149 ) ) ;
#33657 = CARTESIAN_POINT ( 'NONE',  ( -0.0003043527560127933592, -0.9376677575348233429, 0.2158120078562527078 ) ) ;
#33658 = CIRCLE ( 'NONE', #3457, 0.01500000000000001853 ) ;
#33659 = CARTESIAN_POINT ( 'NONE',  ( 0.6169636335926310666, -1.622911811178471497, -0.5279922895341171429 ) ) ;
#33660 = CARTESIAN_POINT ( 'NONE',  ( 0.08964076868335302262, -1.440626440711184619, -0.6869804198957685237 ) ) ;
#33661 = CARTESIAN_POINT ( 'NONE',  ( 0.6653925203977641978, -1.561488534969810438, 0.6071316550003091894 ) ) ;
#33662 = CARTESIAN_POINT ( 'NONE',  ( 0.3829573361688640154, -1.749254992990724622, -0.4372965273082253246 ) ) ;
#33663 = DIRECTION ( 'NONE',  ( -1.000000000000000000, -0.000000000000000000, -0.000000000000000000 ) ) ;
#33664 = AXIS2_PLACEMENT_3D ( 'NONE', #17077, #1467, #1677 ) ;
#33665 = VECTOR ( 'NONE', #35154, 39.37007874015748143 ) ;
#33666 = VERTEX_POINT ( 'NONE', #15514 ) ;
#33667 = CARTESIAN_POINT ( 'NONE',  ( 0.1958798485499332886, -1.272568564212325670, 1.036395571016125006 ) ) ;
#33668 = CARTESIAN_POINT ( 'NONE',  ( 0.3626617637547003836, -1.756793103646928644, -0.5948424371531259025 ) ) ;
#33669 = AXIS2_PLACEMENT_3D ( 'NONE', #17053, #7360, #4896 ) ;
#33670 = CARTESIAN_POINT ( 'NONE',  ( -0.3000000000000000999, -1.962518963160043706, -0.3791801492432049780 ) ) ;
#33671 = EDGE_CURVE ( 'NONE', #38278, #34438, #5516, .T. ) ;
#33672 = DIRECTION ( 'NONE',  ( 0.4999551463232372317, -0.8660512985181134660, 0.000000000000000000 ) ) ;
#33673 = B_SPLINE_CURVE_WITH_KNOTS ( 'NONE', 3,
 ( #14571, #8201, #35781, #11504, #14179, #20564, #30208, #39670, #13763, #4499, #33096, #17062, #26744, #29607, #26329, #30026, #1853, #7593, #14368, #20168, #26932, #20361, #26535, #39074, #39465, #10899, #11290, #23859, #36382, #24071 ),
 .UNSPECIFIED., .F., .F.,
 ( 4, 2, 2, 2, 2, 2, 2, 2, 2, 2, 2, 2, 2, 2, 4 ),
 ( -5.999999999964222910E-08, 0.0003594096777401402550, 0.0007188793554802801536, 0.001437818710960556698, 0.002875697421921122581, 0.004313576132881688681, 0.005751454843842254347, 0.008627212265763385679, 0.01006509097672395221, 0.01150296968768451875, 0.01437872710960562753, 0.01725448453152673978, 0.02013024195344785203, 0.02156812066440840989, 0.02300599937536896428 ),
 .UNSPECIFIED. ) ;
#33675 = ORIENTED_EDGE ( 'NONE', *, *, #2228, .T. ) ;
#33674 = B_SPLINE_SURFACE_WITH_KNOTS ( 'NONE', 3, 3, ( 
 ( #12516, #27754, #28163, #28, #15808, #34321, #12120, #24469, #3257, #12721 ),
 ( #28357, #24686, #40503, #25071, #25282, #21400, #19108, #16024, #37605, #31647 ),
 ( #33938, #37216, #9428, #18913, #37826, #18696, #37406, #22211, #6134, #9642 ),
 ( #21596, #2655, #5922, #18484, #31041, #22006, #28567, #37003, #34531, #227 ) ),
 .UNSPECIFIED., .F., .F., .F.,
 ( 4, 4 ),
 ( 4, 3, 3, 4 ),
 ( 0.3963327724766242399, 1.014871814752778434 ),
 ( -1.046553497504219397E-15, 0.4999999999999997224, 0.7500000000000001110, 1.000000000000000444 ),
 .UNSPECIFIED. ) ;
#33676 = CARTESIAN_POINT ( 'NONE',  ( 0.4002999475594375967, -1.110987091864168885, 0.6207864592343738108 ) ) ;
#33677 = AXIS2_PLACEMENT_3D ( 'NONE', #6286, #18856, #14745 ) ;
#33678 = CARTESIAN_POINT ( 'NONE',  ( 0.3249672098042813984, -1.168533503727528400, 0.5670347247539490043 ) ) ;
#33679 = DIRECTION ( 'NONE',  ( 0.01455087616121368381, 0.9998941303972840311, 0.000000000000000000 ) ) ;
#33680 = DIRECTION ( 'NONE',  ( -1.000000000000000000, -0.000000000000000000, -0.000000000000000000 ) ) ;
#33681 = CARTESIAN_POINT ( 'NONE',  ( 0.4745309070972864030, -1.255194402924658670, 0.7290776394288778217 ) ) ;
#33683 = ORIENTED_EDGE ( 'NONE', *, *, #17284, .T. ) ;
#33682 = DIRECTION ( 'NONE',  ( 1.000000000000000000, 0.000000000000000000, 0.000000000000000000 ) ) ;
#33684 = CARTESIAN_POINT ( 'NONE',  ( 0.4473065160884135416, -1.054428903401835704, 0.6531518022732211159 ) ) ;
#33685 = EDGE_LOOP ( 'NONE', ( #23496, #3289, #2336, #38035, #20103 ) ) ;
#33686 = DIRECTION ( 'NONE',  ( 0.000000000000000000, 0.000000000000000000, -1.000000000000000000 ) ) ;
#33687 = ORIENTED_EDGE ( 'NONE', *, *, #24325, .F. ) ;
#33688 = CARTESIAN_POINT ( 'NONE',  ( -0.1088121136105147380, -0.4964308608213456875, 0.09999999999999989453 ) ) ;
#33689 = ORIENTED_EDGE ( 'NONE', *, *, #18286, .T. ) ;
#33690 = CARTESIAN_POINT ( 'NONE',  ( 0.3560862010677396938, -1.622388544012473233, 0.5735089325637127144 ) ) ;
#33692 = CARTESIAN_POINT ( 'NONE',  ( 0.1142833079139667918, -0.5209214772459205278, -0.02864359220122766891 ) ) ;
#33691 = CARTESIAN_POINT ( 'NONE',  ( 0.06637855911726646407, -0.7256089028387239237, 0.002745430285754289681 ) ) ;
#33693 = DIRECTION ( 'NONE',  ( 0.007183093100618577476, 0.4999484090412817938, 0.8660253988599867503 ) ) ;
#33694 = CIRCLE ( 'NONE', #36987, 0.07999999999999996003 ) ;
#33695 = VERTEX_POINT ( 'NONE', #8923 ) ;
#33696 = ORIENTED_EDGE ( 'NONE', *, *, #9000, .T. ) ;
#33697 = CARTESIAN_POINT ( 'NONE',  ( 0.5121281216239255141, -1.125982481116337919, 0.6765354010138239227 ) ) ;
#33698 = B_SPLINE_CURVE_WITH_KNOTS ( 'NONE', 3,
 ( #36263, #11598, #36685, #2734 ),
 .UNSPECIFIED., .F., .F.,
 ( 4, 4 ),
 ( 0.000000000000000000, 1.000000000000000000 ),
 .UNSPECIFIED. ) ;
#33699 = ORIENTED_EDGE ( 'NONE', *, *, #23807, .T. ) ;
#33700 = CARTESIAN_POINT ( 'NONE',  ( 0.4219866632171650478, -1.610104465087853765, -0.3647299066799348233 ) ) ;
#33701 = CARTESIAN_POINT ( 'NONE',  ( 0.4165761542997364897, -1.741708882820427906, 0.5182417262812423209 ) ) ;
#33702 = AXIS2_PLACEMENT_3D ( 'NONE', #2866, #8829, #21409 ) ;
#33703 = AXIS2_PLACEMENT_3D ( 'NONE', #30047, #32298, #7396 ) ;
#33704 = CARTESIAN_POINT ( 'NONE',  ( 0.2154757676707194647, -1.081506276767553176, 0.7440243676801590045 ) ) ;
#33705 = CARTESIAN_POINT ( 'NONE',  ( 0.5718134511589890723, -1.573821939672337411, -0.4594826857674059739 ) ) ;
#33706 = VECTOR ( 'NONE', #32296, 39.37007874015747433 ) ;
#33707 = EDGE_CURVE ( 'NONE', #7421, #36854, #26565, .T. ) ;
#33708 = CARTESIAN_POINT ( 'NONE',  ( 0.5840964882222685617, -1.491811162635231058, -0.4356935235874836998 ) ) ;
#33709 = CIRCLE ( 'NONE', #2188, 0.1000000000000000194 ) ;
#33710 = CARTESIAN_POINT ( 'NONE',  ( -0.1707812261971881906, 0.4977922652119479152, 0.3123933982393728437 ) ) ;
#33711 = CARTESIAN_POINT ( 'NONE',  ( 0.07344416302227160798, -1.332345902377664260, 0.4917314202680824198 ) ) ;
#33712 = CARTESIAN_POINT ( 'NONE',  ( -2.070754768975509919, -0.09959325338431655739, 0.09813923389047504720 ) ) ;
#33713 =( GEOMETRIC_REPRESENTATION_CONTEXT ( 3 ) GLOBAL_UNCERTAINTY_ASSIGNED_CONTEXT ( ( #18632 ) ) GLOBAL_UNIT_ASSIGNED_CONTEXT ( ( #324, #38110, #35637 ) ) REPRESENTATION_CONTEXT ( 'NONE', 'WORKASPACE' ) );
#33714 = DIRECTION ( 'NONE',  ( 0.000000000000000000, 3.330669073875469621E-16, 1.000000000000000000 ) ) ;
#33715 = FACE_OUTER_BOUND ( 'NONE', #35361, .T. ) ;
#33716 = CALENDAR_DATE ( 2026, 13, 10 ) ;
#33717 = CARTESIAN_POINT ( 'NONE',  ( 0.4647723852893586582, -1.134116793214159147, 0.4600189020470820123 ) ) ;
#33718 = CARTESIAN_POINT ( 'NONE',  ( 0.3623650104644992598, -1.158602411851195724, 0.5324242784680641716 ) ) ;
#33719 = DIRECTION ( 'NONE',  ( 0.000000000000000000, 0.000000000000000000, -1.000000000000000000 ) ) ;
#33720 = CARTESIAN_POINT ( 'NONE',  ( 1.002343701812023279E-05, -0.5552538295932334389, -0.07958962418979929898 ) ) ;
#33721 = CARTESIAN_POINT ( 'NONE',  ( -0.02000000000000000042, -2.180619779672576364, -0.3917908354455199582 ) ) ;
#33722 = CIRCLE ( 'NONE', #27195, 0.005000000000000014849 ) ;
#33723 = CARTESIAN_POINT ( 'NONE',  ( 0.07272417404265385521, -0.8336665982203107506, 0.8213584970460865442 ) ) ;
#33724 = DIRECTION ( 'NONE',  ( -0.8660512985181130219, -0.4999551463232377868, 0.000000000000000000 ) ) ;
#33725 = ORIENTED_EDGE ( 'NONE', *, *, #29326, .T. ) ;
#33726 = B_SPLINE_CURVE_WITH_KNOTS ( 'NONE', 3,
 ( #5522, #18692, #31254, #28160 ),
 .UNSPECIFIED., .F., .F.,
 ( 4, 4 ),
 ( 1.734723475976807094E-18, 0.0004255989732717012559 ),
 .UNSPECIFIED. ) ;
#33727 = CIRCLE ( 'NONE', #37015, 0.01499999999999997689 ) ;
#33728 = VERTEX_POINT ( 'NONE', #28248 ) ;
#33729 = CIRCLE ( 'NONE', #38985, 0.01500000000000000291 ) ;
#33730 = CARTESIAN_POINT ( 'NONE',  ( -0.1133606652272154125, -0.5183057948313382068, 0.1157398326556813989 ) ) ;
#33731 = VERTEX_POINT ( 'NONE', #5819 ) ;
#33732 = DIRECTION ( 'NONE',  ( 0.3181970600707382246, -0.9480245940703960761, 3.970578237956065974E-16 ) ) ;
#33733 = CARTESIAN_POINT ( 'NONE',  ( -0.1124521194441292365, -0.5140518175047488203, 0.1111873348898323038 ) ) ;
#33735 = ORIENTED_EDGE ( 'NONE', *, *, #13417, .F. ) ;
#33734 = CARTESIAN_POINT ( 'NONE',  ( 0.001639899432043153858, -0.5409522198614201693, 0.06344722032422416003 ) ) ;
#33736 = AXIS2_PLACEMENT_3D ( 'NONE', #24182, #20688, #2162 ) ;
#33737 = ORIENTED_EDGE ( 'NONE', *, *, #18835, .T. ) ;
#33738 = CARTESIAN_POINT ( 'NONE',  ( 0.1978587402095111636, -0.5849795632145003976, 0.3178455878192510409 ) ) ;
#33739 = VERTEX_POINT ( 'NONE', #112 ) ;
#33740 = AXIS2_PLACEMENT_3D ( 'NONE', #32099, #37661, #279 ) ;
#33741 = CARTESIAN_POINT ( 'NONE',  ( 0.2663068527664966267, -1.675293026590164880, 0.5727052833931987053 ) ) ;
#33743 = CARTESIAN_POINT ( 'NONE',  ( 0.1273065581027945647, -1.282153141076411318, 0.6035032530794141037 ) ) ;
#33742 = FACE_OUTER_BOUND ( 'NONE', #34009, .T. ) ;
#33744 = CARTESIAN_POINT ( 'NONE',  ( 0.1590992539432692365, -1.295692464083599171, 0.5182417262812423209 ) ) ;
#33745 = CALENDAR_DATE ( 2026, 13, 10 ) ;
#33746 = CARTESIAN_POINT ( 'NONE',  ( -0.1696273608102555064, 0.4941101834779049740, 0.3212105875170800373 ) ) ;
#33748 = ORIENTED_EDGE ( 'NONE', *, *, #39561, .F. ) ;
#33747 = ORIENTED_EDGE ( 'NONE', *, *, #38310, .F. ) ;
#33749 = CARTESIAN_POINT ( 'NONE',  ( 0.01140841165526322240, -0.9199322217433030247, 0.03086158767695902291 ) ) ;
#33750 = CARTESIAN_POINT ( 'NONE',  ( 0.1862143093560868212, -0.9153542374866747711, 0.1423358669777752550 ) ) ;
#33751 = LINE ( 'NONE', #9069, #2821 ) ;
#33752 = CARTESIAN_POINT ( 'NONE',  ( 0.2556524848986769793, -0.9586451026735138825, 0.7438133644576581105 ) ) ;
#33753 =( BOUNDED_SURFACE ( )  B_SPLINE_SURFACE ( 3, 2, ( 
 ( #31790, #25432, #574 ),
 ( #34862, #13069, #15344 ),
 ( #6671, #22546, #12450 ),
 ( #25621, #18633, #38153 ) ),
 .UNSPECIFIED., .F., .F., .T. ) 
 B_SPLINE_SURFACE_WITH_KNOTS ( ( 4, 4 ),
 ( 3, 3 ),
 ( -1.387778780781445676E-17, 0.001804009323275673022 ),
 ( 0.000000000000000000, 1.000000000000000000 ),
 .UNSPECIFIED. ) 
 GEOMETRIC_REPRESENTATION_ITEM ( )  RATIONAL_B_SPLINE_SURFACE ( (
 ( 1.000000000000000000, 0.7071067811865464625, 1.000000000000000000),
 ( 1.000000000000000000, 0.7071042723947947861, 1.000000000000000000),
 ( 1.000000000000000000, 0.7064338697126878452, 1.000000000000000000),
 ( 1.000000000000000000, 0.7053326528219889813, 1.000000000000000000) ) ) 
 REPRESENTATION_ITEM ( '' )  SURFACE ( )  );
#33754 = CARTESIAN_POINT ( 'NONE',  ( 0.1866433404661365369, -0.7454955835292522703, 0.03807266482934637541 ) ) ;
#33755 = CARTESIAN_POINT ( 'NONE',  ( 0.3511079287476752686, -1.164805985122749687, 0.4335040596137051394 ) ) ;
#33756 = LINE ( 'NONE', #39323, #17833 ) ;
#33757 = AXIS2_PLACEMENT_3D ( 'NONE', #38234, #35366, #19928 ) ;
#33758 = CARTESIAN_POINT ( 'NONE',  ( 0.4170221576077899894, -1.703439424313293094, -0.4186838340555589233 ) ) ;
#33759 = DIRECTION ( 'NONE',  ( -0.7525498468814693087, -0.4343474113619809063, 0.4949859131347307817 ) ) ;
#33760 = ADVANCED_FACE ( 'NONE', ( #24963 ), #30927, .F. ) ;
#33761 = DIRECTION ( 'NONE',  ( 0.000000000000000000, 0.000000000000000000, -1.000000000000000000 ) ) ;
#33762 = CIRCLE ( 'NONE', #10806, 0.03749999999977551152 ) ;
#33763 = DIRECTION ( 'NONE',  ( 1.000000000000000000, -0.000000000000000000, -0.000000000000000000 ) ) ;
#33764 = CARTESIAN_POINT ( 'NONE',  ( 0.4814184380812144282, -1.664799897621735303, 0.3157417262808778213 ) ) ;
#33765 = AXIS2_PLACEMENT_3D ( 'NONE', #37189, #3046, #12482 ) ;
#33766 = CARTESIAN_POINT ( 'NONE',  ( 0.4001190030211318471, -1.111027321722804606, 0.6208328323685005090 ) ) ;
#33767 = CARTESIAN_POINT ( 'NONE',  ( 0.3681092974666538842, -1.616496510625566208, -0.4182513407341701406 ) ) ;
#33768 = DIRECTION ( 'NONE',  ( 1.848892746611746419E-32, -1.665334536937734811E-16, 1.000000000000000000 ) ) ;
#33769 = EDGE_CURVE ( 'NONE', #22735, #28470, #2752, .T. ) ;
#33770 = CARTESIAN_POINT ( 'NONE',  ( 0.03672447062657864525, -0.2485879206383752038, 0.4115698867982532372 ) ) ;
#33771 = ADVANCED_FACE ( 'NONE', ( #37710 ), #33777, .T. ) ;
#33772 = CARTESIAN_POINT ( 'NONE',  ( 0.06825878040686909898, -0.8404074238475144343, 0.8024108098889147778 ) ) ;
#33773 = VECTOR ( 'NONE', #16173, 39.37007874015748854 ) ;
#33774 = CARTESIAN_POINT ( 'NONE',  ( 0.08014420339816276384, -1.182225237729999101, 0.7631665397026843323 ) ) ;
#33775 = PERSON_AND_ORGANIZATION_ROLE ( 'creator' ) ;
#33776 = CARTESIAN_POINT ( 'NONE',  ( 0.6998761188508713094, -1.434392152549301747, 0.7385670194571644087 ) ) ;
#33777 = CONICAL_SURFACE ( 'NONE', #16724, 0.3698489655878005045, 1.211529128687673262 ) ;
#33778 = CARTESIAN_POINT ( 'NONE',  ( 0.000000000000000000, 0.000000000000000000, 0.000000000000000000 ) ) ;
#33779 = CARTESIAN_POINT ( 'NONE',  ( 0.2629665421248923995, -1.157745397434066126, -0.5155029497116575543 ) ) ;
#33780 = EDGE_CURVE ( 'NONE', #30237, #29543, #4297, .T. ) ;
#33781 = CARTESIAN_POINT ( 'NONE',  ( 0.3761389819862501205, -1.668938135269312895, -0.4224620603250751616 ) ) ;
#33782 = EDGE_LOOP ( 'NONE', ( #6964, #27249, #24812, #23134 ) ) ;
#33783 = CARTESIAN_POINT ( 'NONE',  ( -0.2746410161513779258, -2.377368549242099949, -0.4802393080720198104 ) ) ;
#33784 = APPLIED_PERSON_AND_ORGANIZATION_ASSIGNMENT ( #28415, #15662, ( #39149 ) ) ;
#33785 = B_SPLINE_CURVE_WITH_KNOTS ( 'NONE', 3,
 ( #36062, #23941, #1746, #10772, #27012, #23344 ),
 .UNSPECIFIED., .F., .F.,
 ( 4, 2, 4 ),
 ( 0.000000000000000000, 0.5000000000000000000, 1.000000000000000000 ),
 .UNSPECIFIED. ) ;
#33786 = CARTESIAN_POINT ( 'NONE',  ( 0.1683595846758117187, -1.287579619409340292, 0.9462029255750337153 ) ) ;
#33787 = CIRCLE ( 'NONE', #35108, 0.03000000000000008563 ) ;
#33788 = CARTESIAN_POINT ( 'NONE',  ( 0.5888136248176969456, -1.490730112924630424, 0.5990021645472617395 ) ) ;
#33790 = VERTEX_POINT ( 'NONE', #327 ) ;
#33789 = CARTESIAN_POINT ( 'NONE',  ( -0.01548846960707490547, 0.5198120922912040642, 0.07362328916749247276 ) ) ;
#33791 = VECTOR ( 'NONE', #22866, 39.37007874015748143 ) ;
#33792 = CARTESIAN_POINT ( 'NONE',  ( 0.6177995476601370051, -1.296677486146512681, 0.6035100636680229558 ) ) ;
#33794 = VERTEX_POINT ( 'NONE', #22303 ) ;
#33793 = EDGE_LOOP ( 'NONE', ( #24380, #31473 ) ) ;
#33795 = CARTESIAN_POINT ( 'NONE',  ( 0.5885374655969598523, -1.253074615311095652, 0.8149014300617682949 ) ) ;
#33796 = AXIS2_PLACEMENT_3D ( 'NONE', #12085, #33672, #5484 ) ;
#33797 = AXIS2_PLACEMENT_3D ( 'NONE', #27936, #24857, #34293 ) ;
#33798 = DIRECTION ( 'NONE',  ( -0.4999999999999976685, 0.5006794435238191010, -0.7066258520834637347 ) ) ;
#33799 = APPROVAL_PERSON_ORGANIZATION ( #39337, #28254, #11158 ) ;
#33800 = CARTESIAN_POINT ( 'NONE',  ( 0.1399999999999994582, -3.326417233800874210E-17, -0.1249999999999999584 ) ) ;
#33801 = PERSON_AND_ORGANIZATION ( #36787, #35245 ) ;
#33802 = CYLINDRICAL_SURFACE ( 'NONE', #30975, 0.03749999999977554621 ) ;
#33803 = VERTEX_POINT ( 'NONE', #38721 ) ;
#33804 = CARTESIAN_POINT ( 'NONE',  ( 0.1463705207591960988, -0.7909580375454078327, 0.5232196913181064168 ) ) ;
#33805 = CARTESIAN_POINT ( 'NONE',  ( 0.3112602777207036375, -1.738619137813147031, 0.7428781199237085575 ) ) ;
#33806 = CARTESIAN_POINT ( 'NONE',  ( 0.4782480661408347600, -1.500260821454189042, 0.7558612605875917323 ) ) ;
#33807 = AXIS2_PLACEMENT_3D ( 'NONE', #28958, #31860, #34938 ) ;
#33809 = CARTESIAN_POINT ( 'NONE',  ( -0.01548846960721204577, 0.5203207976464816475, 0.08861466064783131424 ) ) ;
#33808 = CARTESIAN_POINT ( 'NONE',  ( 0.5953197980378833742, -1.599064723402610300, 0.4311035055375501135 ) ) ;
#33810 = CARTESIAN_POINT ( 'NONE',  ( 0.05992090360963508999, -1.332693131100006312, 0.5767975242531366842 ) ) ;
#33811 = ORIENTED_EDGE ( 'NONE', *, *, #34158, .F. ) ;
#33812 = EDGE_LOOP ( 'NONE', ( #24381, #12628, #22238, #35917 ) ) ;
#33813 = CARTESIAN_POINT ( 'NONE',  ( -0.1663058949916037810, 0.5166728756553465862, 0.1255325300626441154 ) ) ;
#33814 = CARTESIAN_POINT ( 'NONE',  ( 0.3784499407546133010, -1.011947937249764173, 0.8629558619193703484 ) ) ;
#33815 = EDGE_CURVE ( 'NONE', #35103, #20340, #39700, .T. ) ;
#33816 = LINE ( 'NONE', #12216, #37106 ) ;
#33817 = B_SPLINE_CURVE_WITH_KNOTS ( 'NONE', 3,
 ( #6389, #9690, #9478, #31696 ),
 .UNSPECIFIED., .F., .F.,
 ( 4, 4 ),
 ( 0.000000000000000000, 0.0004633377961365348703 ),
 .UNSPECIFIED. ) ;
#33818 = EDGE_CURVE ( 'NONE', #29632, #35323, #10542, .T. ) ;
#33819 = CARTESIAN_POINT ( 'NONE',  ( -0.2399999999999999079, -1.835749455202394298, -0.3938319975228649072 ) ) ;
#33820 = AXIS2_PLACEMENT_3D ( 'NONE', #23602, #36117, #7924 ) ;
#33821 = ADVANCED_FACE ( 'NONE', ( #29058 ), #5633, .T. ) ;
#33822 = CARTESIAN_POINT ( 'NONE',  ( 0.5840964882222685617, -1.491811162635231058, -0.4356935235874836998 ) ) ;
#33823 = EDGE_CURVE ( 'NONE', #39055, #5283, #10710, .T. ) ;
#33824 = AXIS2_PLACEMENT_3D ( 'NONE', #20675, #29712, #19849 ) ;
#33825 = CARTESIAN_POINT ( 'NONE',  ( 0.06046277342610767436, -1.448078595047667116, -0.6496421378630458099 ) ) ;
#33826 = EDGE_CURVE ( 'NONE', #36494, #21571, #14715, .T. ) ;
#33827 = CARTESIAN_POINT ( 'NONE',  ( 0.3225244551428645967, -1.181327507850448155, 0.4853335682619487335 ) ) ;
#33828 = CARTESIAN_POINT ( 'NONE',  ( 0.4978751173634345939, -1.107738205778658669, 0.6841874689585324409 ) ) ;
#33829 = AXIS2_PLACEMENT_3D ( 'NONE', #32496, #26338, #39474 ) ;
#33830 = PERSON_AND_ORGANIZATION ( #28500, #32463 ) ;
#33831 = VECTOR ( 'NONE', #7636, 39.37007874015748854 ) ;
#33832 = CARTESIAN_POINT ( 'NONE',  ( 0.1895842342730561514, -0.5876096019965807438, 0.2995157642027707623 ) ) ;
#33833 = SECURITY_CLASSIFICATION ( '', '', #23977 ) ;
#33834 = LINE ( 'NONE', #15096, #22611 ) ;
#33835 = CARTESIAN_POINT ( 'NONE',  ( 0.03113248654051816583, -3.491513147198971704E-33, 0.2000000000000000111 ) ) ;
#33836 = AXIS2_PLACEMENT_3D ( 'NONE', #6529, #7325, #28765 ) ;
#33837 = CARTESIAN_POINT ( 'NONE',  ( -0.04575334816098020063, -0.3363904506959644602, -0.3523376320073989820 ) ) ;
#33838 = EDGE_CURVE ( 'NONE', #11782, #37196, #10790, .T. ) ;
#33839 = EDGE_LOOP ( 'NONE', ( #10923, #5321, #2688, #22245 ) ) ;
#33840 = DIRECTION ( 'NONE',  ( 0.2259631160204149669, 0.000000000000000000, 0.9741358581832129104 ) ) ;
#33841 = CARTESIAN_POINT ( 'NONE',  ( -0.01899468245561106855, -0.3622301702732843576, 0.3730449234618263277 ) ) ;
#33842 = DIRECTION ( 'NONE',  ( -0.4709550870498656616, 0.000000000000000000, -0.8821571889305518388 ) ) ;
#33843 = ORIENTED_EDGE ( 'NONE', *, *, #35309, .T. ) ;
#33844 = CARTESIAN_POINT ( 'NONE',  ( -0.04308745346420374267, -0.05688354191225564876, -0.4910214150057568006 ) ) ;
#33845 = CARTESIAN_POINT ( 'NONE',  ( 0.03443144359732585452, -0.9312087828476524054, 0.6026922210726547435 ) ) ;
#33847 = EDGE_LOOP ( 'NONE', ( #22524, #38016, #13396, #14882 ) ) ;
#33846 = ORIENTED_EDGE ( 'NONE', *, *, #27413, .F. ) ;
#33848 = CARTESIAN_POINT ( 'NONE',  ( -0.02953079040095700838, 0.000000000000000000, 0.000000000000000000 ) ) ;
#33849 = CARTESIAN_POINT ( 'NONE',  ( 0.04575185649130613513, -0.06505045373102469330, 0.4827759578813183849 ) ) ;
#33850 = CARTESIAN_POINT ( 'NONE',  ( 0.04762035657657653215, -0.4434998562185943349, -0.1892652133704821049 ) ) ;
#33851 = CARTESIAN_POINT ( 'NONE',  ( 0.3573173253698222473, -1.879934324363079501, -0.3378928523157883612 ) ) ;
#33852 = AXIS2_PLACEMENT_3D ( 'NONE', #15337, #18219, #40626 ) ;
#33853 = CARTESIAN_POINT ( 'NONE',  ( 0.4488667739067040974, -1.208173968264157905, 0.6504506168610796335 ) ) ;
#33855 = CARTESIAN_POINT ( 'NONE',  ( 0.2211959769661343000, -1.309495541150525799, -0.7462941026102624109 ) ) ;
#33854 = CARTESIAN_POINT ( 'NONE',  ( -0.09596847297450977754, 0.06113703066755011434, 0.08377772888334905632 ) ) ;
#33856 = ORIENTED_EDGE ( 'NONE', *, *, #25995, .F. ) ;
#33857 = AXIS2_PLACEMENT_3D ( 'NONE', #26486, #33258, #5068 ) ;
#33858 = EDGE_LOOP ( 'NONE', ( #3455, #39463, #38954, #19034 ) ) ;
#33859 = PLANE ( 'NONE',  #39503 ) ;
#33860 = VERTEX_POINT ( 'NONE', #31953 ) ;
#33861 = CARTESIAN_POINT ( 'NONE',  ( 0.7050990918974278099, -1.519384653903026905, 0.5628786012043504039 ) ) ;
#33862 = CARTESIAN_POINT ( 'NONE',  ( 0.4433254787940574815, -1.568196705436662342, 0.6582884301997589116 ) ) ;
#33864 = CARTESIAN_POINT ( 'NONE',  ( 0.5673723352274240295, -1.614853471436807242, 0.4836300718228428996 ) ) ;
#33863 = DIRECTION ( 'NONE',  ( -0.3468893892380661148, 0.9373665302208729067, 0.03180785525185500506 ) ) ;
#33865 = CARTESIAN_POINT ( 'NONE',  ( 0.3048982267989297501, -1.756746414302344350, 0.5594309555313059512 ) ) ;
#33866 = LOCAL_TIME ( 0, 53, 7.000000000000000000, #21078 ) ;
#33867 = ORIENTED_EDGE ( 'NONE', *, *, #11878, .T. ) ;
#33868 = DIRECTION ( 'NONE',  ( 1.000000000000000000, 0.000000000000000000, 0.000000000000000000 ) ) ;
#33869 = CARTESIAN_POINT ( 'NONE',  ( 0.3868936632023516897, -1.853519627552301152, -0.3097036711958909283 ) ) ;
#33870 = CARTESIAN_POINT ( 'NONE',  ( 0.3914081408461116407, -1.186566226689276915, 0.8257643602198004862 ) ) ;
#33871 = CARTESIAN_POINT ( 'NONE',  ( 0.4737921430874441620, -1.667306459498246296, 0.4630076221598910524 ) ) ;
#33872 = CARTESIAN_POINT ( 'NONE',  ( -0.08000000000000000167, -2.253856486606507836, -0.7252438489935795207 ) ) ;
#33873 = EDGE_CURVE ( 'NONE', #6348, #35653, #28453, .T. ) ;
#33874 = ORIENTED_EDGE ( 'NONE', *, *, #12304, .T. ) ;
#33875 = CARTESIAN_POINT ( 'NONE',  ( -0.03868649100028168086, 0.4624880946332503573, 0.1149381524902354512 ) ) ;
#33876 = B_SPLINE_CURVE_WITH_KNOTS ( 'NONE', 3,
 ( #14946, #27498, #2202, #15561, #18234, #40024, #33875, #5864, #8971, #9162, #5679, #21545, #2802, #15349, #18638, #27907, #40447, #12271 ),
 .UNSPECIFIED., .F., .F.,
 ( 4, 2, 2, 2, 2, 2, 2, 2, 4 ),
 ( 0.0003425652276237348809, 0.001007165397454244833, 0.001671765567284754731, 0.002336365737115264629, 0.003000965906945774527, 0.003665566076776284425, 0.004330166246606793889, 0.004994766416437303354, 0.005659366586267813685 ),
 .UNSPECIFIED. ) ;
#33877 = CARTESIAN_POINT ( 'NONE',  ( 0.4419048264408291793, -1.686280600454908019, 0.4284299735155673861 ) ) ;
#33878 = EDGE_CURVE ( 'NONE', #27248, #14778, #26499, .T. ) ;
#33879 = CARTESIAN_POINT ( 'NONE',  ( 0.6300550326132239309, -1.371036769560420421, -0.6250000000000000000 ) ) ;
#33880 = DIRECTION ( 'NONE',  ( 1.000000000000000000, 0.000000000000000000, 8.537024980200777445E-16 ) ) ;
#33881 = EDGE_CURVE ( 'NONE', #3745, #8808, #29673, .T. ) ;
#33882 = CARTESIAN_POINT ( 'NONE',  ( 0.4993356427094534644, -1.110845742389603430, 0.8468575151840780357 ) ) ;
#33883 = CARTESIAN_POINT ( 'NONE',  ( -0.04139678531769643011, 0.2626830136224079237, 0.3904580303439411648 ) ) ;
#33884 = CARTESIAN_POINT ( 'NONE',  ( 0.02071941500637600186, -1.004773761618042993, 0.5203810855262117618 ) ) ;
#33885 = EDGE_CURVE ( 'NONE', #28931, #38085, #13823, .T. ) ;
#33886 = AXIS2_PLACEMENT_3D ( 'NONE', #28741, #16808, #28926 ) ;
#33887 = CARTESIAN_POINT ( 'NONE',  ( 0.5822092398946240310, -1.604441550281183737, -0.4592476338510794176 ) ) ;
#33888 = VECTOR ( 'NONE', #3284, 39.37007874015748143 ) ;
#33889 = DIRECTION ( 'NONE',  ( -1.000000000000000000, -0.000000000000000000, -0.000000000000000000 ) ) ;
#33890 = CARTESIAN_POINT ( 'NONE',  ( 0.6179826973912112553, -1.588466188088726305, 0.6165989319811293612 ) ) ;
#33891 = CARTESIAN_POINT ( 'NONE',  ( 0.03868649100028150739, 0.3066017772948840814, -0.3648306000529298321 ) ) ;
#33892 = DIRECTION ( 'NONE',  ( -1.000000000000000000, -0.000000000000000000, -0.000000000000000000 ) ) ;
#33893 = EDGE_CURVE ( 'NONE', #6212, #40008, #12174, .T. ) ;
#33894 = LOCAL_TIME ( 0, 53, 7.000000000000000000, #11966 ) ;
#33895 = VERTEX_POINT ( 'NONE', #1316 ) ;
#33896 = CARTESIAN_POINT ( 'NONE',  ( 0.01548846960707524721, 0.4638115001430989648, -0.2459753896937820483 ) ) ;
#33897 = CARTESIAN_POINT ( 'NONE',  ( 0.4170115945640068822, -1.702980413955155425, -0.6123808887097256237 ) ) ;
#33898 = EDGE_CURVE ( 'NONE', #24795, #21660, #20475, .T. ) ;
#33899 = CARTESIAN_POINT ( 'NONE',  ( 0.1337229918471090351, -1.289495155180872876, 0.5510147389724832090 ) ) ;
#33900 = CARTESIAN_POINT ( 'NONE',  ( 0.3589389236034170594, -1.749584479564031625, 0.5938934903193374693 ) ) ;
#33901 = EDGE_CURVE ( 'NONE', #16266, #2769, #12680, .T. ) ;
#33902 = AXIS2_PLACEMENT_3D ( 'NONE', #7085, #19655, #16569 ) ;
#33903 = VERTEX_POINT ( 'NONE', #7662 ) ;
#33904 = CARTESIAN_POINT ( 'NONE',  ( 0.1994740068363786423, -2.042640899752901085, -0.2765909798240093198 ) ) ;
#33905 = CARTESIAN_POINT ( 'NONE',  ( 0.3551276078911581591, -1.131964321692829678, 0.6011313928527168837 ) ) ;
#33906 = LINE ( 'NONE', #5703, #20437 ) ;
#33907 = CARTESIAN_POINT ( 'NONE',  ( 0.04157078424165694397, 0.2900150886686586604, -0.3701869471361532438 ) ) ;
#33908 = CARTESIAN_POINT ( 'NONE',  ( 0.5168936871241821551, -1.320940109607575019, 0.6421529002730038682 ) ) ;
#33910 = FACE_OUTER_BOUND ( 'NONE', #16216, .T. ) ;
#33909 = CARTESIAN_POINT ( 'NONE',  ( 0.01548846960703782229, -0.4638115001431039053, -0.2459753896937787732 ) ) ;
#33911 = CARTESIAN_POINT ( 'NONE',  ( 0.5078487756305317680, -1.109832367716456325, 0.6054007957810670915 ) ) ;
#33912 = ORIENTED_EDGE ( 'NONE', *, *, #11800, .F. ) ;
#33913 = PERSON_AND_ORGANIZATION_ROLE ( 'creator' ) ;
#33914 = CARTESIAN_POINT ( 'NONE',  ( -0.2399999999999999079, -3.849534981189179028, -0.3510928155360652503 ) ) ;
#33915 = ORIENTED_EDGE ( 'NONE', *, *, #9532, .F. ) ;
#33916 = DIRECTION ( 'NONE',  ( -1.000000000000000000, -0.000000000000000000, -0.000000000000000000 ) ) ;
#33917 = ORIENTED_EDGE ( 'NONE', *, *, #28069, .F. ) ;
#33918 = CARTESIAN_POINT ( 'NONE',  ( 0.03595399678886468386, -0.5498052390641160470, 0.2287210428828644337 ) ) ;
#33920 = CARTESIAN_POINT ( 'NONE',  ( 0.1133187343594337232, -0.6553192386313622109, -0.09367839676004516281 ) ) ;
#33919 = CARTESIAN_POINT ( 'NONE',  ( 0.3558574630237864023, -1.162065433541755510, 0.4306974791478214160 ) ) ;
#33921 = DIRECTION ( 'NONE',  ( 1.787262988391350055E-31, 0.8983234858819699742, -0.4393346272636222682 ) ) ;
#33922 = ORIENTED_EDGE ( 'NONE', *, *, #12734, .T. ) ;
#33923 = VERTEX_POINT ( 'NONE', #33360 ) ;
#33924 = AXIS2_PLACEMENT_3D ( 'NONE', #21581, #18072, #12106 ) ;
#33925 = CARTESIAN_POINT ( 'NONE',  ( 0.2471793377096756505, -1.006172282673910123, 0.5861680647017392110 ) ) ;
#33926 = CARTESIAN_POINT ( 'NONE',  ( 0.1192653334777903779, -0.6126589172736857103, 0.3521971464290056253 ) ) ;
#33927 = EDGE_LOOP ( 'NONE', ( #28429, #9230 ) ) ;
#33928 = DIRECTION ( 'NONE',  ( 0.000000000000000000, -0.5781348229923771731, 0.8159412518334715481 ) ) ;
#33929 = FACE_OUTER_BOUND ( 'NONE', #38088, .T. ) ;
#33930 = LOCAL_TIME ( 0, 53, 7.000000000000000000, #520 ) ;
#33931 = DIRECTION ( 'NONE',  ( -1.188678714063518424E-15, 1.000000000000000000, 0.000000000000000000 ) ) ;
#33932 = EDGE_CURVE ( 'NONE', #36711, #20307, #29804, .T. ) ;
#33933 = CARTESIAN_POINT ( 'NONE',  ( -0.1210963378865855811, -0.5065302875297102991, 0.3108129518247090828 ) ) ;
#33934 = EDGE_CURVE ( 'NONE', #40614, #5313, #23327, .T. ) ;
#33935 = AXIS2_PLACEMENT_3D ( 'NONE', #21631, #18326, #9254 ) ;
#33936 = DIRECTION ( 'NONE',  ( -5.551115123125767911E-17, 5.007578356027541926E-16, 1.000000000000000000 ) ) ;
#33937 = CARTESIAN_POINT ( 'NONE',  ( 0.4802217237380822512, -1.662726879635128219, 0.3667417262808781442 ) ) ;
#33938 = CARTESIAN_POINT ( 'NONE',  ( 0.2490119727783751402, -1.333982754301515028, -0.7187326247832955817 ) ) ;
#33939 = CARTESIAN_POINT ( 'NONE',  ( 0.001484713323275439105, -0.9577160478316373293, 0.3237126889746802516 ) ) ;
#33940 = PERSON_AND_ORGANIZATION_ROLE ( 'design_supplier' ) ;
#33941 = CARTESIAN_POINT ( 'NONE',  ( 0.4825669698268504892, -1.124365842536106053, 0.5003378186883976619 ) ) ;
#33942 = CARTESIAN_POINT ( 'NONE',  ( 0.5595653757848308985, -1.183094497137172629, 0.6057417262809812186 ) ) ;
#33943 = CARTESIAN_POINT ( 'NONE',  ( 0.5782730993802743802, -1.562463384465315519, -0.5918479448017719413 ) ) ;
#33944 = CARTESIAN_POINT ( 'NONE',  ( -0.002083146443013340551, -0.8967360763018591419, 0.1296726476164832831 ) ) ;
#33945 = LINE ( 'NONE', #34332, #12717 ) ;
#33946 = CARTESIAN_POINT ( 'NONE',  ( 0.3991140026135005514, -1.226416419011188808, 0.5182417262812423209 ) ) ;
#33947 = CARTESIAN_POINT ( 'NONE',  ( 0.1960722456818422554, -1.288731303253010330, -0.2917126172454976296 ) ) ;
#33948 = VERTEX_POINT ( 'NONE', #39739 ) ;
#33949 = ORIENTED_EDGE ( 'NONE', *, *, #11773, .T. ) ;
#33950 = CARTESIAN_POINT ( 'NONE',  ( -0.1044436713285742391, -0.4741860147765890043, 0.1089215716837025894 ) ) ;
#33951 = ORIENTED_EDGE ( 'NONE', *, *, #33671, .T. ) ;
#33952 = APPROVAL_PERSON_ORGANIZATION ( #14834, #11774, #26969 ) ;
#33953 = DIRECTION ( 'NONE',  ( 0.5794373887239211429, -0.8150167559926626559, 5.038681971366855054E-15 ) ) ;
#33954 = CARTESIAN_POINT ( 'NONE',  ( -0.1148699535791915805, -0.5253002637279400311, 0.1262353127152416599 ) ) ;
#33956 = ORIENTED_EDGE ( 'NONE', *, *, #4610, .T. ) ;
#33955 = DIRECTION ( 'NONE',  ( 0.4999999999999968359, 0.000000000000000000, -0.8660254037844405950 ) ) ;
#33957 = ORIENTED_EDGE ( 'NONE', *, *, #6623, .F. ) ;
#33958 = DIRECTION ( 'NONE',  ( 0.000000000000000000, 0.5877852522924936762, -0.8090169943749323522 ) ) ;
#33959 = ORIENTED_EDGE ( 'NONE', *, *, #7205, .T. ) ;
#33960 = CARTESIAN_POINT ( 'NONE',  ( 0.08011936691053324344, -0.9288656528420190517, 0.7837102162258990923 ) ) ;
#33962 = CARTESIAN_POINT ( 'NONE',  ( 0.1047782527215795206, -1.275408578320203157, 0.5976651094688776311 ) ) ;
#33961 = CARTESIAN_POINT ( 'NONE',  ( 0.06650046747100032962, -0.8363599969432670145, 0.2317722016253256911 ) ) ;
#33963 = DIRECTION ( 'NONE',  ( 1.000000000000000000, -0.000000000000000000, -0.000000000000000000 ) ) ;
#33964 = DIRECTION ( 'NONE',  ( 0.9823333030490228879, -0.1871397384865027547, 5.691349986800549851E-16 ) ) ;
#33966 = ORIENTED_EDGE ( 'NONE', *, *, #15523, .F. ) ;
#33965 = EDGE_LOOP ( 'NONE', ( #9125, #7790, #25609, #2933, #2238, #22429 ) ) ;
#33967 = CARTESIAN_POINT ( 'NONE',  ( 0.3915344748440447442, -1.113207836370987636, 0.6228311983407980312 ) ) ;
#33968 = DIRECTION ( 'NONE',  ( -1.000000000000000000, 0.000000000000000000, 0.000000000000000000 ) ) ;
#33969 = CARTESIAN_POINT ( 'NONE',  ( -0.05279185365593582618, -0.4562178057547947585, 0.1062796545748983384 ) ) ;
#33970 = CARTESIAN_POINT ( 'NONE',  ( 0.1833549916660507650, -0.8423218050691670955, 0.6657346342128551697 ) ) ;
#33971 = CARTESIAN_POINT ( 'NONE',  ( 0.4737412056605618815, -1.678808096592666388, 0.5629907880828596278 ) ) ;
#33972 = CYLINDRICAL_SURFACE ( 'NONE', #33626, 0.1000000000000000056 ) ;
#33973 = CARTESIAN_POINT ( 'NONE',  ( 0.01617491007160833452, -0.4928941197314672951, 0.3779610642509277363 ) ) ;
#33974 = CARTESIAN_POINT ( 'NONE',  ( 0.4161606292527415540, -1.703533559239368556, 0.4226782797517861789 ) ) ;
#33975 = AXIS2_PLACEMENT_3D ( 'NONE', #40190, #34023, #15097 ) ;
#33976 = CARTESIAN_POINT ( 'NONE',  ( -0.05464101615137786222, -2.321277022828569958, -0.5785054236952983375 ) ) ;
#33977 = DIRECTION ( 'NONE',  ( 2.280301054154496008E-31, -1.000000000000000000, 3.330669073875470114E-16 ) ) ;
#33978 = CARTESIAN_POINT ( 'NONE',  ( -0.0003802752418593652317, -0.9311711565920335332, 0.09304606914443409871 ) ) ;
#33979 = DIRECTION ( 'NONE',  ( -1.000000000000000000, -0.000000000000000000, -0.000000000000000000 ) ) ;
#33980 = CARTESIAN_POINT ( 'NONE',  ( 0.2922741047311901985, -1.688215408676643658, 0.8015225518757634893 ) ) ;
#33981 = CARTESIAN_POINT ( 'NONE',  ( 0.05225207911860056675, -1.070115161207997101, 0.7386715066487512527 ) ) ;
#33982 = APPROVAL_DATE_TIME ( #21457, #24749 ) ;
#33983 = CARTESIAN_POINT ( 'NONE',  ( 0.4224057990199354684, -0.9849677903659747047, 0.8092447908785728172 ) ) ;
#33984 = CARTESIAN_POINT ( 'NONE',  ( -0.2300000000000000655, 0.5182417262804733804, 0.3749999999999999445 ) ) ;
#33985 = CARTESIAN_POINT ( 'NONE',  ( -0.01548846960712824648, 0.07651041855115098267, -0.5222379212567075379 ) ) ;
#33986 = FACE_OUTER_BOUND ( 'NONE', #32402, .T. ) ;
#33987 = ORIENTED_EDGE ( 'NONE', *, *, #36869, .F. ) ;
#33988 = DIRECTION ( 'NONE',  ( -7.771561172376107616E-16, 7.170354002788761615E-17, -1.000000000000000000 ) ) ;
#33989 = CARTESIAN_POINT ( 'NONE',  ( 0.2635503086687465135, -1.597273101066688961, 0.8385226914806884757 ) ) ;
#33990 = CARTESIAN_POINT ( 'NONE',  ( 0.1283342468025234773, -0.5638928911301458458, 0.2184306303221273671 ) ) ;
#33992 = ORIENTED_EDGE ( 'NONE', *, *, #11938, .T. ) ;
#33991 = CARTESIAN_POINT ( 'NONE',  ( 0.3862110256088816529, -1.731934476144517010, 0.4282538419479021141 ) ) ;
#33993 = CARTESIAN_POINT ( 'NONE',  ( 0.2089316498445973613, -0.7245868578893045475, 0.3779356710034222910 ) ) ;
#33995 = ORIENTED_EDGE ( 'NONE', *, *, #6117, .T. ) ;
#33994 = ORIENTED_EDGE ( 'NONE', *, *, #40311, .T. ) ;
#33996 = CARTESIAN_POINT ( 'NONE',  ( 0.4539313471337609318, -1.044844956913612677, 0.7902625984474508369 ) ) ;
#33997 =( BOUNDED_SURFACE ( )  B_SPLINE_SURFACE ( 3, 2, ( 
 ( #19858, #33553, #26054 ),
 ( #7086, #10590, #20076 ),
 ( #24138, #20843, #13865 ),
 ( #39742, #38573, #23164 ),
 ( #11576, #32604, #10394 ),
 ( #14858, #16781, #38977 ),
 ( #35475, #19656, #32191 ),
 ( #1176, #26238, #36660 ),
 ( #4418, #16977, #29519 ),
 ( #30271, #1356, #26442 ),
 ( #14638, #27421, #10809 ),
 ( #23384, #36458, #5171 ),
 ( #17723, #2101, #27209 ),
 ( #8466, #21030, #5362 ),
 ( #2317, #34377, #11965 ),
 ( #37058, #27811, #21456 ),
 ( #6194, #34171, #24529 ),
 ( #24738, #18542, #37667 ),
 ( #36849, #8880, #40553 ),
 ( #9081, #33981, #286 ),
 ( #34591, #6395, #5786 ),
 ( #24321, #8662, #40347 ),
 ( #15469, #18343, #30888 ),
 ( #37265, #27607, #18762 ),
 ( #12175, #21850, #30697 ),
 ( #21235, #18961, #33774 ),
 ( #12373, #2709, #21647 ),
 ( #5583, #24929, #31495 ),
 ( #15253, #18142, #5979 ),
 ( #3119, #2518, #15057 ),
 ( #31311, #31096, #40136 ),
 ( #15661, #37457, #15866 ),
 ( #2917, #3305, #28210 ),
 ( #28020, #76, #9274 ),
 ( #12570, #25129, #9488 ),
 ( #22067, #28414, #4110 ),
 ( #6582, #28822, #10098 ),
 ( #23063, #19574, #12994 ),
 ( #19164, #31702, #16085 ),
 ( #25542, #10495, #22264 ),
 ( #25346, #681, #25740 ),
 ( #16888, #32503, #19757 ),
 ( #35592, #4326, #13383 ),
 ( #34777, #22673, #28626 ),
 ( #13170, #38485, #497 ),
 ( #29431, #19966, #38070 ) ),
 .UNSPECIFIED., .F., .F., .T. ) 
 B_SPLINE_SURFACE_WITH_KNOTS ( ( 4, 2, 2, 2, 2, 2, 2, 2, 2, 2, 2, 2, 2, 2, 2, 2, 2, 2, 2, 2, 2, 2, 4 ),
 ( 3, 3 ),
 ( 0.004598587694449686458, 0.008053666893016626915, 0.01150874609158356564, 0.01496382529015050436, 0.01582759508979223947, 0.01669136488943397459, 0.01841890448871744482, 0.01928267428835917646, 0.02014644408800091158, 0.02101021388764264669, 0.02187398368728438180, 0.02273775348692611692, 0.02360152328656785203, 0.02532906288585132226, 0.02619283268549305738, 0.02705660248513479249, 0.02792037228477652760, 0.02878414208441826272, 0.02964791188405999783, 0.03051168168370173295, 0.03094356658352260050, 0.03137545148334346806, 0.03223922128298520318 ),
 ( 0.000000000000000000, 1.000000000000000000 ),
 .UNSPECIFIED. ) 
 GEOMETRIC_REPRESENTATION_ITEM ( )  RATIONAL_B_SPLINE_SURFACE ( (
 ( 1.000000000000000000, 0.7632047519019736770, 1.000000000000000000),
 ( 1.000000000000000000, 0.7632286149905481709, 1.000000000000000000),
 ( 1.000000000000000000, 0.7629254557762273903, 1.000000000000000000),
 ( 1.000000000000000000, 0.7637623039598308017, 1.000000000000000000),
 ( 1.000000000000000000, 0.7648987287669885005, 1.000000000000000000),
 ( 1.000000000000000000, 0.7701097848380057398, 1.000000000000000000),
 ( 1.000000000000000000, 0.7743524099804016680, 1.000000000000000000),
 ( 1.000000000000000000, 0.7814619412129618636, 1.000000000000000000),
 ( 1.000000000000000000, 0.7829602748593540440, 1.000000000000000000),
 ( 1.000000000000000000, 0.7860833734074590406, 1.000000000000000000),
 ( 1.000000000000000000, 0.7877007998171637881, 1.000000000000000000),
 ( 1.000000000000000000, 0.7924769341938445733, 1.000000000000000000),
 ( 1.000000000000000000, 0.7956231603520705908, 1.000000000000000000),
 ( 1.000000000000000000, 0.7994035787022366613, 1.000000000000000000),
 ( 1.000000000000000000, 0.8005088628952052865, 1.000000000000000000),
 ( 1.000000000000000000, 0.8022700022555464550, 1.000000000000000000),
 ( 1.000000000000000000, 0.8029714101659524150, 1.000000000000000000),
 ( 1.000000000000000000, 0.8038112144617808319, 1.000000000000000000),
 ( 1.000000000000000000, 0.8039451361680508557, 1.000000000000000000),
 ( 1.000000000000000000, 0.8034950465542111120, 1.000000000000000000),
 ( 1.000000000000000000, 0.8029308292737085129, 1.000000000000000000),
 ( 1.000000000000000000, 0.8014392268801329156, 1.000000000000000000),
 ( 1.000000000000000000, 0.8004564543759468132, 1.000000000000000000),
 ( 1.000000000000000000, 0.7979003383569539531, 1.000000000000000000),
 ( 1.000000000000000000, 0.7962632686529542703, 1.000000000000000000),
 ( 1.000000000000000000, 0.7909923980647605157, 1.000000000000000000),
 ( 1.000000000000000000, 0.7869922070366083267, 1.000000000000000000),
 ( 1.000000000000000000, 0.7800571597425866033, 1.000000000000000000),
 ( 1.000000000000000000, 0.7775874025926204913, 1.000000000000000000),
 ( 1.000000000000000000, 0.7724354519564852195, 1.000000000000000000),
 ( 1.000000000000000000, 0.7697310273206949827, 1.000000000000000000),
 ( 1.000000000000000000, 0.7640258123504037879, 1.000000000000000000),
 ( 1.000000000000000000, 0.7609241244781310698, 1.000000000000000000),
 ( 1.000000000000000000, 0.7541134444708277318, 1.000000000000000000),
 ( 1.000000000000000000, 0.7504651226881818848, 1.000000000000000000),
 ( 1.000000000000000000, 0.7429106411578584312, 1.000000000000000000),
 ( 1.000000000000000000, 0.7390392288429025180, 1.000000000000000000),
 ( 1.000000000000000000, 0.7307215126039489084, 1.000000000000000000),
 ( 1.000000000000000000, 0.7264137187239084748, 1.000000000000000000),
 ( 1.000000000000000000, 0.7203301539224434835, 1.000000000000000000),
 ( 1.000000000000000000, 0.7183325906642731296, 1.000000000000000000),
 ( 1.000000000000000000, 0.7145333189904975457, 1.000000000000000000),
 ( 1.000000000000000000, 0.7127256081940787080, 1.000000000000000000),
 ( 1.000000000000000000, 0.7076437807589661677, 1.000000000000000000),
 ( 1.000000000000000000, 0.7048615031870756331, 1.000000000000000000),
 ( 1.000000000000000000, 0.7032008504187987619, 1.000000000000000000) ) ) 
 REPRESENTATION_ITEM ( '' )  SURFACE ( )  );
#33998 = CARTESIAN_POINT ( 'NONE',  ( -2.070754768975504589, -0.09959325338431362917, 0.3599999999999976552 ) ) ;
#33999 = DIRECTION ( 'NONE',  ( -1.387778780781449225E-15, 6.616194359655655447E-16, -1.000000000000000000 ) ) ;
#34000 = CARTESIAN_POINT ( 'NONE',  ( -0.01548846960707531660, -0.5198120922912100594, 0.07362328916748400731 ) ) ;
#34001 = ORIENTED_EDGE ( 'NONE', *, *, #13883, .T. ) ;
#34002 = CARTESIAN_POINT ( 'NONE',  ( 0.08731704049279917501, -0.7051593094029652287, 0.1785453983726967564 ) ) ;
#34003 = CIRCLE ( 'NONE', #40578, 0.01499999999999997342 ) ;
#34004 = CARTESIAN_POINT ( 'NONE',  ( 0.2059273467974226113, -1.283046334493782359, -0.7462941026102624109 ) ) ;
#34005 = CARTESIAN_POINT ( 'NONE',  ( 0.1048038408359760476, -0.5640354025563051321, 0.2328515503754501059 ) ) ;
#34007 = CARTESIAN_POINT ( 'NONE',  ( -0.0004942178885020764119, -0.7418118112770993866, -0.01346943646478583612 ) ) ;
#34006 = CARTESIAN_POINT ( 'NONE',  ( 0.3180120677078723812, -1.763266930125749088, 0.5173096362706023355 ) ) ;
#34008 = CARTESIAN_POINT ( 'NONE',  ( -0.03309060444528717781, -0.3730661130945393533, 0.3633899800202449182 ) ) ;
#34009 = EDGE_LOOP ( 'NONE', ( #31778, #32829, #696, #20561 ) ) ;
#34010 = FACE_OUTER_BOUND ( 'NONE', #18115, .T. ) ;
#34011 = CARTESIAN_POINT ( 'NONE',  ( 0.6069988657307503477, -1.282399503386861372, 0.8072536527268652229 ) ) ;
#34012 = DIRECTION ( 'NONE',  ( 0.3515883117872520836, -3.118021572908016454E-16, -0.9361547195921142706 ) ) ;
#34013 = CARTESIAN_POINT ( 'NONE',  ( 0.03113248654051816583, 0.1969856463038233696, 0.03459270371430114843 ) ) ;
#34014 = APPLIED_PERSON_AND_ORGANIZATION_ASSIGNMENT ( #15384, #9194, ( #3006 ) ) ;
#34015 = DIRECTION ( 'NONE',  ( -1.000000000000000000, -2.341930812374887555E-31, 1.664003471950578127E-31 ) ) ;
#34016 = CARTESIAN_POINT ( 'NONE',  ( 0.3824648761353414694, -1.161281635105729793, 0.4182417262808778013 ) ) ;
#34017 = DIRECTION ( 'NONE',  ( 0.000000000000000000, 0.000000000000000000, -1.000000000000000000 ) ) ;
#34018 = CARTESIAN_POINT ( 'NONE',  ( 0.3157767417926863884, -1.173633493893747604, 0.4907895864628127325 ) ) ;
#34019 = CARTESIAN_POINT ( 'NONE',  ( 0.4767475950167052168, -1.082687895696078595, 0.6905128956159171105 ) ) ;
#34020 = PERSON_AND_ORGANIZATION ( #28500, #32463 ) ;
#34021 = CARTESIAN_POINT ( 'NONE',  ( 0.6575684296065228418, -1.565022818668032167, 0.6191063639631391169 ) ) ;
#34022 = CARTESIAN_POINT ( 'NONE',  ( 0.3673039290742221574, -2.033686460013540476, -0.5076811077424107088 ) ) ;
#34023 = DIRECTION ( 'NONE',  ( 1.188678714063518227E-15, -1.000000000000000000, -3.263080277421930985E-16 ) ) ;
#34024 = CARTESIAN_POINT ( 'NONE',  ( -0.02953079040095578714, -0.09152108205201867075, 0.5223162075576457397 ) ) ;
#34025 = EDGE_CURVE ( 'NONE', #38792, #890, #6778, .T. ) ;
#34026 = ORIENTED_EDGE ( 'NONE', *, *, #1154, .F. ) ;
#34027 = DIRECTION ( 'NONE',  ( 0.9998941247116546194, -0.01455087607601020239, 0.0001066420868422379362 ) ) ;
#34028 = DIRECTION ( 'NONE',  ( -0.4494955276729005189, -0.2607972048181872449, 0.8543644354495810722 ) ) ;
#34029 = DIRECTION ( 'NONE',  ( 8.881784197001246407E-16, -2.361472542561082612E-16, 1.000000000000000000 ) ) ;
#34030 = ORIENTED_EDGE ( 'NONE', *, *, #23266, .F. ) ;
#34031 = CARTESIAN_POINT ( 'NONE',  ( -0.03474824846560305158, 0.07233741238827121056, -0.5114535313566268560 ) ) ;
#34032 = CARTESIAN_POINT ( 'NONE',  ( 0.1946323581323236296, -1.284704817078259120, 0.7082202489593650840 ) ) ;
#34034 = ORIENTED_EDGE ( 'NONE', *, *, #15299, .T. ) ;
#34033 = ORIENTED_EDGE ( 'NONE', *, *, #17578, .F. ) ;
#34035 = ADVANCED_FACE ( 'NONE', ( #11154 ), #17537, .T. ) ;
#34036 = DIRECTION ( 'NONE',  ( 0.4999999999999995559, 0.6123724356957944703, -0.6123724356957950254 ) ) ;
#34037 = VERTEX_POINT ( 'NONE', #27205 ) ;
#34038 = CARTESIAN_POINT ( 'NONE',  ( 0.01548846960706656839, -0.07651041855119576629, 0.5222379212568392104 ) ) ;
#34039 = CARTESIAN_POINT ( 'NONE',  ( 0.03170953572518869085, -0.4481091876101387927, -0.2027274919608517967 ) ) ;
#34040 = CARTESIAN_POINT ( 'NONE',  ( 0.3663529472107202034, -2.014034532710156533, -0.3144416355455260104 ) ) ;
#34041 = ADVANCED_FACE ( 'NONE', ( #16928 ), #30431, .T. ) ;
#34042 = DIRECTION ( 'NONE',  ( -0.4999551463232377313, 0.8660512985181132439, 0.000000000000000000 ) ) ;
#34044 = CARTESIAN_POINT ( 'NONE',  ( 0.009280570092012071712, -0.4278883025115321481, 0.1457185332388686028 ) ) ;
#34043 = FACE_OUTER_BOUND ( 'NONE', #4013, .T. ) ;
#34045 = EDGE_CURVE ( 'NONE', #9507, #3931, #32750, .T. ) ;
#34046 = CARTESIAN_POINT ( 'NONE',  ( -0.04582889109739218120, -0.3361233334071005996, -0.3523147457849535868 ) ) ;
#34047 = VERTEX_POINT ( 'NONE', #39144 ) ;
#34048 = EDGE_CURVE ( 'NONE', #17694, #16008, #34750, .T. ) ;
#34049 = CARTESIAN_POINT ( 'NONE',  ( 0.06947962733063202390, -1.315600342532642797, 0.5272843072721160596 ) ) ;
#34050 = ORIENTED_EDGE ( 'NONE', *, *, #18768, .F. ) ;
#34051 = LINE ( 'NONE', #9149, #19387 ) ;
#34052 = CARTESIAN_POINT ( 'NONE',  ( 0.4414602493135039718, -1.573691556144694692, 0.5701842070315025213 ) ) ;
#34054 = CARTESIAN_POINT ( 'NONE',  ( 0.5692155472414205386, -1.626790725381059177, 0.5412322144065360163 ) ) ;
#34053 = DIRECTION ( 'NONE',  ( -1.000000000000000000, -0.000000000000000000, -0.000000000000000000 ) ) ;
#34055 = CARTESIAN_POINT ( 'NONE',  ( 0.5602796947073411804, -1.505596977389118685, 0.5133479035088003295 ) ) ;
#34056 = CARTESIAN_POINT ( 'NONE',  ( 0.1655517683749154478, -1.273122889555738935, -0.2993625373774341791 ) ) ;
#34057 = ORIENTED_EDGE ( 'NONE', *, *, #35417, .T. ) ;
#34058 = DIRECTION ( 'NONE',  ( 0.8660512985181134660, 0.4999551463232372317, 0.000000000000000000 ) ) ;
#34059 = CARTESIAN_POINT ( 'NONE',  ( 0.1978993062382036205, -2.015598760273982215, -0.2839550029289699129 ) ) ;
#34060 = CARTESIAN_POINT ( 'NONE',  ( 0.1223192797020816736, -0.5513356496355160674, 0.1705091651870799807 ) ) ;
#34061 = CARTESIAN_POINT ( 'NONE',  ( 0.4598108443664392087, -1.687057064927079297, 0.4518108406592880599 ) ) ;
#34062 = CARTESIAN_POINT ( 'NONE',  ( -0.05464101615137786222, -2.379949255320110257, -0.6346823614705312533 ) ) ;
#34063 = ADVANCED_FACE ( 'NONE', ( #12568 ), #12371, .F. ) ;
#34064 = DIRECTION ( 'NONE',  ( 0.000000000000000000, 0.000000000000000000, -1.000000000000000000 ) ) ;
#34065 = CARTESIAN_POINT ( 'NONE',  ( 0.4909954411287530407, -1.657501613187781775, 0.4182417262808775793 ) ) ;
#34066 = CARTESIAN_POINT ( 'NONE',  ( 0.1590992539432692365, -1.295692464083599171, 0.5182417262812423209 ) ) ;
#34067 = CARTESIAN_POINT ( 'NONE',  ( 0.3434800707737146741, -1.169184835483404905, 0.4282596159937968605 ) ) ;
#34068 = CARTESIAN_POINT ( 'NONE',  ( 0.6005716857727874114, -1.273429356927226364, 0.8451723082856259506 ) ) ;
#34069 = CARTESIAN_POINT ( 'NONE',  ( -0.03474824846560758962, 0.2421026470131133479, 0.4562934628913907220 ) ) ;
#34070 = CARTESIAN_POINT ( 'NONE',  ( 0.002922095070481303073, -0.9671335970068797305, 0.3874888977936652990 ) ) ;
#34071 = CARTESIAN_POINT ( 'NONE',  ( 0.6417090595529835184, -1.440402100915940675, -0.4001723068962777519 ) ) ;
#34072 = CARTESIAN_POINT ( 'NONE',  ( 0.03188314084667491499, -1.843474523003271415, -0.6753216049888512984 ) ) ;
#34073 = DIRECTION ( 'NONE',  ( -1.000000000000000000, -7.857794173099924470E-32, -8.628166150854818811E-32 ) ) ;
#34074 = CARTESIAN_POINT ( 'NONE',  ( 0.2677971797784672314, -1.674570292523664294, 0.5743078772006583455 ) ) ;
#34075 = LINE ( 'NONE', #40242, #15324 ) ;
#34076 = ORIENTED_EDGE ( 'NONE', *, *, #9641, .F. ) ;
#34077 = DIRECTION ( 'NONE',  ( 0.000000000000000000, -0.7071067811865465735, -0.7071067811865484609 ) ) ;
#34078 = CARTESIAN_POINT ( 'NONE',  ( 0.4841245483858538368, -1.549657009352272352, 0.5686873558213612068 ) ) ;
#34079 = CARTESIAN_POINT ( 'NONE',  ( 0.3675360074875105854, -2.037884037106168389, -0.4877351960998094205 ) ) ;
#34080 = CARTESIAN_POINT ( 'NONE',  ( 0.4258288446711951392, -1.697684769104331526, -0.6161890926816561143 ) ) ;
#34081 = B_SPLINE_CURVE_WITH_KNOTS ( 'NONE', 3,
 ( #29962, #10832, #30153, #38782, #36310, #17195 ),
 .UNSPECIFIED., .F., .F.,
 ( 4, 2, 4 ),
 ( 0.0005396597967631549695, 0.001451180847823622336, 0.002362701898884089595 ),
 .UNSPECIFIED. ) ;
#34082 = ORIENTED_EDGE ( 'NONE', *, *, #39715, .F. ) ;
#34083 = EDGE_CURVE ( 'NONE', #29082, #36582, #40284, .T. ) ;
#34084 = CARTESIAN_POINT ( 'NONE',  ( 0.5260973920207011600, -1.675551188159756677, -0.5699138614228782540 ) ) ;
#34085 = CARTESIAN_POINT ( 'NONE',  ( -0.2399999999999999079, -4.320736256378554963, -0.8145269479932405465 ) ) ;
#34086 = CARTESIAN_POINT ( 'NONE',  ( 0.1850841550199354701, -0.8515884040318244530, 0.1812164098636643572 ) ) ;
#34087 = B_SPLINE_CURVE_WITH_KNOTS ( 'NONE', 3,
 ( #16988, #38584, #987, #32405 ),
 .UNSPECIFIED., .F., .F.,
 ( 4, 4 ),
 ( 1.734723475976807094E-18, 0.0007662876003044726252 ),
 .UNSPECIFIED. ) ;
#34088 = CARTESIAN_POINT ( 'NONE',  ( -0.2300000000000000655, 0.5182417262804733804, 0.3749999999999999445 ) ) ;
#34089 = ADVANCED_FACE ( 'NONE', ( #27419 ), #74, .F. ) ;
#34090 = CARTESIAN_POINT ( 'NONE',  ( 0.4001801618615863920, -1.148636508920398258, 0.7310201398396796169 ) ) ;
#34092 = CARTESIAN_POINT ( 'NONE',  ( 0.5304790502634055827, -1.600740321689024359, -0.5932381786332882045 ) ) ;
#34091 = CARTESIAN_POINT ( 'NONE',  ( -0.1684323895664702475, 0.5231977504175419069, 0.1528658435937316484 ) ) ;
#34093 = CARTESIAN_POINT ( 'NONE',  ( 0.2060221519102763132, -0.8840977030479291177, 0.3560353928791143985 ) ) ;
#34094 = ORIENTED_EDGE ( 'NONE', *, *, #38075, .T. ) ;
#34095 = PERSON_AND_ORGANIZATION_ROLE ( 'design_supplier' ) ;
#34096 = EDGE_CURVE ( 'NONE', #15099, #8761, #23322, .T. ) ;
#34097 = DIRECTION ( 'NONE',  ( -2.526820087036053001E-31, -0.1402348365095093807, 0.9901182710308659152 ) ) ;
#34098 = VERTEX_POINT ( 'NONE', #37263 ) ;
#34099 = ORIENTED_EDGE ( 'NONE', *, *, #7180, .F. ) ;
#34100 = CARTESIAN_POINT ( 'NONE',  ( 0.03842595133820840558, -0.5761514843590607171, 0.3024418328014801816 ) ) ;
#34102 = CARTESIAN_POINT ( 'NONE',  ( 0.1762309537805641091, -0.5849416173095501881, -0.06031293326471942606 ) ) ;
#34101 = CARTESIAN_POINT ( 'NONE',  ( 0.06592485238751269461, -0.7613911970652081918, 0.01751281745013728505 ) ) ;
#34103 = CARTESIAN_POINT ( 'NONE',  ( 0.2456699162554547011, -1.579418306085378143, -0.3207381830095928921 ) ) ;
#34104 = ORIENTED_EDGE ( 'NONE', *, *, #8697, .F. ) ;
#34105 = EDGE_LOOP ( 'NONE', ( #40326, #3052, #700, #946, #26856, #30991, #15844, #21916, #30657, #7500, #665, #21765, #29030, #36666, #1889, #13007, #12634, #5385, #31523, #5806, #9301, #22533, #28645, #17576, #5103, #17407, #127 ) ) ;
#34106 = CARTESIAN_POINT ( 'NONE',  ( 0.2981519290491080887, -1.037850129404853883, 0.6229852180713888465 ) ) ;
#34107 = CARTESIAN_POINT ( 'NONE',  ( 0.4535351762197513681, -1.347617495928803866, 0.8275486820836309709 ) ) ;
#34108 = VERTEX_POINT ( 'NONE', #24527 ) ;
#34109 = CYLINDRICAL_SURFACE ( 'NONE', #12772, 0.1749999999999999889 ) ;
#34110 = DIRECTION ( 'NONE',  ( 0.000000000000000000, 0.000000000000000000, -1.000000000000000000 ) ) ;
#34111 = ADVANCED_FACE ( 'NONE', ( #15251 ), #27605, .F. ) ;
#34112 = FACE_OUTER_BOUND ( 'NONE', #35004, .T. ) ;
#34113 = EDGE_CURVE ( 'NONE', #15872, #2643, #34169, .T. ) ;
#34114 = CARTESIAN_POINT ( 'NONE',  ( 0.5934892211655993233, -1.486388914344519696, -0.3866566986715374021 ) ) ;
#34115 = EDGE_CURVE ( 'NONE', #12918, #9065, #18034, .T. ) ;
#34116 = B_SPLINE_CURVE_WITH_KNOTS ( 'NONE', 3,
 ( #14814, #24282, #27565, #19329, #6960, #15818, #24893, #12951, #31052, #25299, #3082, #19119, #22413, #6544, #12336, #237, #6147, #34738, #27975, #18924, #18711, #35161, #6351, #34945, #22220, #37417 ),
 .UNSPECIFIED., .F., .F.,
 ( 4, 2, 2, 2, 2, 2, 2, 2, 2, 2, 2, 2, 4 ),
 ( 0.000000000000000000, 0.0008799450821173545071, 0.001759890164234709014, 0.002639835246352063847, 0.003519780328469418029, 0.004399725410586773078, 0.005279670492704127693, 0.007039560656938837792, 0.008799450821173547890, 0.01055934098540825886, 0.01231923114964296982, 0.01319917623176032444, 0.01407912131387767905 ),
 .UNSPECIFIED. ) ;
#34117 = CARTESIAN_POINT ( 'NONE',  ( 0.5985082606850495868, -1.473464502187743941, 0.6023744451300401259 ) ) ;
#34118 = CARTESIAN_POINT ( 'NONE',  ( 0.3060205578877235877, -1.769002121529782423, 0.4687417262808789009 ) ) ;
#34119 = CARTESIAN_POINT ( 'NONE',  ( 0.1939671707469822481, -1.242525794052198096, 0.6031029377704193450 ) ) ;
#34120 = DIRECTION ( 'NONE',  ( 0.000000000000000000, 0.000000000000000000, -1.000000000000000000 ) ) ;
#34121 = CARTESIAN_POINT ( 'NONE',  ( 1.365923996832131609E-16, -0.9481888444201341803, 0.1298224387748352637 ) ) ;
#34122 = PERSON_AND_ORGANIZATION ( #28500, #32463 ) ;
#34123 = CARTESIAN_POINT ( 'NONE',  ( 0.4851165728318759252, -1.078419517084477697, 0.6030839855583299824 ) ) ;
#34124 = CARTESIAN_POINT ( 'NONE',  ( 0.4737035873274689224, -1.116906127828866335, 0.5614642110315988255 ) ) ;
#34125 = CARTESIAN_POINT ( 'NONE',  ( 0.5435348920822987706, -1.168928385231105427, 0.5856983068965041506 ) ) ;
#34126 = CARTESIAN_POINT ( 'NONE',  ( 0.5947987396514448077, -1.485632953921246946, -0.6449812926602518370 ) ) ;
#34127 = CARTESIAN_POINT ( 'NONE',  ( 0.09860045244982779122, -1.306187320691368337, 0.7507959704929506595 ) ) ;
#34128 = CARTESIAN_POINT ( 'NONE',  ( 0.2011892967074957184, -1.251141541415955682, -0.7187326247832955817 ) ) ;
#34129 = CYLINDRICAL_SURFACE ( 'NONE', #13359, 0.1000000000000000194 ) ;
#34130 = CARTESIAN_POINT ( 'NONE',  ( 0.3484677573834994435, -1.177852168535778565, 0.4182417262808778013 ) ) ;
#34131 = ORIENTED_EDGE ( 'NONE', *, *, #19260, .T. ) ;
#34132 = ORIENTED_EDGE ( 'NONE', *, *, #36612, .T. ) ;
#34133 = DIRECTION ( 'NONE',  ( 0.9998941303973200023, -0.01455087615875037474, 0.000000000000000000 ) ) ;
#34134 = ORIENTED_EDGE ( 'NONE', *, *, #31764, .F. ) ;
#34135 = CARTESIAN_POINT ( 'NONE',  ( 0.2686719937394452806, -1.673937497439395461, 0.4971255110577562086 ) ) ;
#34136 = CARTESIAN_POINT ( 'NONE',  ( 0.05999999999999990757, -0.2461558908287989345, -0.2173297548048775396 ) ) ;
#34137 = EDGE_CURVE ( 'NONE', #16545, #30897, #10720, .T. ) ;
#34138 = CARTESIAN_POINT ( 'NONE',  ( -0.02000000000000000042, -2.183180860297908144, -0.5562760292030870524 ) ) ;
#34140 = EDGE_LOOP ( 'NONE', ( #8248, #18077, #596, #35282 ) ) ;
#34139 = DIRECTION ( 'NONE',  ( 0.8660512985181134660, 0.4999551463232372317, 0.000000000000000000 ) ) ;
#34141 = EDGE_LOOP ( 'NONE', ( #7154, #14359, #18225, #7306, #29652, #3049, #28474, #30007, #22925, #19136 ) ) ;
#34142 = VERTEX_POINT ( 'NONE', #8877 ) ;
#34143 = CARTESIAN_POINT ( 'NONE',  ( 0.04230188431063459237, 0.4429734639576318189, -0.1531098457317254524 ) ) ;
#34144 = ORIENTED_EDGE ( 'NONE', *, *, #33012, .T. ) ;
#34145 = CARTESIAN_POINT ( 'NONE',  ( -0.0007768880743327374406, -0.5529413628073850395, 0.2588803452509780278 ) ) ;
#34147 = CARTESIAN_POINT ( 'NONE',  ( 0.08496507042635949303, -1.314462971446856754, 0.5855767900618368271 ) ) ;
#34146 = CARTESIAN_POINT ( 'NONE',  ( 0.4915260346479126685, -1.695508583366576616, -0.4333519947141558637 ) ) ;
#34148 = CARTESIAN_POINT ( 'NONE',  ( 0.2850999234409680172, -1.647721251208171367, -0.3633777075355690833 ) ) ;
#34149 = CARTESIAN_POINT ( 'NONE',  ( 0.4075534289126498955, -1.705687498146139847, 0.4182417262809068337 ) ) ;
#34151 = ORIENTED_EDGE ( 'NONE', *, *, #18740, .F. ) ;
#34150 = ORIENTED_EDGE ( 'NONE', *, *, #11803, .T. ) ;
#34152 = CARTESIAN_POINT ( 'NONE',  ( 0.4660077270438260921, -1.088784338607927449, -0.4093149438083810154 ) ) ;
#34153 = CARTESIAN_POINT ( 'NONE',  ( 0.3989031518297398993, -1.748978033746103833, -0.4505407471312883882 ) ) ;
#34154 = CARTESIAN_POINT ( 'NONE',  ( -0.02953079040095503774, -0.5250338024619316535, 0.07436286310882278539 ) ) ;
#34155 = CARTESIAN_POINT ( 'NONE',  ( 0.3583355372769085334, -1.108236462397462097, 0.8023416462808365957 ) ) ;
#34156 = DIRECTION ( 'NONE',  ( 1.000000000000000000, 0.000000000000000000, 0.000000000000000000 ) ) ;
#34157 = CARTESIAN_POINT ( 'NONE',  ( 0.2022720587426989902, -1.382578450136434212, 0.9362826073282410899 ) ) ;
#34158 = EDGE_CURVE ( 'NONE', #31681, #40066, #28559, .T. ) ;
#34159 = CARTESIAN_POINT ( 'NONE',  ( 0.2475864609571435671, -1.418823566509069378, 1.026491066079080250 ) ) ;
#34160 = ADVANCED_FACE ( 'NONE', ( #24735 ), #4318, .T. ) ;
#34161 = B_SPLINE_CURVE_WITH_KNOTS ( 'NONE', 3,
 ( #449, #6952, #22829, #35348, #19706, #15812, #22012, #28364, #231, #12725, #25290, #7760, #36140, #13926, #19912, #4058, #23624, #33058 ),
 .UNSPECIFIED., .F., .F.,
 ( 4, 2, 2, 2, 2, 2, 2, 2, 4 ),
 ( 0.000000000000000000, 0.0003722442504740213886, 0.0007444885009480427772, 0.001116732751422064166, 0.001488977001896085554, 0.001861221252370106943, 0.002233465502844128332, 0.002605709753318149503, 0.002977954003792171109 ),
 .UNSPECIFIED. ) ;
#34162 = CARTESIAN_POINT ( 'NONE',  ( 0.8248651029816849167, 2.049759731064160790E-16, 0.6154198107346400271 ) ) ;
#34163 = DIRECTION ( 'NONE',  ( -1.509929076399588311E-31, -0.9849933812516261655, -0.1725921171157266121 ) ) ;
#34164 = EDGE_CURVE ( 'NONE', #553, #34841, #33709, .T. ) ;
#34165 = DIRECTION ( 'NONE',  ( 0.000000000000000000, 0.7071067811865474617, 0.7071067811865474617 ) ) ;
#34166 = DIRECTION ( 'NONE',  ( 0.8660512985181134660, 0.4999551463232371207, 0.000000000000000000 ) ) ;
#34167 =( LENGTH_UNIT ( ) NAMED_UNIT ( * ) SI_UNIT ( $, .METRE. ) );
#34168 = AXIS2_PLACEMENT_3D ( 'NONE', #1636, #10662, #38832 ) ;
#34169 = LINE ( 'NONE', #2516, #5447 ) ;
#34170 = CARTESIAN_POINT ( 'NONE',  ( -8.537024980200822558E-17, -0.6872203660140397963, 0.1457185332388691301 ) ) ;
#34171 = CARTESIAN_POINT ( 'NONE',  ( 0.04158943244807711270, -1.020592330009299609, 0.7078592779458576789 ) ) ;
#34172 = PERSON_AND_ORGANIZATION ( #28500, #32463 ) ;
#34173 = CARTESIAN_POINT ( 'NONE',  ( 0.7220926616001757115, -1.479655736425856682, 0.5682417262808782121 ) ) ;
#34174 = AXIS2_PLACEMENT_3D ( 'NONE', #37727, #34028, #18822 ) ;
#34175 = DIRECTION ( 'NONE',  ( -6.162975822039154730E-33, 0.000000000000000000, -1.000000000000000000 ) ) ;
#34176 = DIRECTION ( 'NONE',  ( 0.01455087616121368381, 0.9998941303972840311, 0.000000000000000000 ) ) ;
#34177 = DIRECTION ( 'NONE',  ( 0.000000000000000000, 3.341771304121709196E-14, -1.000000000000000000 ) ) ;
#34178 = ORIENTED_EDGE ( 'NONE', *, *, #9894, .T. ) ;
#34179 = DIRECTION ( 'NONE',  ( 0.4999999999999983902, 0.8639288552672733656, -0.06022402374949849257 ) ) ;
#34180 = CARTESIAN_POINT ( 'NONE',  ( 0.2316878579425200868, -1.510780966898643385, 0.9085919253409524554 ) ) ;
#34181 = ADVANCED_FACE ( 'NONE', ( #15864, #28412 ), #7186, .T. ) ;
#34182 = ADVANCED_FACE ( 'NONE', ( #3912 ), #3507, .F. ) ;
#34183 = CARTESIAN_POINT ( 'NONE',  ( 0.1349389734390225581, -0.6048227726405104310, 0.3263205089217648402 ) ) ;
#34185 = VERTEX_POINT ( 'NONE', #32293 ) ;
#34184 = CARTESIAN_POINT ( 'NONE',  ( 0.3676072623606497225, -1.734636822330196448, 0.4290806300446088350 ) ) ;
#34186 = CARTESIAN_POINT ( 'NONE',  ( 0.1886295724182434630, -0.6892155111403490686, 0.2012867199884409153 ) ) ;
#34188 = ORIENTED_EDGE ( 'NONE', *, *, #9692, .F. ) ;
#34187 = VERTEX_POINT ( 'NONE', #284 ) ;
#34189 = CARTESIAN_POINT ( 'NONE',  ( 0.6315607611771009156, -1.321640318787267843, 0.7919778341148684397 ) ) ;
#34190 = CARTESIAN_POINT ( 'NONE',  ( 0.3321231534132307872, -1.664232048909226380, -0.6363989157131245689 ) ) ;
#34191 = SPHERICAL_SURFACE ( 'NONE', #37073, 0.01499999999999999944 ) ;
#34192 = APPROVAL_ROLE ( '' ) ;
#34193 = VECTOR ( 'NONE', #7298, 39.37007874015748143 ) ;
#34194 = CARTESIAN_POINT ( 'NONE',  ( 0.1443375672974070711, 0.07999999999999969635, 0.000000000000000000 ) ) ;
#34195 = VERTEX_POINT ( 'NONE', #4108 ) ;
#34196 = CARTESIAN_POINT ( 'NONE',  ( 0.1616880641390656403, -0.8518218427985874142, 0.5517047459742124849 ) ) ;
#34197 = LINE ( 'NONE', #24559, #33206 ) ;
#34198 = CIRCLE ( 'NONE', #22396, 0.01500000000000007057 ) ;
#34199 = CARTESIAN_POINT ( 'NONE',  ( 0.1041061586474624351, -0.5542841090750713073, 0.2004015504623158361 ) ) ;
#34201 = CARTESIAN_POINT ( 'NONE',  ( 0.001101228876466371154, -0.5768926175761717179, 0.01911525350802194614 ) ) ;
#34200 = CARTESIAN_POINT ( 'NONE',  ( 0.3432523969717229395, -1.751972077818550799, 0.4558970387576508076 ) ) ;
#34202 = CARTESIAN_POINT ( 'NONE',  ( 0.007701696793370658295, -0.9976095849859260012, 0.4998176050132062120 ) ) ;
#34203 = ORIENTED_EDGE ( 'NONE', *, *, #17428, .F. ) ;
#34204 = CIRCLE ( 'NONE', #11889, 0.1033070866141732325 ) ;
#34205 = CARTESIAN_POINT ( 'NONE',  ( -0.02000000000000000042, -2.183180860297908144, -0.4937760292030871079 ) ) ;
#34206 = CARTESIAN_POINT ( 'NONE',  ( 0.2810522391648209162, -0.7111171087874781360, 0.6409053233574648623 ) ) ;
#34207 = CARTESIAN_POINT ( 'NONE',  ( 0.4654635148381854326, -1.611437027087300855, -0.6524167923582313566 ) ) ;
#34208 = CYLINDRICAL_SURFACE ( 'NONE', #24585, 0.1849999999999994982 ) ;
#34209 = ADVANCED_FACE ( 'NONE', ( #12781 ), #16470, .T. ) ;
#34210 = CARTESIAN_POINT ( 'NONE',  ( 0.3798561561205663351, -1.154581612852501715, 0.4182417262808776903 ) ) ;
#34211 = CARTESIAN_POINT ( 'NONE',  ( 0.0005143298144824101203, -1.951520895201868111, -0.6590200376447251651 ) ) ;
#34212 = CARTESIAN_POINT ( 'NONE',  ( 0.3234561073823307709, -1.180921653228079737, 0.5535308386742264775 ) ) ;
#34213 = CARTESIAN_POINT ( 'NONE',  ( 0.5179624304041525740, -1.133452979592703302, 0.6716967517830890744 ) ) ;
#34214 = APPROVAL_ROLE ( '' ) ;
#34215 = CARTESIAN_POINT ( 'NONE',  ( 0.4758903444788569193, -1.092184862719652205, -0.4175441261731758780 ) ) ;
#34216 = AXIS2_PLACEMENT_3D ( 'NONE', #14164, #39453, #23646 ) ;
#34217 = CARTESIAN_POINT ( 'NONE',  ( 0.2349883165480021185, -1.593155449794408485, -0.6704283676663660430 ) ) ;
#34218 = CARTESIAN_POINT ( 'NONE',  ( 0.4004575997975503565, -1.713586824669576902, 0.4219389359880015289 ) ) ;
#34219 =( REPRESENTATION_RELATIONSHIP ('NONE','NONE', #27514, #35919 ) REPRESENTATION_RELATIONSHIP_WITH_TRANSFORMATION ( #22285 )SHAPE_REPRESENTATION_RELATIONSHIP( ) );
#34220 = CARTESIAN_POINT ( 'NONE',  ( 2.915087563824520997E-32, -9.793929126999060983E-17, -0.2149999999999999967 ) ) ;
#34221 = CIRCLE ( 'NONE', #17143, 0.1033070866141732880 ) ;
#34222 =( BOUNDED_SURFACE ( )  B_SPLINE_SURFACE ( 3, 2, ( 
 ( #11958, #18338, #23922 ),
 ( #8262, #8656, #33766 ),
 ( #20835, #30883, #11569 ),
 ( #24523, #11151, #23709 ),
 ( #5578, #33357, #15051 ),
 ( #1911, #39940, #8874 ),
 ( #30264, #15249, #2094 ),
 ( #18137, #14631, #11758 ),
 ( #37053, #27203, #24133 ),
 ( #33164, #17919, #8459 ),
 ( #21023, #4967, #2702 ),
 ( #36840, #30693, #39329 ) ),
 .UNSPECIFIED., .F., .F., .F. ) 
 B_SPLINE_SURFACE_WITH_KNOTS ( ( 4, 2, 2, 2, 2, 4 ),
 ( 3, 3 ),
 ( -1.965116437629976787E-19, 0.0002905500556263221671, 0.0005811001112526445510, 0.001162200222505289319, 0.001743300333757933978, 0.002324400445010578638 ),
 ( 0.000000000000000000, 1.000000000000000000 ),
 .UNSPECIFIED. ) 
 GEOMETRIC_REPRESENTATION_ITEM ( )  RATIONAL_B_SPLINE_SURFACE ( (
 ( 1.000000000000000000, 0.3554223140987168850, 1.000000000000000000),
 ( 1.000000000000000000, 0.3781116103073136059, 1.000000000000000000),
 ( 1.000000000000000000, 0.4049359264755946763, 1.000000000000000000),
 ( 1.000000000000000000, 0.4598140129575411517, 1.000000000000000000),
 ( 1.000000000000000000, 0.4879366426973186788, 1.000000000000000000),
 ( 1.000000000000000000, 0.5702646001839052348, 1.000000000000000000),
 ( 1.000000000000000000, 0.6198565573272236673, 1.000000000000000000),
 ( 1.000000000000000000, 0.7059671795725417365, 1.000000000000000000),
 ( 1.000000000000000000, 0.7435989477609952214, 1.000000000000000000),
 ( 1.000000000000000000, 0.8093167251978203858, 1.000000000000000000),
 ( 1.000000000000000000, 0.8374450039889510533, 1.000000000000000000),
 ( 1.000000000000000000, 0.8603775106309528020, 1.000000000000000000) ) ) 
 REPRESENTATION_ITEM ( '' )  SURFACE ( )  );
#34223 = ORIENTED_EDGE ( 'NONE', *, *, #9989, .F. ) ;
#34224 = CARTESIAN_POINT ( 'NONE',  ( 0.4364024856657339191, -1.140120363169106588, 0.4343543486376312823 ) ) ;
#34225 = CIRCLE ( 'NONE', #14526, 0.01000000000000002970 ) ;
#34226 = FACE_OUTER_BOUND ( 'NONE', #12429, .T. ) ;
#34227 = CIRCLE ( 'NONE', #13867, 0.01499999999999997689 ) ;
#34228 = FACE_OUTER_BOUND ( 'NONE', #30055, .T. ) ;
#34229 = ORIENTED_EDGE ( 'NONE', *, *, #29180, .F. ) ;
#34230 = CARTESIAN_POINT ( 'NONE',  ( -0.01899468245561950625, 0.07378005917298446903, -0.5147132347679479469 ) ) ;
#34231 = CARTESIAN_POINT ( 'NONE',  ( 0.1105865011551944721, -1.209543234154132341, 0.7561629657869882726 ) ) ;
#34233 = EDGE_LOOP ( 'NONE', ( #9664, #25311, #5838, #21966 ) ) ;
#34232 = EDGE_LOOP ( 'NONE', ( #6035, #6112, #36825 ) ) ;
#34234 = CARTESIAN_POINT ( 'NONE',  ( 0.3186320389496528627, -1.760431904683431359, 0.5682417262808792113 ) ) ;
#34235 = VERTEX_POINT ( 'NONE', #31700 ) ;
#34236 = DIRECTION ( 'NONE',  ( -0.4999551463232311255, 0.8660512985181170187, 0.000000000000000000 ) ) ;
#34237 = CARTESIAN_POINT ( 'NONE',  ( 0.04157143636675252052, -0.4522154923419796080, -0.1290233296939804764 ) ) ;
#34238 = CARTESIAN_POINT ( 'NONE',  ( 0.3666869875394455636, -1.756572920003051541, -0.3440370208071864000 ) ) ;
#34239 = CARTESIAN_POINT ( 'NONE',  ( -2.128333683970191216E-14, -2.097675824466503691, -0.2907100122647986451 ) ) ;
#34241 = FACE_OUTER_BOUND ( 'NONE', #35171, .T. ) ;
#34240 = CARTESIAN_POINT ( 'NONE',  ( 0.05999999999999990757, 0.000000000000000000, 0.000000000000000000 ) ) ;
#34242 = DIRECTION ( 'NONE',  ( -7.771561172376107616E-16, 7.170354002788761615E-17, -1.000000000000000000 ) ) ;
#34243 = VERTEX_POINT ( 'NONE', #9485 ) ;
#34244 = FACE_OUTER_BOUND ( 'NONE', #27567, .T. ) ;
#34245 = EDGE_LOOP ( 'NONE', ( #18446, #948, #38749 ) ) ;
#34246 = FACE_OUTER_BOUND ( 'NONE', #19825, .T. ) ;
#34247 = CARTESIAN_POINT ( 'NONE',  ( 0.3840491615834836225, -1.381380984370014442, 0.8560923923499079713 ) ) ;
#34249 = CARTESIAN_POINT ( 'NONE',  ( 0.5656120792695429333, -1.615920895601612228, 0.4892587525384312630 ) ) ;
#34248 = CARTESIAN_POINT ( 'NONE',  ( 5.463695987328526437E-16, -0.2899999999999993694, -7.171100983368691195E-16 ) ) ;
#34250 = CARTESIAN_POINT ( 'NONE',  ( 0.4262438152663738933, -1.592651821845863402, -0.6151431148613257793 ) ) ;
#34251 = DIRECTION ( 'NONE',  ( 0.000000000000000000, -0.5295275951190198116, -0.8482927124568896415 ) ) ;
#34252 = AXIS2_PLACEMENT_3D ( 'NONE', #39507, #23696, #15039 ) ;
#34253 = CARTESIAN_POINT ( 'NONE',  ( 0.3964264789023509428, -1.761207211030865194, -0.3116577597928051890 ) ) ;
#34254 = CARTESIAN_POINT ( 'NONE',  ( 0.1254727147607625215, -0.5505682354593325334, 0.1615710687873511131 ) ) ;
#34255 = CARTESIAN_POINT ( 'NONE',  ( 0.4747166437277507978, -1.681399074042227770, 0.5637963070471054827 ) ) ;
#34256 = CARTESIAN_POINT ( 'NONE',  ( 0.3792944791200489885, -1.718975934191981469, 0.4318151841061548257 ) ) ;
#34257 = CIRCLE ( 'NONE', #4668, 0.7750185148639454624 ) ;
#34258 = LINE ( 'NONE', #33651, #38246 ) ;
#34259 = CARTESIAN_POINT ( 'NONE',  ( 0.2207803211308198288, -1.228036517901200719, 0.5094220132429284620 ) ) ;
#34260 = AXIS2_PLACEMENT_3D ( 'NONE', #35306, #16580, #7291 ) ;
#34261 = CARTESIAN_POINT ( 'NONE',  ( 0.2206336596962433783, -1.239453910453733876, 0.5669030946385860137 ) ) ;
#34262 = DIRECTION ( 'NONE',  ( 0.8660512985181135770, 0.4999551463232370652, 0.000000000000000000 ) ) ;
#34263 = EDGE_CURVE ( 'NONE', #35870, #5559, #4798, .T. ) ;
#34264 = EDGE_CURVE ( 'NONE', #4481, #30904, #15980, .T. ) ;
#34265 = CARTESIAN_POINT ( 'NONE',  ( 0.2954936729740054724, -0.7648845942614268534, 0.6619870385404000857 ) ) ;
#34266 = EDGE_CURVE ( 'NONE', #7711, #25042, #921, .T. ) ;
#34267 = CARTESIAN_POINT ( 'NONE',  ( -0.04085667396267504692, 0.2598928711944307746, 0.3937292009461436648 ) ) ;
#34268 = CARTESIAN_POINT ( 'NONE',  ( 0.3264244126186546802, -1.294301107126978767, -0.5166151207188711680 ) ) ;
#34269 = ADVANCED_FACE ( 'NONE', ( #7390 ), #8514, .F. ) ;
#34270 = CARTESIAN_POINT ( 'NONE',  ( 0.6184362100440952137, -1.564428388872008746, -0.4403698313141179432 ) ) ;
#34271 = CARTESIAN_POINT ( 'NONE',  ( 0.1866832830560181955, -0.7995344403538681144, 0.2774612360649313936 ) ) ;
#34272 = CARTESIAN_POINT ( 'NONE',  ( 0.02999999999997886302, -2.107936428766274073, -0.2870436526301869962 ) ) ;
#34273 = EDGE_CURVE ( 'NONE', #24540, #3369, #10818, .T. ) ;
#34274 = CARTESIAN_POINT ( 'NONE',  ( 0.01548846960712814240, 0.2450655194479464116, -0.4674710490748144043 ) ) ;
#34275 = CARTESIAN_POINT ( 'NONE',  ( -0.3000000000000000999, -2.853330612949663170, -0.6088139570729240724 ) ) ;
#34276 = ORIENTED_EDGE ( 'NONE', *, *, #1612, .F. ) ;
#34277 = CYLINDRICAL_SURFACE ( 'NONE', #40370, 0.03000000000000008910 ) ;
#34278 = CARTESIAN_POINT ( 'NONE',  ( 0.4057297589136773519, -1.717105997358977065, -0.6044639876195223582 ) ) ;
#34279 = CARTESIAN_POINT ( 'NONE',  ( 0.6579514796806046339, -1.538074113211328697, 0.4238364680776416371 ) ) ;
#34280 = AXIS2_PLACEMENT_3D ( 'NONE', #6730, #16224, #28560 ) ;
#34281 = CARTESIAN_POINT ( 'NONE',  ( 0.5344271610666608829, -1.636795983080443051, -0.4842394454172543328 ) ) ;
#34282 = CARTESIAN_POINT ( 'NONE',  ( 0.1323301854973741309, -1.244705972311918263, -0.5155029497116575543 ) ) ;
#34283 = ORIENTED_EDGE ( 'NONE', *, *, #36099, .F. ) ;
#34284 = DIRECTION ( 'NONE',  ( 0.4999999999999963918, 0.000000000000000000, -0.8660254037844405950 ) ) ;
#34285 = VECTOR ( 'NONE', #6005, 39.37007874015748143 ) ;
#34286 = AXIS2_PLACEMENT_3D ( 'NONE', #10092, #22668, #16464 ) ;
#34287 = EDGE_CURVE ( 'NONE', #13090, #5913, #27818, .T. ) ;
#34288 = CARTESIAN_POINT ( 'NONE',  ( 0.3738069751030371757, -1.122463183855469948, 0.6233846043333758358 ) ) ;
#34289 = CARTESIAN_POINT ( 'NONE',  ( 0.3249483201304784741, -1.768002432019315728, 0.5182417262812728520 ) ) ;
#34290 = APPLIED_DATE_AND_TIME_ASSIGNMENT ( #12518, #36509, ( #17414 ) ) ;
#34291 = CARTESIAN_POINT ( 'NONE',  ( 0.05279755784604157898, 0.2420637527537952693, -0.4010259520538080324 ) ) ;
#34292 = CARTESIAN_POINT ( 'NONE',  ( 0.4303872151682832659, -1.189052686049667074, 0.7234122301098351304 ) ) ;
#34294 = ORIENTED_EDGE ( 'NONE', *, *, #5528, .F. ) ;
#34293 = DIRECTION ( 'NONE',  ( 0.000000000000000000, -3.330669073875470114E-16, -1.000000000000000000 ) ) ;
#34295 = CARTESIAN_POINT ( 'NONE',  ( 0.4430687885351943245, -1.051147784193108281, 0.6535119922057798236 ) ) ;
#34296 = ORIENTED_EDGE ( 'NONE', *, *, #38119, .F. ) ;
#34297 = PERSON_AND_ORGANIZATION_ROLE ( 'design_supplier' ) ;
#34298 = FACE_OUTER_BOUND ( 'NONE', #29605, .T. ) ;
#34299 = ORIENTED_EDGE ( 'NONE', *, *, #32108, .F. ) ;
#34300 = ORIENTED_EDGE ( 'NONE', *, *, #447, .F. ) ;
#34301 = CARTESIAN_POINT ( 'NONE',  ( 0.1289379552302614418, -0.9164046769963616335, 0.7560741064833712555 ) ) ;
#34303 = CARTESIAN_POINT ( 'NONE',  ( 0.1749985090116134290, -0.8722846205208456549, 0.008124829994509464443 ) ) ;
#34302 = CARTESIAN_POINT ( 'NONE',  ( 0.06626660213556555268, -0.7348254893761211326, 0.005522339898145539085 ) ) ;
#34304 = CARTESIAN_POINT ( 'NONE',  ( 0.4560259861529415981, -1.119845760975095139, -0.4237974160008213809 ) ) ;
#34305 = ORIENTED_EDGE ( 'NONE', *, *, #32364, .T. ) ;
#34306 = ORIENTED_EDGE ( 'NONE', *, *, #29769, .T. ) ;
#34307 = CARTESIAN_POINT ( 'NONE',  ( 0.3620239859624554968, -1.000756814187188315, 0.6096560215957895768 ) ) ;
#34308 = CARTESIAN_POINT ( 'NONE',  ( 0.5529025669954783506, -1.511171647080765679, 0.5718623976496952643 ) ) ;
#34309 = ORIENTED_EDGE ( 'NONE', *, *, #14738, .T. ) ;
#34310 = CARTESIAN_POINT ( 'NONE',  ( 0.2860007606812444703, -1.398056877809351839, -0.3144976166544465324 ) ) ;
#34311 = CARTESIAN_POINT ( 'NONE',  ( 0.03113248654051816583, -0.03575622569115821658, -0.2978615321325044363 ) ) ;
#34312 = CARTESIAN_POINT ( 'NONE',  ( -2.031982644102707652E-14, -2.061923090639281586, -0.3032530188522716830 ) ) ;
#34313 = AXIS2_PLACEMENT_3D ( 'NONE', #36388, #39674, #2256 ) ;
#34314 = CARTESIAN_POINT ( 'NONE',  ( 0.5994069634879333197, -1.482972712863466436, -0.4086340618636334909 ) ) ;
#34315 = DIRECTION ( 'NONE',  ( 0.4441145778363653207, 0.000000000000000000, -0.8959700004761470549 ) ) ;
#34316 = ADVANCED_FACE ( 'NONE', ( #28774 ), #32, .T. ) ;
#34317 = CIRCLE ( 'NONE', #16585, 0.5400000000000012568 ) ;
#34318 = FACE_OUTER_BOUND ( 'NONE', #37275, .T. ) ;
#34319 = CIRCLE ( 'NONE', #32992, 0.7043128707267513056 ) ;
#34320 = CARTESIAN_POINT ( 'NONE',  ( 0.1438259253235277535, -1.251381717279140160, 0.6230599517298043288 ) ) ;
#34321 = CARTESIAN_POINT ( 'NONE',  ( 0.2397041043040182284, -1.887673249773291095, -0.6585554176240054902 ) ) ;
#34322 = DIRECTION ( 'NONE',  ( -7.771561172376107616E-16, 7.170354002788761615E-17, -1.000000000000000000 ) ) ;
#34323 = DATE_TIME_ROLE ( 'creation_date' ) ;
#34324 = VECTOR ( 'NONE', #36814, 39.37007874015748854 ) ;
#34325 = EDGE_CURVE ( 'NONE', #11991, #17796, #15336, .T. ) ;
#34326 = CARTESIAN_POINT ( 'NONE',  ( 0.3611884512188844321, -1.010424417365897831, 0.6143157383772529512 ) ) ;
#34327 = CARTESIAN_POINT ( 'NONE',  ( 0.4839995430037176138, -1.120831722135291697, 0.5371002527360760892 ) ) ;
#34328 = EDGE_CURVE ( 'NONE', #10938, #20043, #25273, .T. ) ;
#34329 = CARTESIAN_POINT ( 'NONE',  ( 0.4374001795570605089, -1.230147717240742677, 0.6057417262809753344 ) ) ;
#34330 = CARTESIAN_POINT ( 'NONE',  ( 0.5617906032868313915, -1.585432954525022531, -0.5313147025850599725 ) ) ;
#34331 = CARTESIAN_POINT ( 'NONE',  ( -0.003124719664520048124, -0.8057675726412016903, 0.1457185332388697963 ) ) ;
#34332 = CARTESIAN_POINT ( 'NONE',  ( -0.07999999999999998779, -2.004218822785767795, -0.4035264592197354561 ) ) ;
#34333 = DIRECTION ( 'NONE',  ( 0.4999551463232372317, -0.8660512985181135770, 0.000000000000000000 ) ) ;
#34334 = CARTESIAN_POINT ( 'NONE',  ( 0.3792114031565354537, -1.610124904551262226, 0.4986251887174527608 ) ) ;
#34335 = ORIENTED_EDGE ( 'NONE', *, *, #38819, .F. ) ;
#34336 = ORIENTED_EDGE ( 'NONE', *, *, #16281, .T. ) ;
#34337 = ADVANCED_FACE ( 'NONE', ( #3473 ), #25906, .F. ) ;
#34338 = CARTESIAN_POINT ( 'NONE',  ( -0.1056392956507359038, -0.4804620820570907891, 0.09550516425342367444 ) ) ;
#34339 = ORIENTED_EDGE ( 'NONE', *, *, #31499, .T. ) ;
#34340 = FACE_OUTER_BOUND ( 'NONE', #8998, .T. ) ;
#34341 = CARTESIAN_POINT ( 'NONE',  ( -0.05561176441985789948, -0.4316390549698244650, -0.1616802657107529184 ) ) ;
#34342 = AXIS2_PLACEMENT_3D ( 'NONE', #28501, #15743, #7439 ) ;
#34343 = DIRECTION ( 'NONE',  ( -0.4999999999999970024, 0.000000000000000000, 0.8660254037844403729 ) ) ;
#34345 = ORIENTED_EDGE ( 'NONE', *, *, #12815, .F. ) ;
#34344 = CARTESIAN_POINT ( 'NONE',  ( 0.01018941234914808383, -0.5369207985381054815, 0.09707054648710758404 ) ) ;
#34346 = VERTEX_POINT ( 'NONE', #9837 ) ;
#34347 = CARTESIAN_POINT ( 'NONE',  ( 0.01895884884825246863, 0.4667865995382938227, -0.2292744456225718208 ) ) ;
#34348 = AXIS2_PLACEMENT_3D ( 'NONE', #34268, #36559, #11666 ) ;
#34349 = ORIENTED_EDGE ( 'NONE', *, *, #24543, .T. ) ;
#34350 = AXIS2_PLACEMENT_3D ( 'NONE', #6691, #980, #19471 ) ;
#34351 = CARTESIAN_POINT ( 'NONE',  ( 0.1390698109426623252, -1.062601491521927288, 0.8567851293273262003 ) ) ;
#34353 = CARTESIAN_POINT ( 'NONE',  ( 0.1093547303742859189, -1.269651521606318889, 0.6004988576366063757 ) ) ;
#34352 = CARTESIAN_POINT ( 'NONE',  ( 0.3951243486924778114, -1.180114500222565033, 0.7033046486683809384 ) ) ;
#34354 = DIRECTION ( 'NONE',  ( 0.4999551463232373427, -0.8660512985181134660, 0.000000000000000000 ) ) ;
#34355 = VECTOR ( 'NONE', #32709, 39.37007874015748143 ) ;
#34356 = DIRECTION ( 'NONE',  ( -1.000000000000000000, -1.188678714063518030E-15, -1.779758311459931231E-16 ) ) ;
#34358 = VERTEX_POINT ( 'NONE', #15620 ) ;
#34357 = ORIENTED_EDGE ( 'NONE', *, *, #28577, .T. ) ;
#34359 = DIRECTION ( 'NONE',  ( 0.000000000000000000, 0.8438867430782092116, 0.5365213554527465956 ) ) ;
#34360 = DIRECTION ( 'NONE',  ( 0.8660512985181135770, 0.4999551463232370652, 0.000000000000000000 ) ) ;
#34361 = DIRECTION ( 'NONE',  ( 1.000000000000000000, 0.000000000000000000, 0.000000000000000000 ) ) ;
#34362 = CARTESIAN_POINT ( 'NONE',  ( 0.5161999997979804800, -1.324679096059732331, 0.7828784074225845213 ) ) ;
#34363 = VECTOR ( 'NONE', #25481, 39.37007874015748143 ) ;
#34364 = CARTESIAN_POINT ( 'NONE',  ( 0.01548846960707528191, 0.3772621329472709006, 0.3651003739303413931 ) ) ;
#34365 = CARTESIAN_POINT ( 'NONE',  ( 0.1870037891866919988, -0.7120005297123722654, 0.07613086658547316143 ) ) ;
#34366 = CARTESIAN_POINT ( 'NONE',  ( 0.3228554848850782033, -1.719965048204380231, 0.8062249495306545999 ) ) ;
#34367 = CARTESIAN_POINT ( 'NONE',  ( 0.01548846960707582834, 0.4770632572900484480, 0.2530032579707400253 ) ) ;
#34368 = EDGE_CURVE ( 'NONE', #26308, #26277, #28168, .T. ) ;
#34369 = FACE_OUTER_BOUND ( 'NONE', #4392, .T. ) ;
#34370 = CARTESIAN_POINT ( 'NONE',  ( 0.4465751558565839163, -1.208568754259124800, 0.6870635310481745250 ) ) ;
#34371 = LINE ( 'NONE', #5782, #29937 ) ;
#34372 = B_SPLINE_CURVE_WITH_KNOTS ( 'NONE', 3,
 ( #39468, #33302, #17476, #7597, #5109, #1453 ),
 .UNSPECIFIED., .F., .F.,
 ( 4, 2, 4 ),
 ( 0.000000000000000000, 0.0005460346488701544763, 0.001092069297740308953 ),
 .UNSPECIFIED. ) ;
#34373 = CIRCLE ( 'NONE', #32363, 0.03000000000000029379 ) ;
#34374 = EDGE_CURVE ( 'NONE', #2583, #35372, #15522, .T. ) ;
#34375 = CARTESIAN_POINT ( 'NONE',  ( 0.04760578872587302446, -0.2475315945985540611, 0.4138583970464106421 ) ) ;
#34376 = CARTESIAN_POINT ( 'NONE',  ( 3.414809992080329023E-17, -0.4262518876079541830, 0.1639910581422319991 ) ) ;
#34377 = CARTESIAN_POINT ( 'NONE',  ( 0.03538878874458249030, -0.9945019241485085759, 0.6847322700004405682 ) ) ;
#34378 = CALENDAR_DATE ( 2026, 13, 10 ) ;
#34379 = AXIS2_PLACEMENT_3D ( 'NONE', #27920, #11673, #36752 ) ;
#34380 = CARTESIAN_POINT ( 'NONE',  ( 0.7218807932984940834, -1.475040712527332376, 0.6299232363116300526 ) ) ;
#34381 = TOROIDAL_SURFACE ( 'NONE', #5468, 0.04749999999977554815, 0.01000000000000000021 ) ;
#34382 = EDGE_CURVE ( 'NONE', #20992, #17702, #16087, .T. ) ;
#34383 = DIRECTION ( 'NONE',  ( 0.000000000000000000, -0.8438867430782093226, -0.5365213554527464845 ) ) ;
#34384 = CARTESIAN_POINT ( 'NONE',  ( 0.6754612668510717732, -1.566418238229341897, 0.6053376557078533615 ) ) ;
#34385 = CARTESIAN_POINT ( 'NONE',  ( 0.5333644791322821321, -1.633651814608773734, -0.5988298493401544853 ) ) ;
#34386 = AXIS2_PLACEMENT_3D ( 'NONE', #23982, #2561, #2762 ) ;
#34387 = EDGE_CURVE ( 'NONE', #34142, #30939, #3585, .T. ) ;
#34388 = DIRECTION ( 'NONE',  ( -1.510243460696184176E-15, 0.000000000000000000, -1.000000000000000000 ) ) ;
#34389 = ORIENTED_EDGE ( 'NONE', *, *, #7930, .F. ) ;
#34390 = DIRECTION ( 'NONE',  ( 0.000000000000000000, -3.885780586188049371E-16, -1.000000000000000000 ) ) ;
#34391 = CARTESIAN_POINT ( 'NONE',  ( 0.2400417667449158410, -1.530793041395833720, 0.9076943226153151301 ) ) ;
#34392 = EDGE_CURVE ( 'NONE', #11216, #35098, #28573, .T. ) ;
#34393 = CARTESIAN_POINT ( 'NONE',  ( 0.1313096082175202184, -0.5612069155677682497, 0.2075466349573875935 ) ) ;
#34395 = ORIENTED_EDGE ( 'NONE', *, *, #33823, .T. ) ;
#34394 = CARTESIAN_POINT ( 'NONE',  ( 0.1614670899430008522, -0.7569536277469717245, 0.1022936816274460647 ) ) ;
#34396 = EDGE_CURVE ( 'NONE', #36370, #16052, #37652, .T. ) ;
#34397 = CARTESIAN_POINT ( 'NONE',  ( 0.2393369856776542404, -0.7683812882957752333, 0.4887749849253086309 ) ) ;
#34399 = ORIENTED_EDGE ( 'NONE', *, *, #6993, .F. ) ;
#34398 = EDGE_LOOP ( 'NONE', ( #27621, #17009, #26623, #26180, #32033, #30615 ) ) ;
#34400 = CARTESIAN_POINT ( 'NONE',  ( 0.5213874123744923761, -1.147839253744530774, 0.8164622333705154889 ) ) ;
#34401 = EDGE_CURVE ( 'NONE', #10078, #34849, #11397, .T. ) ;
#34402 = CARTESIAN_POINT ( 'NONE',  ( 0.04582713223189471829, 0.4389429380065681952, -0.2108029774974885806 ) ) ;
#34403 = DIRECTION ( 'NONE',  ( 0.000000000000000000, -0.9510565162951458706, 0.3090169943749713766 ) ) ;
#34404 = AXIS2_PLACEMENT_3D ( 'NONE', #35261, #28684, #19434 ) ;
#34405 = CARTESIAN_POINT ( 'NONE',  ( 0.3186308459106851343, -1.760406140419759069, 0.5654457401203095701 ) ) ;
#34406 = ORIENTED_EDGE ( 'NONE', *, *, #8112, .T. ) ;
#34407 = CARTESIAN_POINT ( 'NONE',  ( 0.1503728836000403912, -0.8245688327091527103, 0.5282395445164650427 ) ) ;
#34408 = CIRCLE ( 'NONE', #8768, 0.1033070866141732325 ) ;
#34409 = CARTESIAN_POINT ( 'NONE',  ( 0.3567375191406563784, -1.622233719184205336, -0.3666517953721947776 ) ) ;
#34410 = AXIS2_PLACEMENT_3D ( 'NONE', #38236, #22639, #22427 ) ;
#34411 = CARTESIAN_POINT ( 'NONE',  ( 0.5201261370170202625, -1.511049808878615952, 0.6955162974028021861 ) ) ;
#34412 = DIRECTION ( 'NONE',  ( 1.000000000000000000, 0.000000000000000000, 0.000000000000000000 ) ) ;
#34413 = CARTESIAN_POINT ( 'NONE',  ( -0.1710642718812869778, 0.4986889572247778513, 0.1528658435937169657 ) ) ;
#34414 = VERTEX_POINT ( 'NONE', #7140 ) ;
#34415 = CARTESIAN_POINT ( 'NONE',  ( 0.4665252869708542138, -1.674583161905657702, 0.5704180265848416420 ) ) ;
#34416 = CARTESIAN_POINT ( 'NONE',  ( 0.6759764701317674263, -1.395871262418312497, 0.8266306626867110374 ) ) ;
#34417 = AXIS2_PLACEMENT_3D ( 'NONE', #2474, #15010, #11916 ) ;
#34418 = CARTESIAN_POINT ( 'NONE',  ( 0.5965761245944036784, -1.493465029535157029, 0.5182417262812423209 ) ) ;
#34419 = CIRCLE ( 'NONE', #30461, 0.1000000000000000194 ) ;
#34420 = DIRECTION ( 'NONE',  ( 0.000000000000000000, 2.964295475749157234E-14, 1.000000000000000000 ) ) ;
#34421 = EDGE_CURVE ( 'NONE', #11729, #10550, #34161, .T. ) ;
#34422 = CARTESIAN_POINT ( 'NONE',  ( 0.2321526281619643584, -1.233007205928619232, 0.3667417262808778111 ) ) ;
#34423 = FACE_OUTER_BOUND ( 'NONE', #9953, .T. ) ;
#34424 = EDGE_CURVE ( 'NONE', #15629, #22311, #21278, .T. ) ;
#34425 = CARTESIAN_POINT ( 'NONE',  ( -0.05464101615137769569, -2.070343076906777213, -0.2454056712452573896 ) ) ;
#34426 = CARTESIAN_POINT ( 'NONE',  ( 0.2195574306699510647, -0.7404155031343288007, 0.4240249586596535059 ) ) ;
#34427 = APPLICATION_PROTOCOL_DEFINITION ( 'international standard', 'automotive_design', 2000, #28459 ) ;
#34428 = CARTESIAN_POINT ( 'NONE',  ( 0.4688459138424372341, -1.061988423737608045, -0.4248180574663140141 ) ) ;
#34429 = CARTESIAN_POINT ( 'NONE',  ( -0.08000000000000000167, -2.058305985490972212, -0.5970033804171128722 ) ) ;
#34430 = CARTESIAN_POINT ( 'NONE',  ( -0.04139678531769536846, -0.01699044972118052277, 0.4702883835734110729 ) ) ;
#34431 = VECTOR ( 'NONE', #782, 39.37007874015748143 ) ;
#34432 = AXIS2_PLACEMENT_3D ( 'NONE', #23595, #35496, #4239 ) ;
#34433 = EDGE_LOOP ( 'NONE', ( #13994, #7819, #14960, #7631, #25598, #1482 ) ) ;
#34434 = CARTESIAN_POINT ( 'NONE',  ( 0.4879674388967786824, -1.124945552576106289, 0.5170992273679249074 ) ) ;
#34435 = AXIS2_PLACEMENT_3D ( 'NONE', #9879, #19372, #16278 ) ;
#34436 = DIRECTION ( 'NONE',  ( -2.686534417925915961E-31, 0.5877852522924640333, -0.8090169943749540016 ) ) ;
#34437 = CARTESIAN_POINT ( 'NONE',  ( 0.08927640104142192667, -0.5804883439722833272, 0.08457828714984440277 ) ) ;
#34438 = VERTEX_POINT ( 'NONE', #26712 ) ;
#34439 = CARTESIAN_POINT ( 'NONE',  ( -0.04211812644076821238, -0.008544267401287195668, -0.4689465636496595313 ) ) ;
#34440 = AXIS2_PLACEMENT_3D ( 'NONE', #4796, #20673, #14280 ) ;
#34441 = CARTESIAN_POINT ( 'NONE',  ( 0.1177782521778383135, -1.233918990886516465, 0.7507158840856879012 ) ) ;
#34443 = ORIENTED_EDGE ( 'NONE', *, *, #17925, .T. ) ;
#34442 = ORIENTED_EDGE ( 'NONE', *, *, #9958, .T. ) ;
#34444 = CARTESIAN_POINT ( 'NONE',  ( 0.2209956536232957902, -1.227897296991992793, 0.5182417262820130377 ) ) ;
#34445 = AXIS2_PLACEMENT_3D ( 'NONE', #12015, #28066, #24574 ) ;
#34446 = ORIENTED_EDGE ( 'NONE', *, *, #40466, .T. ) ;
#34447 = DIRECTION ( 'NONE',  ( 0.000000000000000000, 0.000000000000000000, -1.000000000000000000 ) ) ;
#34448 = B_SPLINE_CURVE_WITH_KNOTS ( 'NONE', 3,
 ( #20619, #17525, #27409, #11143 ),
 .UNSPECIFIED., .F., .F.,
 ( 4, 4 ),
 ( -6.000000000378846861E-08, 0.001468701496818329089 ),
 .UNSPECIFIED. ) ;
#34449 = CARTESIAN_POINT ( 'NONE',  ( 0.3636045566369612292, -1.982526720389788721, -0.3214018419552013839 ) ) ;
#34450 = CARTESIAN_POINT ( 'NONE',  ( 0.3711181956551158900, -1.768536140287003011, -0.5764455761630662423 ) ) ;
#34452 = CARTESIAN_POINT ( 'NONE',  ( -0.01548846960707517956, -0.2306506793134033284, -0.4716198300880336536 ) ) ;
#34451 = DIRECTION ( 'NONE',  ( 0.000000000000000000, 0.9343694307158671997, -0.3563057211773426602 ) ) ;
#34453 = CARTESIAN_POINT ( 'NONE',  ( 0.7053080889764471451, -1.513942001867420339, 0.5667347313869608438 ) ) ;
#34454 = ORIENTED_EDGE ( 'NONE', *, *, #20859, .F. ) ;
#34455 = CARTESIAN_POINT ( 'NONE',  ( 0.1302229724485401419, -0.6987652251196058151, 0.4850897968509496616 ) ) ;
#34456 = VERTEX_POINT ( 'NONE', #17225 ) ;
#34457 = CARTESIAN_POINT ( 'NONE',  ( 0.05283094505689992643, 0.03968992937477589661, 0.4666439588235274938 ) ) ;
#34458 = CARTESIAN_POINT ( 'NONE',  ( 0.07393562383578071440, -0.5614078526008612346, 0.2422426369645085398 ) ) ;
#34460 = CARTESIAN_POINT ( 'NONE',  ( 0.5960294191658490615, -1.609979221294132179, 0.4458189870587250803 ) ) ;
#34459 = CARTESIAN_POINT ( 'NONE',  ( -0.02953079040095707777, -0.5250338024619264354, 0.07436286310882474215 ) ) ;
#34461 = CARTESIAN_POINT ( 'NONE',  ( 0.4208456803029674287, -1.590742843837566811, -0.4148738790983051428 ) ) ;
#34462 = CARTESIAN_POINT ( 'NONE',  ( 0.1771372480334198196, -0.9211842106723756585, 0.2626135244724711049 ) ) ;
#34463 = VECTOR ( 'NONE', #12392, 39.37007874015748854 ) ;
#34464 = DIRECTION ( 'NONE',  ( 8.881784197001246407E-16, -2.361472542561082612E-16, 1.000000000000000000 ) ) ;
#34465 = CARTESIAN_POINT ( 'NONE',  ( 0.4018863715143964899, -1.731540629620808680, -0.3052291807102240906 ) ) ;
#34466 = VECTOR ( 'NONE', #6936, 39.37007874015748143 ) ;
#34467 = CARTESIAN_POINT ( 'NONE',  ( 0.1397689641161724283, -0.6337347103700835538, 0.3872242776158923427 ) ) ;
#34468 = CARTESIAN_POINT ( 'NONE',  ( 0.4814626134252603107, -1.674667815061178455, 0.4945816651399402297 ) ) ;
#34469 = CARTESIAN_POINT ( 'NONE',  ( -0.03303708955568269295, 0.3731861634337363953, -0.3634708273687332070 ) ) ;
#34470 = AXIS2_PLACEMENT_3D ( 'NONE', #22363, #10403, #28520 ) ;
#34471 = VECTOR ( 'NONE', #9141, 39.37007874015747433 ) ;
#34472 = FACE_OUTER_BOUND ( 'NONE', #33839, .T. ) ;
#34473 = LOCAL_TIME ( 0, 53, 7.000000000000000000, #20981 ) ;
#34474 = CARTESIAN_POINT ( 'NONE',  ( 0.2343914929394679270, -1.231693708927193986, 0.5277184083482510113 ) ) ;
#34475 = DIRECTION ( 'NONE',  ( -6.162975822039154730E-33, 0.000000000000000000, -1.000000000000000000 ) ) ;
#34476 = FACE_OUTER_BOUND ( 'NONE', #25145, .T. ) ;
#34477 = VECTOR ( 'NONE', #34868, 39.37007874015748143 ) ;
#34478 = CARTESIAN_POINT ( 'NONE',  ( 0.4715326458378593655, -1.065703591122391103, 0.8369151567944118630 ) ) ;
#34479 = CARTESIAN_POINT ( 'NONE',  ( -0.04285561529641203349, 0.3459893009865078750, 0.3537429040513690448 ) ) ;
#34480 = CARTESIAN_POINT ( 'NONE',  ( 0.03249461378931156608, -1.132065962088204980, 0.6695808836488423843 ) ) ;
#34481 = DIRECTION ( 'NONE',  ( 1.000000000000000000, 1.446659165673942287E-15, -8.266623803851098360E-16 ) ) ;
#34482 = CARTESIAN_POINT ( 'NONE',  ( -0.2399999999999999079, -2.853330612949663170, -0.6088139570729240724 ) ) ;
#34483 = CARTESIAN_POINT ( 'NONE',  ( 0.1713655093773583105, -0.9087330125397632408, 0.6023929517496198205 ) ) ;
#34484 = CARTESIAN_POINT ( 'NONE',  ( 0.3727347521531706454, -1.154750239813580714, 0.4257713460756237245 ) ) ;
#34485 = CARTESIAN_POINT ( 'NONE',  ( -0.6247879186461532397, 0.2375666616292463063, 0.08499999999999977018 ) ) ;
#34486 = ORIENTED_EDGE ( 'NONE', *, *, #29393, .T. ) ;
#34487 = DIRECTION ( 'NONE',  ( -1.000000000000000000, -0.000000000000000000, -0.000000000000000000 ) ) ;
#34488 = FACE_OUTER_BOUND ( 'NONE', #21925, .T. ) ;
#34489 = VECTOR ( 'NONE', #9248, 39.37007874015748143 ) ;
#34490 = CARTESIAN_POINT ( 'NONE',  ( 0.6568730927750903170, -1.460570608776345036, 0.4224083929475443422 ) ) ;
#34491 = CARTESIAN_POINT ( 'NONE',  ( 0.02953079040095728247, 0.000000000000000000, 0.000000000000000000 ) ) ;
#34492 = CARTESIAN_POINT ( 'NONE',  ( 0.3388158023681371311, -1.760717924938912438, 0.5703872202102562294 ) ) ;
#34493 = CIRCLE ( 'NONE', #35789, 0.03000000000000003705 ) ;
#34494 = CIRCLE ( 'NONE', #27928, 0.1762268159172233339 ) ;
#34495 = ORIENTED_EDGE ( 'NONE', *, *, #25521, .F. ) ;
#34496 = CARTESIAN_POINT ( 'NONE',  ( 0.3868427017360319686, -1.755940305036085558, -0.5592542411036628414 ) ) ;
#34497 = CARTESIAN_POINT ( 'NONE',  ( 0.1514353721145317300, -1.395111566407175152, 0.4677691116936663618 ) ) ;
#34498 = APPROVAL_PERSON_ORGANIZATION ( #19806, #23269, #25588 ) ;
#34499 = CARTESIAN_POINT ( 'NONE',  ( 0.1876514731215554732, -0.8468096824363462449, 0.2227353535533353190 ) ) ;
#34500 = CARTESIAN_POINT ( 'NONE',  ( 0.03171861681798987531, 0.3665016810530090652, -0.3753647833258712541 ) ) ;
#34501 = CARTESIAN_POINT ( 'NONE',  ( 0.5117419007255246122, -1.313278830500390182, 0.6011698456470916385 ) ) ;
#34503 = ORIENTED_EDGE ( 'NONE', *, *, #5884, .F. ) ;
#34502 = CARTESIAN_POINT ( 'NONE',  ( 0.05999999999999990757, -0.2940959072101921867, -0.05922497245433272495 ) ) ;
#34504 = CARTESIAN_POINT ( 'NONE',  ( 0.4878597496520711285, -1.079924603896147195, 0.5970707234729024648 ) ) ;
#34505 = EDGE_LOOP ( 'NONE', ( #7031, #24106, #16255, #23726 ) ) ;
#34506 = DATE_AND_TIME ( #18890, #20778 ) ;
#34507 = CIRCLE ( 'NONE', #13518, 0.1400000000000010403 ) ;
#34508 = DIRECTION ( 'NONE',  ( -0.4999551463232372317, 0.8660512985181134660, 0.000000000000000000 ) ) ;
#34509 = VERTEX_POINT ( 'NONE', #39031 ) ;
#34510 = CARTESIAN_POINT ( 'NONE',  ( 0.04758055007403567266, -0.6291802298475768218, 0.4158285656181007761 ) ) ;
#34512 = CARTESIAN_POINT ( 'NONE',  ( 0.1852687023069083672, -0.7992365650813095801, 0.02179029107226419792 ) ) ;
#34511 = DIRECTION ( 'NONE',  ( 1.664003471950577032E-31, 3.330669073875470114E-16, 1.000000000000000000 ) ) ;
#34513 = CARTESIAN_POINT ( 'NONE',  ( 0.3568401510066848137, -1.627103573605686027, -0.3706434065951008661 ) ) ;
#34514 = ORIENTED_EDGE ( 'NONE', *, *, #13374, .F. ) ;
#34515 = ORIENTED_EDGE ( 'NONE', *, *, #9716, .T. ) ;
#34516 = ORIENTED_EDGE ( 'NONE', *, *, #30870, .T. ) ;
#34517 = CARTESIAN_POINT ( 'NONE',  ( 0.3443385366210869325, -1.072482504630695388, 0.6392052143392089603 ) ) ;
#34518 = CARTESIAN_POINT ( 'NONE',  ( 0.4889399104974117560, -1.382089549755538327, 0.8085469255259594146 ) ) ;
#34519 = ORIENTED_EDGE ( 'NONE', *, *, #16014, .F. ) ;
#34520 = CARTESIAN_POINT ( 'NONE',  ( 0.1873216024392761192, -0.6989317540256104744, 0.03190675745988370837 ) ) ;
#34521 = CARTESIAN_POINT ( 'NONE',  ( 0.5433433239293584682, -1.169038973927291503, 0.5856983068965047057 ) ) ;
#34522 = CARTESIAN_POINT ( 'NONE',  ( 0.6067096000040144155, -1.405345748401797712, -0.6250000000000000000 ) ) ;
#34523 = CARTESIAN_POINT ( 'NONE',  ( 0.4688459138424372341, -1.061988423737608045, -0.4248180574663140141 ) ) ;
#34524 = TOROIDAL_SURFACE ( 'NONE', #6263, 1.986674066779348768, 0.01499999999999999944 ) ;
#34525 = B_SPLINE_CURVE_WITH_KNOTS ( 'NONE', 3,
 ( #21005, #5553, #14006, #27397 ),
 .UNSPECIFIED., .F., .F.,
 ( 4, 4 ),
 ( 0.000000000000000000, 0.0003263726155882985011 ),
 .UNSPECIFIED. ) ;
#34526 = AXIS2_PLACEMENT_3D ( 'NONE', #13075, #35287, #25628 ) ;
#34527 = CARTESIAN_POINT ( 'NONE',  ( -0.3000000000000000999, -3.318147336744930342, -0.6877918253319055264 ) ) ;
#34528 = CARTESIAN_POINT ( 'NONE',  ( 0.000000000000000000, 0.000000000000000000, 0.000000000000000000 ) ) ;
#34529 = CARTESIAN_POINT ( 'NONE',  ( 0.2225889308918536924, -1.238345268919997855, 0.5682417262808776570 ) ) ;
#34530 = ADVANCED_FACE ( 'NONE', ( #38817 ), #4272, .F. ) ;
#34531 = CARTESIAN_POINT ( 'NONE',  ( -0.005948725901132238467, -2.039406408238342294, -0.6755655181501677431 ) ) ;
#34532 = CARTESIAN_POINT ( 'NONE',  ( 0.1145268569410018006, -1.410781586862627224, 0.6062388606988194928 ) ) ;
#34533 = DATE_TIME_ROLE ( 'classification_date' ) ;
#34534 = LOCAL_TIME ( 0, 53, 7.000000000000000000, #35500 ) ;
#34535 = APPLIED_PERSON_AND_ORGANIZATION_ASSIGNMENT ( #33554, #24322, ( #2357 ) ) ;
#34536 = CARTESIAN_POINT ( 'NONE',  ( 0.1897171943901793389, -0.9163440338727294465, 0.2193954077252403545 ) ) ;
#34537 = DIRECTION ( 'NONE',  ( 0.000000000000000000, -0.8438867430782091006, -0.5365213554527469286 ) ) ;
#34538 = CARTESIAN_POINT ( 'NONE',  ( 0.5523217627366585614, -1.163855889859017889, 0.5856983068965044836 ) ) ;
#34539 = AXIS2_PLACEMENT_3D ( 'NONE', #39429, #11665, #23820 ) ;
#34541 = EDGE_LOOP ( 'NONE', ( #12912, #17198, #17287 ) ) ;
#34540 = LINE ( 'NONE', #40294, #15971 ) ;
#34542 = CARTESIAN_POINT ( 'NONE',  ( 0.1799043607419438529, -1.488798643046104875, 0.7589116457392215409 ) ) ;
#34543 = CARTESIAN_POINT ( 'NONE',  ( 0.5831586614430237514, -1.507066788378804478, -0.4433506751720494021 ) ) ;
#34544 = CARTESIAN_POINT ( 'NONE',  ( 0.4311002502204824838, -1.610536115251105738, -0.3671355303406891313 ) ) ;
#34545 = CARTESIAN_POINT ( 'NONE',  ( 0.3459486122327841695, -1.629317532511044497, 0.4807459044743475629 ) ) ;
#34546 = ORIENTED_EDGE ( 'NONE', *, *, #32500, .F. ) ;
#34547 = EDGE_LOOP ( 'NONE', ( #7207, #3756 ) ) ;
#34548 = CARTESIAN_POINT ( 'NONE',  ( 0.02953079040095673430, -0.2329676531120485339, -0.4763574306556319637 ) ) ;
#34549 = ORIENTED_EDGE ( 'NONE', *, *, #36389, .F. ) ;
#34550 = CARTESIAN_POINT ( 'NONE',  ( -0.02000000000000000042, -2.253856486606507836, -0.7252438489935795207 ) ) ;
#34551 = CARTESIAN_POINT ( 'NONE',  ( -0.04582713223189510687, -0.4389429380065676400, -0.2108029774974920778 ) ) ;
#34552 = CARTESIAN_POINT ( 'NONE',  ( 0.5912128005600242320, -1.447495737070808142, 0.6721173034932466095 ) ) ;
#34554 = ORIENTED_EDGE ( 'NONE', *, *, #26622, .F. ) ;
#34553 = CARTESIAN_POINT ( 'NONE',  ( 0.6020307166002785149, -1.477835242481402078, 0.5986708909347367991 ) ) ;
#34555 = AXIS2_PLACEMENT_3D ( 'NONE', #36531, #30353, #26873 ) ;
#34556 = AXIS2_PLACEMENT_3D ( 'NONE', #28668, #6836, #19001 ) ;
#34557 = B_SPLINE_CURVE_WITH_KNOTS ( 'NONE', 3,
 ( #3560, #19200, #6235, #31531 ),
 .UNSPECIFIED., .F., .F.,
 ( 4, 4 ),
 ( 7.823333095578703919E-15, 0.001097874967820342733 ),
 .UNSPECIFIED. ) ;
#34558 = VERTEX_POINT ( 'NONE', #26496 ) ;
#34559 = CARTESIAN_POINT ( 'NONE',  ( 0.5994846556772400747, -1.482927862621986392, -0.6371164520993247704 ) ) ;
#34560 = ADVANCED_FACE ( 'NONE', ( #39242 ), #1231, .T. ) ;
#34561 = ORIENTED_EDGE ( 'NONE', *, *, #19006, .T. ) ;
#34562 = CARTESIAN_POINT ( 'NONE',  ( 0.1618130643425950421, -1.132953745604308393, 0.8857258589616595623 ) ) ;
#34564 = CARTESIAN_POINT ( 'NONE',  ( 0.08765592157946001939, -1.316965293376829216, 0.5674773004636822771 ) ) ;
#34563 = CARTESIAN_POINT ( 'NONE',  ( 0.3354003383065387589, -1.100282042489750811, 0.7404311049156548918 ) ) ;
#34565 = DIRECTION ( 'NONE',  ( 1.000000000000000000, -0.000000000000000000, -0.000000000000000000 ) ) ;
#34566 = ORGANIZATION ( 'NAUO-ORG7', 'UNSPECIFIED', 'UNSPECIFIED' ) ;
#34567 = CARTESIAN_POINT ( 'NONE',  ( 0.01215609957436605652, -0.4301083516152499620, 0.1115223648745343049 ) ) ;
#34568 = ADVANCED_FACE ( 'NONE', ( #27917 ), #4820, .T. ) ;
#34569 = EDGE_CURVE ( 'NONE', #27821, #10465, #8560, .T. ) ;
#34570 = CARTESIAN_POINT ( 'NONE',  ( -0.1210148435730243194, -0.5061394519557864680, 0.3122829191279359318 ) ) ;
#34571 = B_SPLINE_CURVE_WITH_KNOTS ( 'NONE', 3,
 ( #22913, #920, #35632, #7654 ),
 .UNSPECIFIED., .F., .F.,
 ( 4, 4 ),
 ( 1.734723475976806902E-18, 0.0007336933749192815985 ),
 .UNSPECIFIED. ) ;
#34573 = VERTEX_POINT ( 'NONE', #18436 ) ;
#34572 = EDGE_LOOP ( 'NONE', ( #9905, #21419, #16639, #7530 ) ) ;
#34574 = B_SPLINE_CURVE_WITH_KNOTS ( 'NONE', 3,
 ( #22277, #21867, #18973, #299 ),
 .UNSPECIFIED., .F., .F.,
 ( 4, 4 ),
 ( 0.004092191055103780277, 0.004352811462213712450 ),
 .UNSPECIFIED. ) ;
#34575 = EDGE_CURVE ( 'NONE', #15823, #27338, #17634, .T. ) ;
#34576 = CIRCLE ( 'NONE', #38502, 0.07499999999999977518 ) ;
#34577 = CARTESIAN_POINT ( 'NONE',  ( -0.04285534776242611033, -0.4878382857517556404, 0.08280911155782857969 ) ) ;
#34578 = CARTESIAN_POINT ( 'NONE',  ( -2.104403335822566002E-14, -2.101103024888176130, -0.2895076595251908080 ) ) ;
#34579 = CARTESIAN_POINT ( 'NONE',  ( 0.1261292094506277772, -0.8244062005499848134, 0.1457185332388709897 ) ) ;
#34580 = DIRECTION ( 'NONE',  ( 0.8660512985181139101, 0.4999551463232363990, 0.000000000000000000 ) ) ;
#34581 = CARTESIAN_POINT ( 'NONE',  ( 0.09862427037191998092, -0.8798430304322220064, 0.8669395311361297596 ) ) ;
#34582 = CARTESIAN_POINT ( 'NONE',  ( 0.07030502144589019509, -1.326531751660471548, 0.5682417262808779901 ) ) ;
#34583 = CARTESIAN_POINT ( 'NONE',  ( 0.2842326993136328195, -1.549395603922531617, -0.7208999815284821144 ) ) ;
#34584 = DIRECTION ( 'NONE',  ( 0.8660512985181133550, 0.4999551463232372872, 0.000000000000000000 ) ) ;
#34585 = EDGE_CURVE ( 'NONE', #2897, #36711, #19463, .T. ) ;
#34586 = CARTESIAN_POINT ( 'NONE',  ( 0.1999999999999787226, -2.097675824466502803, -0.4688691127277801463 ) ) ;
#34587 = DIRECTION ( 'NONE',  ( 6.801665408008644605E-18, -0.6431838620227177117, 0.7657117732107437957 ) ) ;
#34588 = CIRCLE ( 'NONE', #5683, 0.1749999999999999889 ) ;
#34589 = CARTESIAN_POINT ( 'NONE',  ( 0.6540709664215760277, -1.593060928864740156, 0.5182417262812423209 ) ) ;
#34590 = CARTESIAN_POINT ( 'NONE',  ( 0.2556072607908594918, -1.486118078215695082, 1.019147448260280475 ) ) ;
#34591 = CARTESIAN_POINT ( 'NONE',  ( 0.05224697855747006958, -1.083945988322971843, 0.7370724361663850699 ) ) ;
#34592 = PRODUCT_CONTEXT ( 'NONE', #18750, 'mechanical' ) ;
#34593 = LOCAL_TIME ( 0, 53, 7.000000000000000000, #2686 ) ;
#34594 = CARTESIAN_POINT ( 'NONE',  ( -0.04229974373173753938, 0.4430055847546672809, 0.1530238331097821258 ) ) ;
#34595 = CARTESIAN_POINT ( 'NONE',  ( 0.7012556518089668733, -1.538026872409016255, 0.5808264824219138145 ) ) ;
#34596 = CIRCLE ( 'NONE', #2392, 0.06173076923076910999 ) ;
#34597 = CARTESIAN_POINT ( 'NONE',  ( -0.1399999999999997358, 0.000000000000000000, 0.000000000000000000 ) ) ;
#34598 = CARTESIAN_POINT ( 'NONE',  ( 0.3674440818730608238, -1.689157367836090273, -0.4373319235121027604 ) ) ;
#34599 = ORIENTED_EDGE ( 'NONE', *, *, #875, .F. ) ;
#34600 = CARTESIAN_POINT ( 'NONE',  ( 0.4469283285619459201, -1.099869350908816878, -0.4033480720695140631 ) ) ;
#34601 = CARTESIAN_POINT ( 'NONE',  ( 0.2663611043439514936, -1.609278709772456795, 0.8236604638598111761 ) ) ;
#34602 = CARTESIAN_POINT ( 'NONE',  ( 0.5938776191701434781, -1.482008058293285746, 0.6415007704987426562 ) ) ;
#34604 = ORIENTED_EDGE ( 'NONE', *, *, #40550, .F. ) ;
#34603 = CARTESIAN_POINT ( 'NONE',  ( 0.5433433239293584682, -1.169038973927291503, 0.5856983068965047057 ) ) ;
#34605 = B_SPLINE_CURVE_WITH_KNOTS ( 'NONE', 3,
 ( #396, #10213, #25451, #35304, #37982, #22364, #34887, #6696, #26450, #29728, #26251, #16578, #16987, #1185, #32805, #1368, #10404, #29124, #4427, #13686, #38988, #29527, #38771, #13875 ),
 .UNSPECIFIED., .F., .F.,
 ( 4, 2, 2, 2, 2, 2, 2, 2, 2, 2, 2, 4 ),
 ( 0.01813101908972761245, 0.02053964073319797246, 0.02294826237666833246, 0.02535688402013869247, 0.02776550566360905248, 0.03258274895054977249, 0.03378705977228495250, 0.03499137059402013250, 0.03619568141575531250, 0.03679783682662289557, 0.03709891453205669404, 0.03739999223749048557 ),
 .UNSPECIFIED. ) ;
#34607 = ORIENTED_EDGE ( 'NONE', *, *, #20057, .F. ) ;
#34606 = ORIENTED_EDGE ( 'NONE', *, *, #975, .T. ) ;
#34608 = CARTESIAN_POINT ( 'NONE',  ( 0.3278576390227929127, -0.8618518445022319563, 0.6723808983945177564 ) ) ;
#34609 = EDGE_CURVE ( 'NONE', #9161, #18789, #2811, .T. ) ;
#34610 = DIRECTION ( 'NONE',  ( -1.000000000000000000, -2.341930812374887555E-31, 1.664003471950578127E-31 ) ) ;
#34611 = DIRECTION ( 'NONE',  ( -1.000000000000000000, -1.138269997360102279E-15, 1.138269997360102279E-15 ) ) ;
#34612 = APPROVAL_ROLE ( '' ) ;
#34613 = EDGE_CURVE ( 'NONE', #545, #10778, #25889, .T. ) ;
#34614 = DIRECTION ( 'NONE',  ( -1.000000000000000000, -0.000000000000000000, -0.000000000000000000 ) ) ;
#34615 = ORIENTED_EDGE ( 'NONE', *, *, #7887, .T. ) ;
#34616 = TOROIDAL_SURFACE ( 'NONE', #40514, 0.07749999999977548459, 0.01000000000000000021 ) ;
#34617 = EDGE_CURVE ( 'NONE', #30000, #2251, #38991, .T. ) ;
#34618 = CARTESIAN_POINT ( 'NONE',  ( 0.1816443464261394691, -0.8741777808320030374, 0.5909987484381754586 ) ) ;
#34619 = CARTESIAN_POINT ( 'NONE',  ( 0.5252056258530563015, -1.526865455870212163, 0.5731947314661878234 ) ) ;
#34620 = CARTESIAN_POINT ( 'NONE',  ( 0.3698249976192136135, -1.096058018356230734, -0.5155029497116575543 ) ) ;
#34621 = CARTESIAN_POINT ( 'NONE',  ( -0.05083665881509043943, -0.2375940621857665636, 0.4096919151850478835 ) ) ;
#34622 = VERTEX_POINT ( 'NONE', #11858 ) ;
#34623 = CARTESIAN_POINT ( 'NONE',  ( 0.4524429500423481909, -1.683290388497794776, 0.5885333811653102876 ) ) ;
#34624 = CARTESIAN_POINT ( 'NONE',  ( 0.6663429882773612700, -1.552917541305505189, 0.6639169729098425288 ) ) ;
#34625 = DIRECTION ( 'NONE',  ( 0.8660512985181134660, 0.4999551463232372317, 0.000000000000000000 ) ) ;
#34626 = CARTESIAN_POINT ( 'NONE',  ( 0.4119022438926009388, -1.177436575425700571, 0.8152005758745497488 ) ) ;
#34627 = ADVANCED_FACE ( 'NONE', ( #21350 ), #26534, .T. ) ;
#34628 = DIRECTION ( 'NONE',  ( -1.387778780781449423E-15, 6.590151126658376924E-16, -1.000000000000000000 ) ) ;
#34629 = EDGE_CURVE ( 'NONE', #14891, #37899, #2610, .T. ) ;
#34630 = CARTESIAN_POINT ( 'NONE',  ( 0.000000000000000000, 0.000000000000000000, 0.000000000000000000 ) ) ;
#34631 = EDGE_CURVE ( 'NONE', #40066, #13061, #37770, .T. ) ;
#34632 = FACE_OUTER_BOUND ( 'NONE', #16005, .T. ) ;
#34633 = EDGE_CURVE ( 'NONE', #39255, #19455, #12597, .T. ) ;
#34634 = DIRECTION ( 'NONE',  ( -1.000000000000000000, -2.280301054154495132E-31, 1.664003471950577689E-31 ) ) ;
#34635 = CARTESIAN_POINT ( 'NONE',  ( 0.0003547581337898165674, -0.9504652791025145486, 0.2394745140284491591 ) ) ;
#34636 = CARTESIAN_POINT ( 'NONE',  ( 0.2577558225373174916, -0.8624250852862554995, 0.5195666343558283939 ) ) ;
#34637 = PERSON_AND_ORGANIZATION ( #28500, #32463 ) ;
#34638 = CARTESIAN_POINT ( 'NONE',  ( -2.070754768975505034, -0.09959325338431362917, 0.09813923389047245205 ) ) ;
#34639 = CARTESIAN_POINT ( 'NONE',  ( 0.5375396755134189686, -1.518737640874254335, 0.5483303752197447034 ) ) ;
#34640 = CARTESIAN_POINT ( 'NONE',  ( -0.04947837552028416103, 0.03507397079375183108, 0.4759739487165450256 ) ) ;
#34641 = ORIENTED_EDGE ( 'NONE', *, *, #23528, .T. ) ;
#34642 = CARTESIAN_POINT ( 'NONE',  ( 0.2075534016687414773, -1.285863081042195377, -0.3981962265531751588 ) ) ;
#34643 = B_SPLINE_CURVE_WITH_KNOTS ( 'NONE', 3,
 ( #39897, #2471, #20581, #2661, #33110, #14380, #15005, #2052, #17489, #39687, #20984, #18095, #18299, #4923, #11309, #40082, #33501, #11911 ),
 .UNSPECIFIED., .F., .F.,
 ( 4, 2, 2, 2, 2, 2, 2, 2, 4 ),
 ( 0.0003425652276237173711, 0.001007165397454238978, 0.001671765567284760586, 0.002336365737115281976, 0.003000965906945803584, 0.003665566076776325191, 0.004330166246606846799, 0.004994766416437368406, 0.005659366586267890013 ),
 .UNSPECIFIED. ) ;
#34644 = CARTESIAN_POINT ( 'NONE',  ( 0.1873984653709714066, -0.8522402958051090716, 0.2163211054440509484 ) ) ;
#34645 = EDGE_LOOP ( 'NONE', ( #3437, #9251, #17295, #31022, #36533, #4992, #19631, #2635, #15274, #3845, #21616, #28838, #38685, #778, #37590, #505, #18274 ) ) ;
#34646 = CARTESIAN_POINT ( 'NONE',  ( 0.2318589737339854795, -1.232498520698479982, 0.5197417262808780025 ) ) ;
#34647 = CARTESIAN_POINT ( 'NONE',  ( 0.07600224412002334895, -1.084198183792790315, 0.7459357625971153594 ) ) ;
#34649 = VERTEX_POINT ( 'NONE', #18648 ) ;
#34648 = ORIENTED_EDGE ( 'NONE', *, *, #10168, .F. ) ;
#34650 = CARTESIAN_POINT ( 'NONE',  ( -2.112273405726188513E-14, -2.097675824466503691, -0.6968637352380161465 ) ) ;
#34651 = DIRECTION ( 'NONE',  ( 1.000000000000000000, 1.544378112879830442E-12, 7.552944938426298648E-13 ) ) ;
#34652 = CARTESIAN_POINT ( 'NONE',  ( 0.1995529058109177523, -2.050896138459941564, -0.3054326997595748217 ) ) ;
#34653 = EDGE_CURVE ( 'NONE', #38249, #27529, #30457, .T. ) ;
#34655 = DIRECTION ( 'NONE',  ( -7.771561172376107616E-16, 7.170354002788761615E-17, -1.000000000000000000 ) ) ;
#34654 = CARTESIAN_POINT ( 'NONE',  ( -0.01548846960707490547, 0.5198120922912035091, 0.07362328916749301400 ) ) ;
#34656 = CARTESIAN_POINT ( 'NONE',  ( -2.112273405726188513E-14, -2.097675824466503691, -0.7286991843995640483 ) ) ;
#34657 = ORIENTED_EDGE ( 'NONE', *, *, #11247, .T. ) ;
#34658 = CARTESIAN_POINT ( 'NONE',  ( 0.3324871086615504012, -1.659137217475707304, -0.6399689536651966826 ) ) ;
#34659 = ADVANCED_FACE ( 'NONE', ( #28512 ), #774, .F. ) ;
#34660 = CARTESIAN_POINT ( 'NONE',  ( 0.2195632003157210466, -0.8548457781082356988, 0.6847411545281603118 ) ) ;
#34661 = ORIENTED_EDGE ( 'NONE', *, *, #24403, .F. ) ;
#34662 = ORIENTED_EDGE ( 'NONE', *, *, #19556, .F. ) ;
#34663 = CARTESIAN_POINT ( 'NONE',  ( 0.03650577977170427202, 0.08362514765351862500, 0.5048437183011799112 ) ) ;
#34664 = CARTESIAN_POINT ( 'NONE',  ( 0.08156795407636466266, -0.6096982493729176111, 0.3618699794873930786 ) ) ;
#34666 = DIRECTION ( 'NONE',  ( -1.000000000000000000, -2.341930812374887555E-31, 1.664003471950578127E-31 ) ) ;
#34665 = CARTESIAN_POINT ( 'NONE',  ( 0.002316381905007189150, -0.5232263146340704330, 0.1844568262363025790 ) ) ;
#34667 = LINE ( 'NONE', #40630, #19832 ) ;
#34668 = CARTESIAN_POINT ( 'NONE',  ( 0.2707375556126198068, -0.9607971206205383474, 0.5189254608558738768 ) ) ;
#34669 = DIRECTION ( 'NONE',  ( 0.000000000000000000, 0.000000000000000000, -1.000000000000000000 ) ) ;
#34670 = CARTESIAN_POINT ( 'NONE',  ( 0.1255523023994105092, -0.5499328071996130163, 0.1457185332388692689 ) ) ;
#34671 = CARTESIAN_POINT ( 'NONE',  ( -0.03650581953630599452, 0.2290855126858387936, 0.4575806651622378318 ) ) ;
#34672 = CARTESIAN_POINT ( 'NONE',  ( -0.2399999999999999079, -4.074947978347777777, -0.4909924454747331413 ) ) ;
#34673 = CARTESIAN_POINT ( 'NONE',  ( -0.02238765564325446641, -0.4611651364438438261, -0.2234192167502431769 ) ) ;
#34674 = CARTESIAN_POINT ( 'NONE',  ( 0.06926373081126928344, -0.5403174658036256073, 0.1556459889883224090 ) ) ;
#34675 = DIRECTION ( 'NONE',  ( 0.4999999999999984457, 0.4254978411528151372, 0.7542887956043727860 ) ) ;
#34676 = EDGE_CURVE ( 'NONE', #12314, #19872, #17986, .T. ) ;
#34677 = CONICAL_SURFACE ( 'NONE', #20220, 0.03999999999999933470, 1.047197551196598742 ) ;
#34678 = CARTESIAN_POINT ( 'NONE',  ( 0.3050116026255210722, -0.8112037691066587008, 0.6500339927034136656 ) ) ;
#34679 = CARTESIAN_POINT ( 'NONE',  ( -0.05187277790672333022, 0.2910352029727566459, 0.3700865090056973394 ) ) ;
#34680 = CARTESIAN_POINT ( 'NONE',  ( 0.05318916154647986699, -1.262669248688604862, 0.6621301725941526328 ) ) ;
#34681 = CARTESIAN_POINT ( 'NONE',  ( 0.6382086589690751932, -1.585474446196608600, -0.4355293602703178557 ) ) ;
#34682 = CARTESIAN_POINT ( 'NONE',  ( -0.3000000000000000999, -2.416006048095809877, -1.059240699271965402 ) ) ;
#34683 = CARTESIAN_POINT ( 'NONE',  ( 0.1203098315036280619, -0.8529650373737380775, 0.4308920117485077195 ) ) ;
#34684 = DIRECTION ( 'NONE',  ( 0.000000000000000000, 2.731847993664262824E-15, -1.000000000000000000 ) ) ;
#34685 = CARTESIAN_POINT ( 'NONE',  ( -2.070903537920736781, -2.678131749591557309, 0.6057417262810178560 ) ) ;
#34686 = EDGE_LOOP ( 'NONE', ( #29364, #24772, #17015, #13683 ) ) ;
#34687 = CARTESIAN_POINT ( 'NONE',  ( 0.3616412802242882085, -1.759290408629955671, -0.5212859374497357257 ) ) ;
#34688 = CARTESIAN_POINT ( 'NONE',  ( 0.5951553339360416972, -1.455642694606908760, 0.6304964123869174486 ) ) ;
#34689 = CARTESIAN_POINT ( 'NONE',  ( 0.3660631757498663541, -2.015934369490486322, -0.5042582106743112025 ) ) ;
#34690 = DIRECTION ( 'NONE',  ( -7.771561172376107616E-16, 7.170354002788761615E-17, -1.000000000000000000 ) ) ;
#34691 = CARTESIAN_POINT ( 'NONE',  ( -0.2399999999999999079, -2.139295658456680904, -0.2024034539465678073 ) ) ;
#34692 = VERTEX_POINT ( 'NONE', #15571 ) ;
#34693 = CARTESIAN_POINT ( 'NONE',  ( 0.3794148853686062361, -1.617193962983704880, -0.6670239321470404770 ) ) ;
#34694 = DIRECTION ( 'NONE',  ( -0.4999551463232372317, 0.8660512985181135770, -0.000000000000000000 ) ) ;
#34695 = CARTESIAN_POINT ( 'NONE',  ( 0.4869779214331270700, -1.661191848117253178, 0.5366761509299960986 ) ) ;
#34696 = CARTESIAN_POINT ( 'NONE',  ( 0.04157143636675521281, 0.2624507507128696071, -0.3902120892151714759 ) ) ;
#34697 = CARTESIAN_POINT ( 'NONE',  ( 0.4097880553864961528, -1.161594837369823940, 0.7403270510053888698 ) ) ;
#34698 = ADVANCED_FACE ( 'NONE', ( #25020 ), #19266, .F. ) ;
#34699 = EDGE_CURVE ( 'NONE', #27226, #6266, #9992, .T. ) ;
#34701 = CARTESIAN_POINT ( 'NONE',  ( 0.3768783096114195486, -1.720370743462858343, 0.4222122349756301518 ) ) ;
#34700 = DIRECTION ( 'NONE',  ( -1.387778780781449620E-15, 6.528313220153589231E-16, -1.000000000000000000 ) ) ;
#34702 = CARTESIAN_POINT ( 'NONE',  ( 0.4885592119991905014, -1.080308374838712782, 0.5952236481819053182 ) ) ;
#34703 = ORIENTED_EDGE ( 'NONE', *, *, #30794, .T. ) ;
#34704 = PERSON_AND_ORGANIZATION ( #28500, #32463 ) ;
#34705 = CIRCLE ( 'NONE', #29458, 0.01500000000000001679 ) ;
#34706 = CARTESIAN_POINT ( 'NONE',  ( 0.004754326254995749901, -0.8878146167104555841, 0.4619373158225143494 ) ) ;
#34707 = ORIENTED_EDGE ( 'NONE', *, *, #29288, .F. ) ;
#34708 = CARTESIAN_POINT ( 'NONE',  ( 0.3811835917169881793, -1.578736998356156773, 0.7419389678365337915 ) ) ;
#34710 = CARTESIAN_POINT ( 'NONE',  ( 0.1856512491390554243, -0.7629151448678782588, -0.003031259884144057136 ) ) ;
#34709 = DIRECTION ( 'NONE',  ( 7.771561172376107616E-16, -7.170354002788761615E-17, 1.000000000000000000 ) ) ;
#34711 = PLANE ( 'NONE',  #18479 ) ;
#34712 = VERTEX_POINT ( 'NONE', #9591 ) ;
#34713 = ORIENTED_EDGE ( 'NONE', *, *, #6638, .F. ) ;
#34714 = CARTESIAN_POINT ( 'NONE',  ( 0.5959315179729194334, -1.587052097778459014, 0.4282417262808783653 ) ) ;
#34715 = CARTESIAN_POINT ( 'NONE',  ( 0.4386138752512657724, -1.295316779970371313, 0.8303206930615300019 ) ) ;
#34716 = EDGE_LOOP ( 'NONE', ( #28138, #11336, #3941, #7359 ) ) ;
#34717 = CARTESIAN_POINT ( 'NONE',  ( 0.01814701835283376308, -0.9892295991911050912, 0.4798887309902147846 ) ) ;
#34718 = FACE_OUTER_BOUND ( 'NONE', #13315, .T. ) ;
#34719 = DIRECTION ( 'NONE',  ( 0.9378410757839547029, 0.2807814858886594211, 0.2039996905746454536 ) ) ;
#34720 = CARTESIAN_POINT ( 'NONE',  ( 0.1852939438208618395, -0.8373517857265262432, 0.1567296349695768420 ) ) ;
#34721 = DIRECTION ( 'NONE',  ( 1.000000000000000000, 1.131052719138050089E-31, -7.771561172376107616E-16 ) ) ;
#34722 = CARTESIAN_POINT ( 'NONE',  ( 0.3423116886662437297, -1.747674139269914884, 0.5964707725471621869 ) ) ;
#34723 = B_SPLINE_CURVE_WITH_KNOTS ( 'NONE', 3,
 ( #13165, #35585, #25732, #16881, #29422, #1269, #13773, #26336, #23265, #29827, #8410, #27151, #39892, #39472, #33309, #39282, #24270, #24468 ),
 .UNSPECIFIED., .F., .F.,
 ( 4, 2, 2, 2, 2, 2, 2, 2, 4 ),
 ( 0.000000000000000000, 0.0007746617437634276387, 0.001549323487526855277, 0.002323985231290282699, 0.003098646975053710555, 0.003873308718817138410, 0.004647970462580565398, 0.005422632206343993254, 0.006197293950107421109 ),
 .UNSPECIFIED. ) ;
#34724 = CARTESIAN_POINT ( 'NONE',  ( 0.08638421507254147313, -0.7700017860723418206, 0.02001464231056792470 ) ) ;
#34725 = LINE ( 'NONE', #40500, #27135 ) ;
#34726 = DIRECTION ( 'NONE',  ( -0.9624590225244425978, 0.000000000000000000, 0.2714270251122657407 ) ) ;
#34727 = CARTESIAN_POINT ( 'NONE',  ( 0.08428283282631070239, -1.315430133339995145, 0.5840562972504370620 ) ) ;
#34728 = CARTESIAN_POINT ( 'NONE',  ( 0.6179353394495009644, -1.299228382567916285, 0.5682417262808779901 ) ) ;
#34729 = PLANE ( 'NONE',  #31037 ) ;
#34730 = CALENDAR_DATE ( 2026, 13, 10 ) ;
#34731 = EDGE_CURVE ( 'NONE', #11734, #29150, #16019, .T. ) ;
#34732 = CARTESIAN_POINT ( 'NONE',  ( 0.3384799338905536970, -0.9979650346196410338, 0.5984318192120324786 ) ) ;
#34733 = CARTESIAN_POINT ( 'NONE',  ( 0.3130168538663060662, -1.175229136912986361, 0.5028472835892379145 ) ) ;
#34734 = DIRECTION ( 'NONE',  ( 1.000000000000000000, 3.414809992080303089E-15, -1.138269997360101095E-15 ) ) ;
#34735 = CARTESIAN_POINT ( 'NONE',  ( -0.1499999999999996336, 0.000000000000000000, 0.000000000000000000 ) ) ;
#34736 = CARTESIAN_POINT ( 'NONE',  ( -0.002083146443013342720, -0.8967360763018593639, 0.1136267619940960899 ) ) ;
#34737 = CARTESIAN_POINT ( 'NONE',  ( 0.0004250980212677150211, -0.4402291855641986551, 0.1128034438869898043 ) ) ;
#34738 = CARTESIAN_POINT ( 'NONE',  ( 0.1760929562092026501, -1.869776474524332821, -0.6851114302485398211 ) ) ;
#34739 = CARTESIAN_POINT ( 'NONE',  ( 0.3319227099733979003, -1.175833534577056527, 0.4282569450358217344 ) ) ;
#34740 = ORIENTED_EDGE ( 'NONE', *, *, #1297, .F. ) ;
#34741 = ORIENTED_EDGE ( 'NONE', *, *, #26862, .F. ) ;
#34742 = CARTESIAN_POINT ( 'NONE',  ( -0.2399999999999999079, -1.804235510932644004, -0.1501860188971498311 ) ) ;
#34743 = ORIENTED_EDGE ( 'NONE', *, *, #35578, .T. ) ;
#34744 = CARTESIAN_POINT ( 'NONE',  ( 0.7053185306253882958, -1.513916414415744649, 0.5667975048583363540 ) ) ;
#34745 = CARTESIAN_POINT ( 'NONE',  ( -0.05634307799789434884, -0.4332460723641310962, -0.1515798417490749894 ) ) ;
#34746 = CARTESIAN_POINT ( 'NONE',  ( 0.5953576370465231138, -1.455492272848171398, 0.6457864647264339730 ) ) ;
#34748 = ORIENTED_EDGE ( 'NONE', *, *, #32417, .F. ) ;
#34747 = CARTESIAN_POINT ( 'NONE',  ( 0.5734482455647949006, -1.622651489275899195, 0.4800729107877242385 ) ) ;
#34749 = ORIENTED_EDGE ( 'NONE', *, *, #38438, .F. ) ;
#34750 = B_SPLINE_CURVE_WITH_KNOTS ( 'NONE', 3,
 ( #10970, #7846, #23527, #33551, #12172, #30886 ),
 .UNSPECIFIED., .F., .F.,
 ( 4, 2, 4 ),
 ( 0.002802047142276810777, 0.003388785079928765924, 0.003975523017580721505 ),
 .UNSPECIFIED. ) ;
#34751 = CARTESIAN_POINT ( 'NONE',  ( 0.1852724517579373009, -0.8388905295248703098, 0.1482875376949696067 ) ) ;
#34752 = ORIENTED_EDGE ( 'NONE', *, *, #24619, .F. ) ;
#34753 = CARTESIAN_POINT ( 'NONE',  ( 0.02183045352075156653, -0.6280315654919215174, 0.4241349530551878355 ) ) ;
#34755 = CARTESIAN_POINT ( 'NONE',  ( -0.02235124290212954848, -0.4612278572487644168, 0.2234747101372511757 ) ) ;
#34754 = CARTESIAN_POINT ( 'NONE',  ( 0.4286824899518620891, -1.220626395943066766, 0.6356727319996533510 ) ) ;
#34756 = CARTESIAN_POINT ( 'NONE',  ( 0.3895888470569853768, -1.758301358926936730, -0.4737257729874836398 ) ) ;
#34757 = LINE ( 'NONE', #28190, #20704 ) ;
#34758 = CARTESIAN_POINT ( 'NONE',  ( 0.000000000000000000, 0.000000000000000000, 0.000000000000000000 ) ) ;
#34760 = ORIENTED_EDGE ( 'NONE', *, *, #9195, .T. ) ;
#34759 = VERTEX_POINT ( 'NONE', #3620 ) ;
#34761 = CARTESIAN_POINT ( 'NONE',  ( 0.7066109249242027435, -1.499057094600571238, 0.5182417262806440217 ) ) ;
#34762 = CARTESIAN_POINT ( 'NONE',  ( 0.2703269693566499043, -0.8913611900814359945, 0.5391764932455734849 ) ) ;
#34763 = CARTESIAN_POINT ( 'NONE',  ( -0.01548846960721245516, -0.07651041855108924039, -0.5222379212565266826 ) ) ;
#34764 = CARTESIAN_POINT ( 'NONE',  ( 0.6044909876012586336, -1.470555607199449666, 0.6611702863572196387 ) ) ;
#34765 = CARTESIAN_POINT ( 'NONE',  ( -0.3000000000000000999, -2.377368549242099949, -0.4802393080720198104 ) ) ;
#34766 = CARTESIAN_POINT ( 'NONE',  ( -0.2399999999999999079, -4.289222312108804225, -0.5708809693675255259 ) ) ;
#34767 = CARTESIAN_POINT ( 'NONE',  ( 0.3248332791687661425, -1.755151979504451676, 0.6785705204500919185 ) ) ;
#34768 =( REPRESENTATION_RELATIONSHIP ('NONE','NONE', #27514, #35919 ) REPRESENTATION_RELATIONSHIP_WITH_TRANSFORMATION ( #37476 )SHAPE_REPRESENTATION_RELATIONSHIP( ) );
#34769 = CARTESIAN_POINT ( 'NONE',  ( -0.05464101615137796630, -1.706654027108509997, -0.06438491259384494791 ) ) ;
#34770 = SPHERICAL_SURFACE ( 'NONE', #25900, 0.01499999999999999944 ) ;
#34771 = LINE ( 'NONE', #27804, #7404 ) ;
#34772 = DIRECTION ( 'NONE',  ( 1.000000000000000000, 0.000000000000000000, 0.000000000000000000 ) ) ;
#34773 = CARTESIAN_POINT ( 'NONE',  ( 0.000000000000000000, 0.000000000000000000, 0.000000000000000000 ) ) ;
#34774 = CARTESIAN_POINT ( 'NONE',  ( 0.04285427992854566603, -0.3459934409501838615, 0.3537438177964201125 ) ) ;
#34775 = EDGE_CURVE ( 'NONE', #20093, #24651, #9167, .T. ) ;
#34776 = CARTESIAN_POINT ( 'NONE',  ( 0.3137727395043992673, -1.722325404801505089, 0.8203598276066251804 ) ) ;
#34777 = CARTESIAN_POINT ( 'NONE',  ( 0.1052213198848533787, -1.408629276248457574, 0.5918252877697837144 ) ) ;
#34778 = EDGE_CURVE ( 'NONE', #2236, #12860, #4164, .T. ) ;
#34779 = SECURITY_CLASSIFICATION_LEVEL ( 'unclassified' ) ;
#34780 = EDGE_CURVE ( 'NONE', #8681, #31055, #13869, .T. ) ;
#34781 = CARTESIAN_POINT ( 'NONE',  ( 0.3351195522891313172, -1.762354232558481337, 0.5631496603913015431 ) ) ;
#34782 = DIRECTION ( 'NONE',  ( 0.7649703263416960386, 0.000000000000000000, 0.6440655244745516761 ) ) ;
#34783 = EDGE_CURVE ( 'NONE', #22334, #27427, #17384, .T. ) ;
#34784 = ORIENTED_EDGE ( 'NONE', *, *, #19556, .T. ) ;
#34785 = CARTESIAN_POINT ( 'NONE',  ( 0.1978587402095143555, -0.5849795632144964008, 0.3178455878192523731 ) ) ;
#34786 = ORIENTED_EDGE ( 'NONE', *, *, #25229, .F. ) ;
#34787 = DIRECTION ( 'NONE',  ( 0.9998941247116546194, -0.01455087607601020412, 0.0001066420868422379362 ) ) ;
#34788 = CARTESIAN_POINT ( 'NONE',  ( 0.2463166633156871344, -1.532156299544739309, 0.8923198964620434603 ) ) ;
#34789 = CARTESIAN_POINT ( 'NONE',  ( 0.1972707534773566473, -0.7764867367545040810, 0.5873998428394819893 ) ) ;
#34790 = B_SPLINE_CURVE_WITH_KNOTS ( 'NONE', 3,
 ( #8191, #33288, #17654, #14982, #36981, #18273, #9564, #14562, #22331, #27129, #33480, #34658 ),
 .UNSPECIFIED., .F., .F.,
 ( 4, 2, 2, 2, 2, 4 ),
 ( 5.485677294651095664E-18, 0.0005133272912129524610, 0.001026654582425899284, 0.002053309164851789027, 0.003079963747277678771, 0.004106618329703567646 ),
 .UNSPECIFIED. ) ;
#34792 = ORIENTED_EDGE ( 'NONE', *, *, #3963, .T. ) ;
#34791 = CARTESIAN_POINT ( 'NONE',  ( 0.4862737308021083393, -1.680336247396838401, -0.4180171117579152273 ) ) ;
#34794 = VERTEX_POINT ( 'NONE', #35478 ) ;
#34793 = ORIENTED_EDGE ( 'NONE', *, *, #21604, .T. ) ;
#34795 = CARTESIAN_POINT ( 'NONE',  ( 0.5399038930177495477, -1.667580954481910904, -0.5371941175943450997 ) ) ;
#34796 = VERTEX_POINT ( 'NONE', #7088 ) ;
#34797 = ADVANCED_FACE ( 'NONE', ( #19658 ), #16937, .F. ) ;
#34798 = APPLIED_PERSON_AND_ORGANIZATION_ASSIGNMENT ( #4269, #10043, ( #33833 ) ) ;
#34799 = CARTESIAN_POINT ( 'NONE',  ( 0.6226517055508813403, -1.619812196680018967, -0.5481868501644782121 ) ) ;
#34800 = APPROVAL_STATUS ( 'not_yet_approved' ) ;
#34801 = DIRECTION ( 'NONE',  ( -1.000000000000000000, -0.000000000000000000, -0.000000000000000000 ) ) ;
#34802 = ORIENTED_EDGE ( 'NONE', *, *, #12228, .T. ) ;
#34803 = CARTESIAN_POINT ( 'NONE',  ( 0.2123995819314469513, -0.9001393775761254989, 0.6432088496448890025 ) ) ;
#34804 = FACE_OUTER_BOUND ( 'NONE', #11413, .T. ) ;
#34805 = CARTESIAN_POINT ( 'NONE',  ( 0.1054506471514282812, -0.5698990576301153910, 0.2500573047465119991 ) ) ;
#34806 = CARTESIAN_POINT ( 'NONE',  ( 0.6111238512687238167, -1.556616907971307473, -0.6228061396314235054 ) ) ;
#34807 = CARTESIAN_POINT ( 'NONE',  ( -0.1646294012188481148, 0.5114631038222671178, 0.1176773486970680294 ) ) ;
#34808 = ORIENTED_EDGE ( 'NONE', *, *, #1224, .F. ) ;
#34809 = VECTOR ( 'NONE', #30663, 39.37007874015748854 ) ;
#34810 = CARTESIAN_POINT ( 'NONE',  ( 0.4081734154113714208, -1.720235488236536714, 0.6107698181414052963 ) ) ;
#34811 = CARTESIAN_POINT ( 'NONE',  ( 0.6433413964517614714, -1.490184457409822416, 0.7922965759278289832 ) ) ;
#34812 = ORIENTED_EDGE ( 'NONE', *, *, #30157, .T. ) ;
#34813 = CARTESIAN_POINT ( 'NONE',  ( 0.4296077269088026673, -1.643823256665882360, -0.6213498245139347231 ) ) ;
#34814 = AXIS2_PLACEMENT_3D ( 'NONE', #27164, #17880, #8424 ) ;
#34815 = CARTESIAN_POINT ( 'NONE',  ( 0.6095958906658129894, -1.477207775979266113, 0.6170772022735478979 ) ) ;
#34816 = CARTESIAN_POINT ( 'NONE',  ( -0.1684323895664525950, 0.5231977504174881721, 0.3032895567580808360 ) ) ;
#34817 = CARTESIAN_POINT ( 'NONE',  ( -0.1045574869087419617, -0.4741643323009803734, 0.09813923389047396473 ) ) ;
#34818 = CARTESIAN_POINT ( 'NONE',  ( 0.02231181081520564047, -0.5045902076536123992, -0.09028112709016493376 ) ) ;
#34819 = CARTESIAN_POINT ( 'NONE',  ( 0.006497850577614296130, -0.9898846675935381034, 0.4770811589384994500 ) ) ;
#34820 = CARTESIAN_POINT ( 'NONE',  ( 0.5137183020217809259, -1.118314259765692764, 0.5770968910244165251 ) ) ;
#34821 = EDGE_CURVE ( 'NONE', #12702, #7023, #835, .T. ) ;
#34822 = APPLICATION_PROTOCOL_DEFINITION ( 'international standard', 'automotive_design', 2000, #23728 ) ;
#34823 =( BOUNDED_SURFACE ( )  B_SPLINE_SURFACE ( 3, 2, ( 
 ( #40518, #33950, #5751 ),
 ( #40307, #27768, #34338 ),
 ( #12137, #5543, #2280 ),
 ( #11728, #14819, #5322 ),
 ( #27382, #15213, #39908 ),
 ( #2672, #42, #36807 ),
 ( #8841, #24699, #33730 ),
 ( #12340, #37231, #9049 ),
 ( #6153, #21191, #21611 ),
 ( #15630, #24898, #2479 ) ),
 .UNSPECIFIED., .F., .F., .F. ) 
 B_SPLINE_SURFACE_WITH_KNOTS ( ( 4, 2, 2, 2, 4 ),
 ( 3, 3 ),
 ( 0.001500576079630530895, 0.001976458225352494859, 0.002452340371074459256, 0.002928222516796423220, 0.003404104662518387184 ),
 ( 0.000000000000000000, 1.000000000000000000 ),
 .UNSPECIFIED. ) 
 GEOMETRIC_REPRESENTATION_ITEM ( )  RATIONAL_B_SPLINE_SURFACE ( (
 ( 1.000000000000000000, 0.9128709291752995503, 1.000000000000000000),
 ( 1.000000000000000000, 0.9128711300566455522, 1.000000000000000000),
 ( 1.000000000000000000, 0.9128295461284150480, 1.000000000000000000),
 ( 1.000000000000000000, 0.9126769222980595231, 1.000000000000000000),
 ( 1.000000000000000000, 0.9125696619638158369, 1.000000000000000000),
 ( 1.000000000000000000, 0.9123247991092858777, 1.000000000000000000),
 ( 1.000000000000000000, 0.9121939566647505604, 1.000000000000000000),
 ( 1.000000000000000000, 0.9119567588128756341, 1.000000000000000000),
 ( 1.000000000000000000, 0.9118559517120560232, 1.000000000000000000),
 ( 1.000000000000000000, 0.9117915798251829962, 1.000000000000000000) ) ) 
 REPRESENTATION_ITEM ( '' )  SURFACE ( )  );
#34824 = DIRECTION ( 'NONE',  ( 0.8660512985181134660, 0.4999551463232372317, 0.000000000000000000 ) ) ;
#34825 = EDGE_CURVE ( 'NONE', #7054, #17084, #16535, .T. ) ;
#34826 = CARTESIAN_POINT ( 'NONE',  ( 0.4665061541563142455, -1.559087575406794546, 0.5615006216634282898 ) ) ;
#34827 = ADVANCED_FACE ( 'NONE', ( #35696 ), #20471, .F. ) ;
#34828 = CARTESIAN_POINT ( 'NONE',  ( -0.05279185365593443147, -0.03990109708163243341, 0.4667311364329202461 ) ) ;
#34829 = VERTEX_POINT ( 'NONE', #30934 ) ;
#34830 = CARTESIAN_POINT ( 'NONE',  ( 0.4369325048625125052, -1.577024436001213337, 0.5877075299981957546 ) ) ;
#34831 = CARTESIAN_POINT ( 'NONE',  ( 0.01548846960707524721, 0.000000000000000000, 0.000000000000000000 ) ) ;
#34832 = AXIS2_PLACEMENT_3D ( 'NONE', #34742, #6548, #6755 ) ;
#34833 = CARTESIAN_POINT ( 'NONE',  ( 0.08895852713552732105, -0.5944957032902286054, 0.06479970134998659648 ) ) ;
#34834 = ORIENTED_EDGE ( 'NONE', *, *, #22319, .T. ) ;
#34835 = CARTESIAN_POINT ( 'NONE',  ( 0.3380199588881184769, -1.750814078658277095, 0.4537226720579596861 ) ) ;
#34836 = CARTESIAN_POINT ( 'NONE',  ( 0.1597909806901142149, -1.352425750947476413, 0.6653032890432879487 ) ) ;
#34838 = ORIENTED_EDGE ( 'NONE', *, *, #37063, .F. ) ;
#34837 = ORIENTED_EDGE ( 'NONE', *, *, #19290, .T. ) ;
#34839 = CARTESIAN_POINT ( 'NONE',  ( -0.05464101615137784834, -2.230494317742474308, -0.6487310457122437146 ) ) ;
#34840 = AXIS2_PLACEMENT_3D ( 'NONE', #8230, #33326, #33515 ) ;
#34841 = VERTEX_POINT ( 'NONE', #36290 ) ;
#34842 = CARTESIAN_POINT ( 'NONE',  ( 0.1834964085430285941, -1.226715333008844055, -0.5155029497116575543 ) ) ;
#34843 = EDGE_CURVE ( 'NONE', #11737, #34649, #25862, .T. ) ;
#34844 = EDGE_CURVE ( 'NONE', #11318, #28442, #10756, .T. ) ;
#34845 = CARTESIAN_POINT ( 'NONE',  ( 0.4315909263077353786, -1.207668101024179430, 0.5182417262812423209 ) ) ;
#34847 = FACE_OUTER_BOUND ( 'NONE', #10330, .T. ) ;
#34846 = CARTESIAN_POINT ( 'NONE',  ( 0.05281452789367269141, 0.4315450824722586454, 0.1820506770216148984 ) ) ;
#34848 = CARTESIAN_POINT ( 'NONE',  ( 0.02953079040094746394, -0.2329676531120573046, -0.4763574306556540017 ) ) ;
#34849 = VERTEX_POINT ( 'NONE', #26855 ) ;
#34850 = DIRECTION ( 'NONE',  ( -1.000000000000000000, -2.280301054154495132E-31, 1.664003471950577689E-31 ) ) ;
#34851 = ORIENTED_EDGE ( 'NONE', *, *, #36156, .F. ) ;
#34852 = ORIENTED_EDGE ( 'NONE', *, *, #6065, .T. ) ;
#34853 = CARTESIAN_POINT ( 'NONE',  ( 0.2666460212928653539, -0.9446779231603621430, 0.7263499614607815680 ) ) ;
#34854 = ORIENTED_EDGE ( 'NONE', *, *, #13789, .T. ) ;
#34855 = ORIENTED_EDGE ( 'NONE', *, *, #6279, .T. ) ;
#34856 = FACE_OUTER_BOUND ( 'NONE', #34686, .T. ) ;
#34857 = CARTESIAN_POINT ( 'NONE',  ( 0.4417433136407998839, -1.573784526376230231, 0.5745458250901962494 ) ) ;
#34859 = CARTESIAN_POINT ( 'NONE',  ( -0.1142670043590661988, -0.4723146173917421309, 0.3382895567580809226 ) ) ;
#34858 = CARTESIAN_POINT ( 'NONE',  ( 0.5208586528260464865, -1.609295453103910090, -0.4933326546058600659 ) ) ;
#34860 = LINE ( 'NONE', #31989, #16546 ) ;
#34861 = CARTESIAN_POINT ( 'NONE',  ( 0.4816455246181599592, -1.076515072263177109, 0.6112998809387040211 ) ) ;
#34862 = CARTESIAN_POINT ( 'NONE',  ( 0.1999999999657006700, -2.081909887788347291, -0.7229608527333891699 ) ) ;
#34863 = CARTESIAN_POINT ( 'NONE',  ( 0.4035771952761294523, -1.734704018191087549, -0.3063975415960173421 ) ) ;
#34864 = CARTESIAN_POINT ( 'NONE',  ( 0.1627274426518589001, -0.7006462241110582578, 0.4958264140424790134 ) ) ;
#34865 = CARTESIAN_POINT ( 'NONE',  ( -0.04760454375021202361, 0.3171166672795173724, -0.3633054878239675989 ) ) ;
#34866 = CARTESIAN_POINT ( 'NONE',  ( 0.1499999999999994948, -0.4638115001430989648, 0.2459753896937853235 ) ) ;
#34867 = CIRCLE ( 'NONE', #17134, 0.4488493849861018292 ) ;
#34868 = DIRECTION ( 'NONE',  ( -1.000000000000000000, -7.857794173099924470E-32, -8.628166150854818811E-32 ) ) ;
#34869 = CARTESIAN_POINT ( 'NONE',  ( 0.5429359209136535025, -1.169310040315109545, 0.5682417262808779901 ) ) ;
#34870 = B_SPLINE_CURVE_WITH_KNOTS ( 'NONE', 3,
 ( #10879, #9704, #37680, #22272, #9898, #19582, #22076, #3312, #38279, #16480 ),
 .UNSPECIFIED., .F., .F.,
 ( 4, 2, 2, 2, 4 ),
 ( 0.000000000000000000, 0.0003203988590849021789, 0.0006407977181698043577, 0.0009611965772547065908, 0.001281595436339608715 ),
 .UNSPECIFIED. ) ;
#34871 = CARTESIAN_POINT ( 'NONE',  ( 0.5104750172518451867, -1.131314744720151477, 0.8088526445616294192 ) ) ;
#34872 = EDGE_CURVE ( 'NONE', #33568, #2775, #6129, .T. ) ;
#34873 = VECTOR ( 'NONE', #30401, 39.37007874015748143 ) ;
#34874 = CYLINDRICAL_SURFACE ( 'NONE', #16176, 0.07999999999999996003 ) ;
#34875 = CARTESIAN_POINT ( 'NONE',  ( 0.06624353298525109679, -1.303414041770764698, 0.6164754190481782636 ) ) ;
#34876 = B_SPLINE_CURVE_WITH_KNOTS ( 'NONE', 3,
 ( #19128, #461, #34744, #31667 ),
 .UNSPECIFIED., .F., .F.,
 ( 4, 4 ),
 ( 0.000000000000000000, 1.000000000000000000 ),
 .UNSPECIFIED. ) ;
#34877 = AXIS2_PLACEMENT_3D ( 'NONE', #28035, #12382, #24937 ) ;
#34878 = CIRCLE ( 'NONE', #30920, 0.01500000000000000291 ) ;
#34879 = ADVANCED_FACE ( 'NONE', ( #30546 ), #39384, .F. ) ;
#34880 = CARTESIAN_POINT ( 'NONE',  ( 0.02238826743734038255, 0.4611641377668463937, -0.2234181651772549626 ) ) ;
#34881 = CARTESIAN_POINT ( 'NONE',  ( 0.4634865284762403892, -1.134362257022321518, -0.3648515278348755109 ) ) ;
#34882 = CARTESIAN_POINT ( 'NONE',  ( 0.1747268316551206235, -0.8716118499233347361, 0.5764457051807095889 ) ) ;
#34883 = CARTESIAN_POINT ( 'NONE',  ( 0.1324860366999178474, 0.05739311687334407164, 0.02052745314230711507 ) ) ;
#34884 = DIRECTION ( 'NONE',  ( 8.881784197001246407E-16, -2.361472542561082612E-16, 1.000000000000000000 ) ) ;
#34885 = VERTEX_POINT ( 'NONE', #5027 ) ;
#34886 = CARTESIAN_POINT ( 'NONE',  ( -0.08000000000000000167, -2.070343076906777213, -0.2454056712452573896 ) ) ;
#34887 = CARTESIAN_POINT ( 'NONE',  ( 0.1641337306192110213, -0.7872022314479601990, 0.5748589285422562867 ) ) ;
#34888 = FACE_OUTER_BOUND ( 'NONE', #28942, .T. ) ;
#34889 = CARTESIAN_POINT ( 'NONE',  ( 0.4368279861777725204, -1.677667223885754844, 0.4182417262808776903 ) ) ;
#34890 = VERTEX_POINT ( 'NONE', #5224 ) ;
#34891 = DIRECTION ( 'NONE',  ( 0.000000000000000000, 0.000000000000000000, -1.000000000000000000 ) ) ;
#34892 = CARTESIAN_POINT ( 'NONE',  ( 0.4115766028365042128, -1.733048369835246794, 0.5182417262812423209 ) ) ;
#34893 = CARTESIAN_POINT ( 'NONE',  ( 0.4605182701905176090, -1.675111011033613817, 0.4442546633674782641 ) ) ;
#34894 = EDGE_CURVE ( 'NONE', #3242, #1535, #1964, .T. ) ;
#34895 = CARTESIAN_POINT ( 'NONE',  ( 0.1909286924077257253, -1.257064795538239466, -0.7137159211901564770 ) ) ;
#34896 = CARTESIAN_POINT ( 'NONE',  ( 0.4790257464341468041, -1.258124379487450817, 0.6720361128856358057 ) ) ;
#34897 = VECTOR ( 'NONE', #13519, 39.37007874015748854 ) ;
#34899 = DIRECTION ( 'NONE',  ( 8.881784197001246407E-16, -2.361472542561082612E-16, 1.000000000000000000 ) ) ;
#34898 = DIRECTION ( 'NONE',  ( -0.000000000000000000, 0.8159412518334725473, 0.5781348229923759519 ) ) ;
#34900 = CARTESIAN_POINT ( 'NONE',  ( 0.4319471385618090520, -1.049247276449186916, 0.6348846931381728620 ) ) ;
#34901 = ORIENTED_EDGE ( 'NONE', *, *, #11681, .F. ) ;
#34902 = EDGE_CURVE ( 'NONE', #31681, #29245, #33834, .T. ) ;
#34903 = APPROVAL_DATE_TIME ( #10017, #4827 ) ;
#34904 = AXIS2_PLACEMENT_3D ( 'NONE', #14994, #24460, #12114 ) ;
#34905 = CARTESIAN_POINT ( 'NONE',  ( 0.09776457712155511848, -1.359218914602520201, 0.6812646313418837529 ) ) ;
#34906 = EDGE_LOOP ( 'NONE', ( #16758, #40367, #9655 ) ) ;
#34907 = ORIENTED_EDGE ( 'NONE', *, *, #9377, .F. ) ;
#34908 = AXIS2_PLACEMENT_3D ( 'NONE', #33629, #27482, #37140 ) ;
#34909 = CARTESIAN_POINT ( 'NONE',  ( 0.3860616713828277091, -1.605769424550066882, 0.5860242868412063322 ) ) ;
#34911 = FACE_OUTER_BOUND ( 'NONE', #6700, .T. ) ;
#34910 = CARTESIAN_POINT ( 'NONE',  ( 0.06503451718542789528, -0.8165451492604878236, 0.07317945280641556527 ) ) ;
#34912 = FACE_BOUND ( 'NONE', #38562, .T. ) ;
#34913 = CIRCLE ( 'NONE', #17172, 0.01500000000000003240 ) ;
#34914 = ORIENTED_EDGE ( 'NONE', *, *, #29900, .F. ) ;
#34915 = AXIS2_PLACEMENT_3D ( 'NONE', #36547, #14329, #26890 ) ;
#34916 = ORIENTED_EDGE ( 'NONE', *, *, #10924, .F. ) ;
#34917 = ORIENTED_EDGE ( 'NONE', *, *, #16732, .F. ) ;
#34918 = CARTESIAN_POINT ( 'NONE',  ( -0.01548846960707490547, 0.09061086148575973886, 0.5171215251571029681 ) ) ;
#34919 = CARTESIAN_POINT ( 'NONE',  ( 0.5669932279378018247, -1.503243827336946392, 0.5741771593363358406 ) ) ;
#34920 = ORIENTED_EDGE ( 'NONE', *, *, #1524, .F. ) ;
#34921 = CARTESIAN_POINT ( 'NONE',  ( 0.07296648554936861764, -1.326663526568328422, 0.4848661492846343402 ) ) ;
#34922 = FACE_OUTER_BOUND ( 'NONE', #35043, .T. ) ;
#34923 = DIRECTION ( 'NONE',  ( 0.000000000000000000, 0.000000000000000000, -1.000000000000000000 ) ) ;
#34924 = DIRECTION ( 'NONE',  ( 0.8660512985181139101, 0.4999551463232363990, 0.000000000000000000 ) ) ;
#34925 = EDGE_LOOP ( 'NONE', ( #21518, #3779, #28795, #39918, #16387, #31283, #26088, #942, #20431, #5648, #21154, #30342 ) ) ;
#34926 = CARTESIAN_POINT ( 'NONE',  ( 0.1840567930975518796, -0.8547793429265486687, 0.1477568935609660794 ) ) ;
#34927 = LINE ( 'NONE', #16226, #383 ) ;
#34928 = CARTESIAN_POINT ( 'NONE',  ( 0.3832704658403437992, -1.758002489716280259, -0.5572338524550815020 ) ) ;
#34929 = AXIS2_PLACEMENT_3D ( 'NONE', #38005, #21985, #19502 ) ;
#34930 = CARTESIAN_POINT ( 'NONE',  ( 0.7185399166019250661, -1.465950542831855330, 0.7545741816404391011 ) ) ;
#34931 = CARTESIAN_POINT ( 'NONE',  ( 0.1988220064826623501, -2.042432882251850934, -0.7119240600711291833 ) ) ;
#34932 = CARTESIAN_POINT ( 'NONE',  ( 0.01548846960707524721, -0.3880410510314797334, -0.3755318131854984420 ) ) ;
#34933 = CARTESIAN_POINT ( 'NONE',  ( 0.3436341067576287323, -1.695284785612029443, -0.4149094092406203638 ) ) ;
#34934 = PERSON_AND_ORGANIZATION ( #28500, #32463 ) ;
#34935 = AXIS2_PLACEMENT_3D ( 'NONE', #34766, #6385, #28008 ) ;
#34936 = EDGE_CURVE ( 'NONE', #9058, #18975, #26305, .T. ) ;
#34937 = CARTESIAN_POINT ( 'NONE',  ( 0.4209912206648682154, -1.078067379053157193, -0.5155029497116575543 ) ) ;
#34938 = DIRECTION ( 'NONE',  ( 0.8660512985181126888, 0.4999551463232384529, 0.000000000000000000 ) ) ;
#34939 = ADVANCED_FACE ( 'NONE', ( #18384 ), #22478, .F. ) ;
#34940 = CARTESIAN_POINT ( 'NONE',  ( 0.4568997192848022748, -1.218890999244366613, 0.6057417262810179670 ) ) ;
#34941 = DIRECTION ( 'NONE',  ( 0.000000000000000000, 3.330669073875470114E-16, 1.000000000000000000 ) ) ;
#34942 = CARTESIAN_POINT ( 'NONE',  ( 0.03167879690716527558, -0.8799939210571326997, 0.6541495583543271986 ) ) ;
#34943 = CARTESIAN_POINT ( 'NONE',  ( 0.6004354142920773629, -1.537439897621929896, -0.4422550059529070654 ) ) ;
#34944 = AXIS2_PLACEMENT_3D ( 'NONE', #38686, #3920, #293 ) ;
#34945 = CARTESIAN_POINT ( 'NONE',  ( 0.1973311420822173867, -2.025401704179647933, -0.7077925230234759502 ) ) ;
#34946 = DIRECTION ( 'NONE',  ( 0.000000000000000000, 0.000000000000000000, 1.000000000000000000 ) ) ;
#34947 = VERTEX_POINT ( 'NONE', #16088 ) ;
#34948 = VERTEX_POINT ( 'NONE', #13388 ) ;
#34949 = CARTESIAN_POINT ( 'NONE',  ( 0.01548846960712814240, 0.3688619771571980954, 0.3775276577326248106 ) ) ;
#34950 = EDGE_LOOP ( 'NONE', ( #16038, #25057, #17684, #19035 ) ) ;
#34951 = CARTESIAN_POINT ( 'NONE',  ( 0.3549495572495519058, -1.751088804252343145, 0.4457772353421656786 ) ) ;
#34952 = CARTESIAN_POINT ( 'NONE',  ( 0.05999999999999990757, 0.000000000000000000, 0.000000000000000000 ) ) ;
#34953 = CARTESIAN_POINT ( 'NONE',  ( 0.3941551577388408556, -1.134933593074018310, 0.8127732636010218670 ) ) ;
#34955 = ORIENTED_EDGE ( 'NONE', *, *, #160, .T. ) ;
#34954 = DIRECTION ( 'NONE',  ( 0.000000000000000000, 3.414809992080318472E-15, -1.000000000000000000 ) ) ;
#34956 = CIRCLE ( 'NONE', #13914, 0.03000000000000008910 ) ;
#34957 = VERTEX_POINT ( 'NONE', #29232 ) ;
#34958 = CARTESIAN_POINT ( 'NONE',  ( 0.1978587402095111636, -0.5849795632145003976, 0.3178455878192510409 ) ) ;
#34959 = ORIENTED_EDGE ( 'NONE', *, *, #35299, .T. ) ;
#34960 = CARTESIAN_POINT ( 'NONE',  ( 0.2972703710326047299, -1.656711430450878986, 0.5747086054135303046 ) ) ;
#34962 = CARTESIAN_POINT ( 'NONE',  ( 0.1121305562899380798, -0.8343818903186780434, -0.04602629424161558402 ) ) ;
#34961 = CARTESIAN_POINT ( 'NONE',  ( 0.6205237272702224249, -1.594602023479971153, 0.4300673587497688133 ) ) ;
#34963 = CARTESIAN_POINT ( 'NONE',  ( -0.01548846960707477016, 0.4638115001430989648, -0.2459753896937820483 ) ) ;
#34964 = DIRECTION ( 'NONE',  ( 0.000000000000000000, 0.000000000000000000, -1.000000000000000000 ) ) ;
#34965 = B_SPLINE_CURVE_WITH_KNOTS ( 'NONE', 3,
 ( #36260, #18360, #26829, #36872, #23736, #33192 ),
 .UNSPECIFIED., .F., .F.,
 ( 4, 2, 4 ),
 ( 4.906538933386825900E-18, 0.0003977219821689530698, 0.0007954439643379011523 ),
 .UNSPECIFIED. ) ;
#34966 = CARTESIAN_POINT ( 'NONE',  ( 0.4141786054075141665, -1.705102989373699529, 0.4226014444323759611 ) ) ;
#34968 = EDGE_LOOP ( 'NONE', ( #7922, #19646, #13111, #2872, #5292, #40038 ) ) ;
#34967 = ORIENTED_EDGE ( 'NONE', *, *, #23535, .F. ) ;
#34969 = FACE_OUTER_BOUND ( 'NONE', #15718, .T. ) ;
#34970 = CARTESIAN_POINT ( 'NONE',  ( 0.1862284309081393141, -0.9153619266321347814, 0.1521157592012398474 ) ) ;
#34971 = CARTESIAN_POINT ( 'NONE',  ( 0.1989976604547370465, -2.047409678865564686, -0.7132172901365274598 ) ) ;
#34972 = CARTESIAN_POINT ( 'NONE',  ( 0.5955365829513108444, -1.457654325452099275, 0.6080873925085832354 ) ) ;
#34973 = CIRCLE ( 'NONE', #33634, 0.03000000000000022787 ) ;
#34974 = CIRCLE ( 'NONE', #864, 0.03000000000000022787 ) ;
#34975 = CARTESIAN_POINT ( 'NONE',  ( 0.3692778306978620750, -1.136428696002824701, 0.7302004567001213475 ) ) ;
#34976 = CARTESIAN_POINT ( 'NONE',  ( 0.01703122118373576882, -0.6267681536281951571, 0.4285498985508694458 ) ) ;
#34977 = DIRECTION ( 'NONE',  ( 1.000000000000000000, 6.779273404243070203E-32, 4.314083075427408311E-32 ) ) ;
#34978 = CARTESIAN_POINT ( 'NONE',  ( -0.002308984842514968851, -0.8531871666706627444, 0.1457185332388709897 ) ) ;
#34979 = LINE ( 'NONE', #25337, #31143 ) ;
#34980 = CARTESIAN_POINT ( 'NONE',  ( 0.4299615998478440448, -1.187820293361493640, 0.7150245015202120191 ) ) ;
#34981 = CARTESIAN_POINT ( 'NONE',  ( -0.1873388932668322848, 0.5325605939836577374, 0.08500000000000018652 ) ) ;
#34982 = DIRECTION ( 'NONE',  ( 0.000000000000000000, 0.000000000000000000, 1.000000000000000000 ) ) ;
#34983 = DIRECTION ( 'NONE',  ( 0.000000000000000000, 0.000000000000000000, -1.000000000000000000 ) ) ;
#34984 = DIRECTION ( 'NONE',  ( 1.000000000000000000, 1.138269997360102279E-15, -8.537024980200767584E-16 ) ) ;
#34985 = CARTESIAN_POINT ( 'NONE',  ( 0.1742107032092684304, -1.802736856131804011, -0.6515483580219902926 ) ) ;
#34986 = DATE_AND_TIME ( #34378, #21432 ) ;
#34987 = CARTESIAN_POINT ( 'NONE',  ( 0.2100859181409473475, -1.630899271293733355, -0.6615904437728673537 ) ) ;
#34988 = CIRCLE ( 'NONE', #40237, 0.02999999999999998848 ) ;
#34989 = CARTESIAN_POINT ( 'NONE',  ( -0.02881195911415162028, 0.4889334074056331247, 0.09563129189200904323 ) ) ;
#34990 = CARTESIAN_POINT ( 'NONE',  ( 0.2914323826288400254, -1.233685883474753497, -0.5166151207188711680 ) ) ;
#34991 = AXIS2_PLACEMENT_3D ( 'NONE', #4514, #8219, #10916 ) ;
#34992 = VECTOR ( 'NONE', #29630, 39.37007874015748854 ) ;
#34993 = ORIENTED_EDGE ( 'NONE', *, *, #25847, .T. ) ;
#34994 = CARTESIAN_POINT ( 'NONE',  ( 0.3854339232390436298, -1.140486404647998775, 0.4306521322894901194 ) ) ;
#34995 = ORIENTED_EDGE ( 'NONE', *, *, #17301, .F. ) ;
#34996 = CARTESIAN_POINT ( 'NONE',  ( 0.1499999999999993561, 0.000000000000000000, 0.000000000000000000 ) ) ;
#34997 = CARTESIAN_POINT ( 'NONE',  ( 0.2739389673431911199, -1.670182469438165507, 0.6632468065124506040 ) ) ;
#34998 = CARTESIAN_POINT ( 'NONE',  ( 0.5244453523138082884, -1.387307315266893104, 0.7902440572305963196 ) ) ;
#35000 = ORIENTED_EDGE ( 'NONE', *, *, #13484, .T. ) ;
#34999 = FACE_OUTER_BOUND ( 'NONE', #33241, .T. ) ;
#35002 = VERTEX_POINT ( 'NONE', #23067 ) ;
#35001 = VERTEX_POINT ( 'NONE', #19576 ) ;
#35003 = CARTESIAN_POINT ( 'NONE',  ( -0.1210148435730249716, -0.5061394519557976812, 0.3122829191278992389 ) ) ;
#35004 = EDGE_LOOP ( 'NONE', ( #39122, #10528, #37038, #24157 ) ) ;
#35005 = CIRCLE ( 'NONE', #2824, 0.01000000000000002970 ) ;
#35006 = CARTESIAN_POINT ( 'NONE',  ( -0.1655961216393919966, 0.4810575411953317282, 0.1221435944151032377 ) ) ;
#35007 = ITEM_DEFINED_TRANSFORMATION ( 'NONE', 'NONE', #40373,  #27819 ) ;
#35008 = DIRECTION ( 'NONE',  ( 0.000000000000000000, 0.000000000000000000, -1.000000000000000000 ) ) ;
#35009 = ORIENTED_EDGE ( 'NONE', *, *, #23579, .F. ) ;
#35010 = CARTESIAN_POINT ( 'NONE',  ( 0.09262370799349907424, -0.7550308318057149526, 0.2814015553635414446 ) ) ;
#35011 = CARTESIAN_POINT ( 'NONE',  ( 0.06924732741833404537, -0.5400192420372453839, 0.1478676264384281847 ) ) ;
#35012 = CARTESIAN_POINT ( 'NONE',  ( 0.4649247847684765400, -1.394123109563673468, 0.8177829614335009323 ) ) ;
#35013 = CARTESIAN_POINT ( 'NONE',  ( 0.5747588096728203366, -1.612720233196342168, -0.5227372493886142113 ) ) ;
#35014 = CARTESIAN_POINT ( 'NONE',  ( -0.1529829672178560085, 0.4739133692255316777, 0.09550516375522978552 ) ) ;
#35015 = CARTESIAN_POINT ( 'NONE',  ( -0.1663058949915988405, 0.5166728756553480295, 0.1255325300626448648 ) ) ;
#35016 = CIRCLE ( 'NONE', #27807, 0.1749999999999999889 ) ;
#35017 = CARTESIAN_POINT ( 'NONE',  ( 0.3424019376673626547, -1.758881546318450395, 0.5758682293985877276 ) ) ;
#35018 = CARTESIAN_POINT ( 'NONE',  ( 0.7337022410813530682, -1.492415808383954046, 0.7062599971678739097 ) ) ;
#35019 = EDGE_CURVE ( 'NONE', #23130, #35163, #10106, .T. ) ;
#35020 = CARTESIAN_POINT ( 'NONE',  ( 0.4902907973143189047, -1.608820546470212109, -0.6381618420067222130 ) ) ;
#35021 = VECTOR ( 'NONE', #3867, 39.37007874015748143 ) ;
#35022 = CARTESIAN_POINT ( 'NONE',  ( 0.1358623780661346869, -0.5778457909491311328, 0.2559053680288311816 ) ) ;
#35023 = CIRCLE ( 'NONE', #6796, 0.01499999999999997863 ) ;
#35024 = CARTESIAN_POINT ( 'NONE',  ( -0.1664683893528073888, 0.5171715631282249870, 0.3299773601679621415 ) ) ;
#35025 =( CONVERSION_BASED_UNIT ( 'INCH', #22301 ) LENGTH_UNIT ( ) NAMED_UNIT ( #38313 ) );
#35026 = FACE_OUTER_BOUND ( 'NONE', #24187, .T. ) ;
#35027 = CARTESIAN_POINT ( 'NONE',  ( 0.4320371192881574118, -1.117877429793240118, -0.3862585142794699444 ) ) ;
#35028 = CARTESIAN_POINT ( 'NONE',  ( 0.05992090360963521489, -1.332693131100006978, 0.5682417262808777680 ) ) ;
#35029 = VECTOR ( 'NONE', #20229, 39.37007874015748143 ) ;
#35030 = CARTESIAN_POINT ( 'NONE',  ( 0.3382833150183324755, -0.9396054708716727877, 0.6333258291577809063 ) ) ;
#35031 = COORDINATED_UNIVERSAL_TIME_OFFSET ( 0, 0, .AHEAD. ) ;
#35032 = DIRECTION ( 'NONE',  ( -0.4999551463232377313, 0.8660512985181132439, -0.000000000000000000 ) ) ;
#35033 = CIRCLE ( 'NONE', #39640, 0.1000000000000000194 ) ;
#35034 = ADVANCED_FACE ( 'NONE', ( #7010 ), #8280, .T. ) ;
#35035 = APPLIED_DATE_AND_TIME_ASSIGNMENT ( #13826, #14037, ( #40563 ) ) ;
#35036 = CARTESIAN_POINT ( 'NONE',  ( -0.03158843595483506322, 0.4482533282648962225, -0.2030547983902464548 ) ) ;
#35037 = CARTESIAN_POINT ( 'NONE',  ( 0.4076976354719489271, -1.154888438488554270, 0.4182417262808778013 ) ) ;
#35038 = ORIENTED_EDGE ( 'NONE', *, *, #5688, .T. ) ;
#35039 = CARTESIAN_POINT ( 'NONE',  ( 0.4338200250350727205, -1.578845347063857707, 0.5905617543171319817 ) ) ;
#35040 = CARTESIAN_POINT ( 'NONE',  ( 1.530770926392632502E-17, 0.06117178301711245075, 0.1249999999999993477 ) ) ;
#35041 = AXIS2_PLACEMENT_3D ( 'NONE', #3812, #23165, #31805 ) ;
#35042 = CARTESIAN_POINT ( 'NONE',  ( 0.08636663003170327868, -0.7620321640752294456, 0.04754930498978150732 ) ) ;
#35043 = EDGE_LOOP ( 'NONE', ( #423, #38892, #21810 ) ) ;
#35044 = CARTESIAN_POINT ( 'NONE',  ( 0.3211756810167746834, -1.183199798883805887, 0.5707417262808780478 ) ) ;
#35045 = CARTESIAN_POINT ( 'NONE',  ( -0.01481790428398078660, -0.8502221965164611373, 0.2178672377299346041 ) ) ;
#35047 = VERTEX_POINT ( 'NONE', #29838 ) ;
#35046 = ORIENTED_EDGE ( 'NONE', *, *, #17337, .T. ) ;
#35048 = CARTESIAN_POINT ( 'NONE',  ( -0.3000000000000000999, -2.423474325126674156, -0.5576739111151496342 ) ) ;
#35049 = AXIS2_PLACEMENT_3D ( 'NONE', #4282, #16849, #39040 ) ;
#35050 = VECTOR ( 'NONE', #36571, 39.37007874015748143 ) ;
#35051 = EDGE_CURVE ( 'NONE', #17498, #11318, #8222, .T. ) ;
#35052 = ORIENTED_EDGE ( 'NONE', *, *, #36086, .F. ) ;
#35053 = CARTESIAN_POINT ( 'NONE',  ( 0.3177856290042974652, -1.645584934368151009, 0.5182417262812344383 ) ) ;
#35054 = PRODUCT ( 'Cage Hanger', 'Cage Hanger', '', ( #28455 ) ) ;
#35055 = CARTESIAN_POINT ( 'NONE',  ( 0.3831477286273856087, -1.691467851574164127, -0.3353491032924195148 ) ) ;
#35056 = CARTESIAN_POINT ( 'NONE',  ( -0.2666757540196708076, 0.4921670437878968851, 0.3749999999999999445 ) ) ;
#35057 = DIRECTION ( 'NONE',  ( 0.000000000000000000, 0.000000000000000000, -1.000000000000000000 ) ) ;
#35058 = ORIENTED_EDGE ( 'NONE', *, *, #12663, .T. ) ;
#35059 = CARTESIAN_POINT ( 'NONE',  ( 0.01562500000000000694, -0.4290069966815239777, 0.1457185332388690469 ) ) ;
#35060 = EDGE_CURVE ( 'NONE', #38034, #28698, #4328, .T. ) ;
#35061 = VERTEX_POINT ( 'NONE', #35802 ) ;
#35062 = CARTESIAN_POINT ( 'NONE',  ( 0.09694602640260427395, -0.6285277416443179055, 0.3013455349893560675 ) ) ;
#35063 = B_SPLINE_CURVE_WITH_KNOTS ( 'NONE', 3,
 ( #33120, #26351, #4517, #17495, #29434, #29839 ),
 .UNSPECIFIED., .F., .F.,
 ( 4, 2, 4 ),
 ( 0.002802047142276813813, 0.003388785079928784139, 0.003975523017580754465 ),
 .UNSPECIFIED. ) ;
#35064 = VERTEX_POINT ( 'NONE', #11312 ) ;
#35065 = EDGE_CURVE ( 'NONE', #34712, #15439, #10633, .T. ) ;
#35066 = CARTESIAN_POINT ( 'NONE',  ( 0.03852295281450220099, -0.6922990027746789288, 0.6869434594017632678 ) ) ;
#35067 = CARTESIAN_POINT ( 'NONE',  ( 0.2743735404850286552, -1.090822434421504505, 0.8247435112018880465 ) ) ;
#35068 = AXIS2_PLACEMENT_3D ( 'NONE', #35634, #26802, #20834 ) ;
#35070 = DIRECTION ( 'NONE',  ( -1.000000000000000000, 0.000000000000000000, 0.000000000000000000 ) ) ;
#35069 = CARTESIAN_POINT ( 'NONE',  ( 0.4680314439923284886, -1.633517906973578349, -0.4203363782011557692 ) ) ;
#35071 = DIRECTION ( 'NONE',  ( -1.000000000000000000, -0.000000000000000000, -0.000000000000000000 ) ) ;
#35072 = CARTESIAN_POINT ( 'NONE',  ( 0.3048716024861035101, -0.9795252986220516211, 0.5672847750834353331 ) ) ;
#35073 = EDGE_CURVE ( 'NONE', #357, #12314, #7189, .T. ) ;
#35074 = UNCERTAINTY_MEASURE_WITH_UNIT (LENGTH_MEASURE( 1.000000000000000082E-05 ), #39522, 'distance_accuracy_value', 'NONE');
#35075 = EDGE_CURVE ( 'NONE', #34796, #14911, #17079, .T. ) ;
#35076 = LINE ( 'NONE', #6879, #14067 ) ;
#35077 = CARTESIAN_POINT ( 'NONE',  ( 0.1897112079047654776, -0.5340520988485685239, 0.1446142472693987546 ) ) ;
#35078 = EDGE_CURVE ( 'NONE', #23695, #4081, #36618, .T. ) ;
#35079 = CARTESIAN_POINT ( 'NONE',  ( -0.05269191099235902981, 0.2718205810684086177, -0.3817379850160022015 ) ) ;
#35080 =( BOUNDED_SURFACE ( )  B_SPLINE_SURFACE ( 3, 2, ( 
 ( #11960, #14423, #2514 ),
 ( #4968, #30694, #33767 ),
 ( #36842, #23923, #29883 ),
 ( #26990, #27418, #36654 ),
 ( #14240, #30265, #36453 ),
 ( #26804, #39330, #8875 ),
 ( #24524, #17535, #27601 ),
 ( #27204, #21025, #30084 ),
 ( #33548, #24317, #14853 ),
 ( #5358, #17920, #1912 ) ),
 .UNSPECIFIED., .F., .F., .T. ) 
 B_SPLINE_SURFACE_WITH_KNOTS ( ( 4, 2, 2, 2, 4 ),
 ( 3, 3 ),
 ( 0.002207820581699636471, 0.002505005507268364285, 0.002802190432837092099, 0.003099375358405819913, 0.003396560283974547727 ),
 ( 0.000000000000000000, 1.000000000000000000 ),
 .UNSPECIFIED. ) 
 GEOMETRIC_REPRESENTATION_ITEM ( )  RATIONAL_B_SPLINE_SURFACE ( (
 ( 1.000000000000000000, 0.5517613080878712717, 1.000000000000000000),
 ( 1.000000000000000000, 0.5512582163888796183, 1.000000000000000000),
 ( 1.000000000000000000, 0.5482345409571344197, 1.000000000000000000),
 ( 1.000000000000000000, 0.5377007643832122374, 1.000000000000000000),
 ( 1.000000000000000000, 0.5301184884994317725, 1.000000000000000000),
 ( 1.000000000000000000, 0.5117099482123855791, 1.000000000000000000),
 ( 1.000000000000000000, 0.5010294111536789385, 1.000000000000000000),
 ( 1.000000000000000000, 0.4783064819327327855, 1.000000000000000000),
 ( 1.000000000000000000, 0.4661873777990636625, 1.000000000000000000),
 ( 1.000000000000000000, 0.4546663607401262852, 1.000000000000000000) ) ) 
 REPRESENTATION_ITEM ( '' )  SURFACE ( )  );
#35081 = CARTESIAN_POINT ( 'NONE',  ( -0.1061036098701634706, -0.4827967145417200179, 0.3599999999999998757 ) ) ;
#35082 = AXIS2_PLACEMENT_3D ( 'NONE', #6311, #11870, #6096 ) ;
#35083 = DIRECTION ( 'NONE',  ( 0.000000000000000000, 0.5877852522925025580, 0.8090169943749260240 ) ) ;
#35084 = CARTESIAN_POINT ( 'NONE',  ( 0.6265937217076796850, -1.312621381056858993, 0.7675331558851111735 ) ) ;
#35085 = AXIS2_PLACEMENT_3D ( 'NONE', #14491, #27059, #4229 ) ;
#35086 = AXIS2_PLACEMENT_3D ( 'NONE', #28182, #27984, #12539 ) ;
#35087 = DIRECTION ( 'NONE',  ( 0.2577569635876607590, 0.1487982532522210410, -0.9546834174485054891 ) ) ;
#35088 = EDGE_CURVE ( 'NONE', #28384, #10719, #28257, .T. ) ;
#35089 = CARTESIAN_POINT ( 'NONE',  ( 0.02106135308996504724, -1.064028623006035845, 0.6283655268256098658 ) ) ;
#35090 = PRODUCT_RELATED_PRODUCT_CATEGORY ( 'detail', '', ( #30071 ) ) ;
#35091 = CARTESIAN_POINT ( 'NONE',  ( 0.03674078017396296275, 0.4681991728402117303, -0.1092756390057526977 ) ) ;
#35092 = CARTESIAN_POINT ( 'NONE',  ( 0.1905436384893574864, -0.5945559727383912252, 0.3046096357648204189 ) ) ;
#35093 = CARTESIAN_POINT ( 'NONE',  ( 0.3303338544634616958, -1.053644867167129240, 0.7371517169581325302 ) ) ;
#35094 = CARTESIAN_POINT ( 'NONE',  ( 0.01548846960721255751, -0.3688619771570325612, 0.3775276577325259453 ) ) ;
#35095 = AXIS2_PLACEMENT_3D ( 'NONE', #18045, #30602, #2426 ) ;
#35096 = CARTESIAN_POINT ( 'NONE',  ( -0.02000000000000000042, -2.626773565144302935, -0.1926934094652516249 ) ) ;
#35097 = CIRCLE ( 'NONE', #17365, 0.07999999999999996003 ) ;
#35098 = VERTEX_POINT ( 'NONE', #13984 ) ;
#35099 = CARTESIAN_POINT ( 'NONE',  ( 0.4621675984227249789, -1.110867290327286261, 0.5635151220948720896 ) ) ;
#35100 = CARTESIAN_POINT ( 'NONE',  ( 0.4013540502050752523, -1.148216799725839232, 0.7886735227232307688 ) ) ;
#35101 = CARTESIAN_POINT ( 'NONE',  ( 0.4909801108973092520, -1.199306193601649362, -0.5155029497116575543 ) ) ;
#35102 = CARTESIAN_POINT ( 'NONE',  ( 0.3445284778472457732, -1.145141864321415515, 0.5942735951974011943 ) ) ;
#35103 = VERTEX_POINT ( 'NONE', #24694 ) ;
#35104 = CARTESIAN_POINT ( 'NONE',  ( -0.1593715683900588098, 0.4948507460962289217, 0.3535463917166351555 ) ) ;
#35105 = DIRECTION ( 'NONE',  ( 0.8660512985181133550, 0.4999551463232373982, 0.000000000000000000 ) ) ;
#35106 = CARTESIAN_POINT ( 'NONE',  ( 0.1856347024191063455, -0.7573053249172038148, 0.1605899983602313563 ) ) ;
#35107 = DIRECTION ( 'NONE',  ( 0.4999551463232385085, -0.8660512985181127998, 0.000000000000000000 ) ) ;
#35108 = AXIS2_PLACEMENT_3D ( 'NONE', #29912, #4780, #11177 ) ;
#35109 = CARTESIAN_POINT ( 'NONE',  ( 0.4897466037307776077, -1.275248307527913960, 0.6033332196752250187 ) ) ;
#35111 = DIRECTION ( 'NONE',  ( 0.4999551463232372317, -0.8660512985181135770, 0.000000000000000000 ) ) ;
#35110 = DIRECTION ( 'NONE',  ( 0.8660512985181134660, 0.4999551463232373427, 0.000000000000000000 ) ) ;
#35112 = CARTESIAN_POINT ( 'NONE',  ( 0.4646871136015383597, -1.067210575163276776, 0.6251146133038130159 ) ) ;
#35113 = ORIENTED_EDGE ( 'NONE', *, *, #24326, .T. ) ;
#35115 = CIRCLE ( 'NONE', #27258, 0.07999999999999996003 ) ;
#35114 = COORDINATED_UNIVERSAL_TIME_OFFSET ( 0, 0, .AHEAD. ) ;
#35116 = CARTESIAN_POINT ( 'NONE',  ( 0.0004665802737306216875, -0.8700472974049004993, 0.3726199621362326075 ) ) ;
#35117 = ORIENTED_EDGE ( 'NONE', *, *, #9756, .T. ) ;
#35118 = CIRCLE ( 'NONE', #30539, 0.01000000000000000194 ) ;
#35119 = EDGE_CURVE ( 'NONE', #22855, #7075, #31051, .T. ) ;
#35120 = EDGE_LOOP ( 'NONE', ( #39153, #37420, #17252, #10186 ) ) ;
#35121 = VECTOR ( 'NONE', #37574, 39.37007874015748143 ) ;
#35122 = CARTESIAN_POINT ( 'NONE',  ( 0.04802164911735522929, -0.5370111569602100676, 0.1635350359062409942 ) ) ;
#35124 = CARTESIAN_POINT ( 'NONE',  ( 0.1743516220684620532, -0.9173990847765624013, 0.1503757705193672634 ) ) ;
#35123 = CARTESIAN_POINT ( 'NONE',  ( 0.06637331517990789631, -0.7260456777667779749, 0.002854135229572256870 ) ) ;
#35125 = DIRECTION ( 'NONE',  ( 0.000000000000000000, 0.8159412518334726583, 0.5781348229923756188 ) ) ;
#35126 = VERTEX_POINT ( 'NONE', #40512 ) ;
#35127 = ADVANCED_FACE ( 'NONE', ( #27564 ), #8776, .F. ) ;
#35128 = ORIENTED_EDGE ( 'NONE', *, *, #40550, .T. ) ;
#35129 = LINE ( 'NONE', #35332, #7663 ) ;
#35130 = ADVANCED_FACE ( 'NONE', ( #33504 ), #31267, .T. ) ;
#35131 = CARTESIAN_POINT ( 'NONE',  ( 0.5667909668417350222, -1.503200344063986282, 0.5705455483130308370 ) ) ;
#35132 = ORIENTED_EDGE ( 'NONE', *, *, #27357, .T. ) ;
#35133 = AXIS2_PLACEMENT_3D ( 'NONE', #26430, #38967, #23369 ) ;
#35134 = CARTESIAN_POINT ( 'NONE',  ( 0.3895823661253040027, -1.931635654259855173, -0.5036415101835181041 ) ) ;
#35135 = CARTESIAN_POINT ( 'NONE',  ( 0.4806378395295556882, -1.105637800341302102, -0.6194292131661300882 ) ) ;
#35136 = DIRECTION ( 'NONE',  ( -0.3468893892380662258, 0.7770416411310642202, 0.5252371270030176120 ) ) ;
#35137 = CYLINDRICAL_SURFACE ( 'NONE', #19842, 0.08000000000000000167 ) ;
#35138 = DIRECTION ( 'NONE',  ( 0.000000000000000000, 0.000000000000000000, -1.000000000000000000 ) ) ;
#35139 = DIRECTION ( 'NONE',  ( 0.000000000000000000, 0.000000000000000000, -1.000000000000000000 ) ) ;
#35140 = FACE_OUTER_BOUND ( 'NONE', #13798, .T. ) ;
#35141 = CARTESIAN_POINT ( 'NONE',  ( 0.01548846960707511190, -0.2372406987223689145, -0.4850946823762606330 ) ) ;
#35142 = CARTESIAN_POINT ( 'NONE',  ( 0.3981442986168809428, -2.030926130361281334, -0.7104987781722165163 ) ) ;
#35143 = EDGE_CURVE ( 'NONE', #15479, #11782, #19311, .T. ) ;
#35144 = CARTESIAN_POINT ( 'NONE',  ( 0.07043814880410684265, -1.334972480813831242, 0.5056242588139928662 ) ) ;
#35145 = CARTESIAN_POINT ( 'NONE',  ( 0.2011892967074957184, -1.251141541415955682, -0.7187326247832955817 ) ) ;
#35146 = APPROVAL_ROLE ( '' ) ;
#35147 = EDGE_CURVE ( 'NONE', #39770, #27951, #21948, .T. ) ;
#35148 = CIRCLE ( 'NONE', #36461, 0.1000000000000000194 ) ;
#35149 = CARTESIAN_POINT ( 'NONE',  ( 0.1637488714925408873, -0.5994898440788770655, 0.1932149833450298726 ) ) ;
#35150 = ADVANCED_FACE ( 'NONE', ( #9226 ), #21606, .T. ) ;
#35151 = AXIS2_PLACEMENT_3D ( 'NONE', #21069, #39978, #33596 ) ;
#35152 = DIRECTION ( 'NONE',  ( 0.000000000000000000, 0.000000000000000000, -1.000000000000000000 ) ) ;
#35153 = CARTESIAN_POINT ( 'NONE',  ( 0.6638964227572436982, -1.375154404986101531, 0.8002223753517787586 ) ) ;
#35154 = DIRECTION ( 'NONE',  ( 1.000000000000000000, 0.000000000000000000, 0.000000000000000000 ) ) ;
#35155 = B_SPLINE_CURVE_WITH_KNOTS ( 'NONE', 3,
 ( #25208, #9153, #31186, #28492 ),
 .UNSPECIFIED., .F., .F.,
 ( 4, 4 ),
 ( 0.000000000000000000, 0.0005696446236587841307 ),
 .UNSPECIFIED. ) ;
#35156 = LINE ( 'NONE', #6956, #35021 ) ;
#35157 = VECTOR ( 'NONE', #2766, 39.37007874015748143 ) ;
#35158 = APPLIED_APPROVAL_ASSIGNMENT ( #13450, ( #19398 ) ) ;
#35159 = CARTESIAN_POINT ( 'NONE',  ( 0.004343411016521666126, -0.7362306918419727619, 0.3916307744012189618 ) ) ;
#35160 = CARTESIAN_POINT ( 'NONE',  ( -0.0003491300308188850007, -0.9207945218656948816, 0.05792235683160573689 ) ) ;
#35161 = CARTESIAN_POINT ( 'NONE',  ( 0.1929609155355634653, -1.992353606873398020, -0.7010103324791125967 ) ) ;
#35162 = PLANE ( 'NONE',  #13866 ) ;
#35163 = VERTEX_POINT ( 'NONE', #24892 ) ;
#35164 = ORIENTED_EDGE ( 'NONE', *, *, #514, .T. ) ;
#35165 = CARTESIAN_POINT ( 'NONE',  ( 0.3757471142192235214, -1.766731021160328874, -0.5680748514784772496 ) ) ;
#35166 = ORIENTED_EDGE ( 'NONE', *, *, #20496, .T. ) ;
#35167 = CARTESIAN_POINT ( 'NONE',  ( 0.3499317094845083576, -1.754137739073151847, 0.4513909310129906038 ) ) ;
#35168 = CARTESIAN_POINT ( 'NONE',  ( 0.3432713340272304237, -1.639810668526975324, -0.4375135453339642488 ) ) ;
#35169 = CYLINDRICAL_SURFACE ( 'NONE', #9853, 0.03749999999977557397 ) ;
#35171 = EDGE_LOOP ( 'NONE', ( #30667, #20802, #11366, #31426, #13142, #24400 ) ) ;
#35170 = CARTESIAN_POINT ( 'NONE',  ( 0.5669405059600367558, -1.627145089617755058, 0.5182417262812432091 ) ) ;
#35172 = CARTESIAN_POINT ( 'NONE',  ( 0.1880247778135462344, -0.6881053353252821747, 0.1842137475136224611 ) ) ;
#35173 = ORIENTED_EDGE ( 'NONE', *, *, #37719, .T. ) ;
#35174 = CARTESIAN_POINT ( 'NONE',  ( 0.5596770508836024227, -1.621439871647906816, 0.5567351769756754276 ) ) ;
#35175 = ORIENTED_EDGE ( 'NONE', *, *, #1321, .T. ) ;
#35176 = CARTESIAN_POINT ( 'NONE',  ( 0.03160920193218080126, -0.6779490433875170474, 0.5099419547340309222 ) ) ;
#35178 = CARTESIAN_POINT ( 'NONE',  ( -0.01895494625228204277, -0.2428766181966267312, 0.4598657641708858157 ) ) ;
#35177 = CARTESIAN_POINT ( 'NONE',  ( 0.5477732146854656925, -1.663038142904176730, -0.4856124366662120662 ) ) ;
#35179 = CARTESIAN_POINT ( 'NONE',  ( 0.3169360506679547163, -1.762143365380179461, 0.5416432108594028128 ) ) ;
#35180 = CARTESIAN_POINT ( 'NONE',  ( 0.01191963247266815060, -0.5294101887948575724, -0.06017522680174922783 ) ) ;
#35181 = AXIS2_PLACEMENT_3D ( 'NONE', #12598, #25157, #9520 ) ;
#35182 = EDGE_CURVE ( 'NONE', #30280, #13990, #33945, .T. ) ;
#35183 = CARTESIAN_POINT ( 'NONE',  ( 0.02145472682158336766, -1.629281619508914591, -0.3446454179893428948 ) ) ;
#35185 = EDGE_LOOP ( 'NONE', ( #19295, #4133, #9234, #26227 ) ) ;
#35184 = ORIENTED_EDGE ( 'NONE', *, *, #32376, .F. ) ;
#35186 = AXIS2_PLACEMENT_3D ( 'NONE', #37740, #23298, #22139 ) ;
#35187 = TOROIDAL_SURFACE ( 'NONE', #3634, 0.1700000000000000400, 0.02999999999999999889 ) ;
#35188 = EDGE_CURVE ( 'NONE', #20386, #1061, #36, .T. ) ;
#35189 = DIRECTION ( 'NONE',  ( 1.000000000000000000, -0.000000000000000000, -0.000000000000000000 ) ) ;
#35190 = CARTESIAN_POINT ( 'NONE',  ( 0.1109049718728688100, -0.9286333055842341810, 0.1423358669777867735 ) ) ;
#35191 = CARTESIAN_POINT ( 'NONE',  ( -0.03664605387828188954, -0.04106737781738599435, -0.4792329708773129804 ) ) ;
#35192 = CARTESIAN_POINT ( 'NONE',  ( -0.2399999999999999079, -4.074947978347777777, -0.4909924454747331413 ) ) ;
#35193 = CARTESIAN_POINT ( 'NONE',  ( 0.2925246921984026582, -1.120422423083942132, 0.7434686055759071044 ) ) ;
#35194 = LOCAL_TIME ( 0, 53, 7.000000000000000000, #16932 ) ;
#35195 = CARTESIAN_POINT ( 'NONE',  ( 0.01071266088865911389, -0.5421084299554996822, 0.2199866464733553073 ) ) ;
#35196 = CARTESIAN_POINT ( 'NONE',  ( 0.1109092093543055241, -0.9286325583098424818, 0.1457252011008478843 ) ) ;
#35197 = AXIS2_PLACEMENT_3D ( 'NONE', #8212, #17669, #17275 ) ;
#35198 = CARTESIAN_POINT ( 'NONE',  ( -0.1508021419688934661, 0.4665171419162789102, 0.3472338286680812791 ) ) ;
#35199 = CARTESIAN_POINT ( 'NONE',  ( 0.06843411546424661707, -1.327640554429453168, 0.5682417262808774350 ) ) ;
#35200 = DIRECTION ( 'NONE',  ( -0.3468893892380670585, 0.3199132558031868578, 0.8816593788960934708 ) ) ;
#35201 = DIRECTION ( 'NONE',  ( 2.374158975444574710E-12, 1.370557379215330847E-12, 1.000000000000000000 ) ) ;
#35202 = DIRECTION ( 'NONE',  ( 1.188678714063518030E-15, -1.000000000000000000, 3.676620095425087714E-16 ) ) ;
#35203 = CARTESIAN_POINT ( 'NONE',  ( 0.1793995099104103708, -0.4942854820514369085, 0.1284778566484219009 ) ) ;
#35204 = B_SPLINE_CURVE_WITH_KNOTS ( 'NONE', 3,
 ( #8601, #5301, #33711, #27749 ),
 .UNSPECIFIED., .F., .F.,
 ( 4, 4 ),
 ( 2.168404344971008868E-19, 0.0005504881370414333418 ),
 .UNSPECIFIED. ) ;
#35205 = CARTESIAN_POINT ( 'NONE',  ( 0.2084121485138739627, -1.634114042384106957, -0.6610165342446623349 ) ) ;
#35206 = COORDINATED_UNIVERSAL_TIME_OFFSET ( 0, 0, .AHEAD. ) ;
#35207 = DIRECTION ( 'NONE',  ( -3.557093741750344791E-15, 0.1725921171157282497, 0.9849933812516257214 ) ) ;
#35208 = CARTESIAN_POINT ( 'NONE',  ( 0.4259076111796487041, -1.664108905841751085, -0.5318766032425232826 ) ) ;
#35209 = CARTESIAN_POINT ( 'NONE',  ( -0.03478489236951871899, 0.5086709597375717040, 0.08927530733454300260 ) ) ;
#35210 = CONICAL_SURFACE ( 'NONE', #21424, 0.03999999999999930000, 1.047197551196598742 ) ;
#35211 = CIRCLE ( 'NONE', #7617, 0.5302738246768095021 ) ;
#35212 = CARTESIAN_POINT ( 'NONE',  ( 0.3650110843922287907, -1.763165835160773076, -0.5889551152805394540 ) ) ;
#35213 = FACE_OUTER_BOUND ( 'NONE', #16302, .T. ) ;
#35214 = ORIENTED_EDGE ( 'NONE', *, *, #500, .F. ) ;
#35215 = DIRECTION ( 'NONE',  ( -1.355854680848614260E-31, 3.330669073875470114E-16, 1.000000000000000000 ) ) ;
#35216 = LOCAL_TIME ( 0, 53, 7.000000000000000000, #9887 ) ;
#35217 = CARTESIAN_POINT ( 'NONE',  ( 0.2652262113535000521, -1.687579907045415828, 0.5753159517177408588 ) ) ;
#35218 = CARTESIAN_POINT ( 'NONE',  ( 0.5956431972771878414, -1.485373576684963171, 0.6181930061425162659 ) ) ;
#35220 = ORIENTED_EDGE ( 'NONE', *, *, #26487, .F. ) ;
#35219 = CARTESIAN_POINT ( 'NONE',  ( 0.000000000000000000, 0.7171888913565960255, -0.2950238883388468514 ) ) ;
#35221 = AXIS2_PLACEMENT_3D ( 'NONE', #23216, #14137, #36344 ) ;
#35223 = ORIENTED_EDGE ( 'NONE', *, *, #37116, .F. ) ;
#35222 = VERTEX_POINT ( 'NONE', #12335 ) ;
#35224 = DIRECTION ( 'NONE',  ( 1.000000000000000000, 0.000000000000000000, 0.000000000000000000 ) ) ;
#35225 = EDGE_LOOP ( 'NONE', ( #34554, #40470, #35369, #5836 ) ) ;
#35226 = ORIENTED_EDGE ( 'NONE', *, *, #40559, .T. ) ;
#35227 = DIRECTION ( 'NONE',  ( 1.000000000000000000, -0.000000000000000000, -0.000000000000000000 ) ) ;
#35228 = CARTESIAN_POINT ( 'NONE',  ( 0.6186988268989424000, -1.622094119273066681, -0.5291206216937438533 ) ) ;
#35229 = SECURITY_CLASSIFICATION_LEVEL ( 'unclassified' ) ;
#35230 = DIRECTION ( 'NONE',  ( -0.4999551463232372317, 0.8660512985181135770, -0.000000000000000000 ) ) ;
#35231 = ORIENTED_EDGE ( 'NONE', *, *, #22268, .T. ) ;
#35232 = CARTESIAN_POINT ( 'NONE',  ( 0.09535391716454494349, -0.8218467293612060631, 0.3072227578265157022 ) ) ;
#35233 = CARTESIAN_POINT ( 'NONE',  ( 0.08990550160137456004, -0.5646315916194289963, 0.1465534274451210095 ) ) ;
#35234 = CARTESIAN_POINT ( 'NONE',  ( 0.5394272294032712578, -1.519093360441811313, 0.5788999028638697197 ) ) ;
#35235 = ORIENTED_EDGE ( 'NONE', *, *, #27386, .F. ) ;
#35236 = CARTESIAN_POINT ( 'NONE',  ( 0.6278493015850613590, -1.616811722123548956, -0.5276078387414424586 ) ) ;
#35237 = CARTESIAN_POINT ( 'NONE',  ( -0.1574073192761877849, 0.4884966930313972555, 0.1147307106484478645 ) ) ;
#35238 = CARTESIAN_POINT ( 'NONE',  ( -0.05562150110511286660, 0.02029635476683722128, 0.4604536315446554617 ) ) ;
#35239 = CARTESIAN_POINT ( 'NONE',  ( 0.3255272214173159928, -1.756778541186221121, 0.5750899042416465212 ) ) ;
#35240 = CARTESIAN_POINT ( 'NONE',  ( 0.6986210655803636316, -1.438860270996676904, 0.5699262351845304497 ) ) ;
#35241 = AXIS2_PLACEMENT_3D ( 'NONE', #31020, #24869, #2641 ) ;
#35242 = CARTESIAN_POINT ( 'NONE',  ( 0.5203574591657224024, -1.609584782789360125, -0.5401600205605632254 ) ) ;
#35243 = CARTESIAN_POINT ( 'NONE',  ( 0.6094178491768812433, -1.479016531803970746, 0.5810952581285231400 ) ) ;
#35244 = CARTESIAN_POINT ( 'NONE',  ( -4.800059970049352646E-06, -0.7803577571415442060, -0.09821680784411590537 ) ) ;
#35245 = ORGANIZATION ( 'NAUO-ORG6', 'UNSPECIFIED', 'UNSPECIFIED' ) ;
#35246 = CARTESIAN_POINT ( 'NONE',  ( 0.3206535937437295369, -1.182295409031864697, 0.3157417262808777658 ) ) ;
#35247 = CARTESIAN_POINT ( 'NONE',  ( 0.03868649100028236087, -0.4417196792138927131, -0.1788567627196029908 ) ) ;
#35248 = CIRCLE ( 'NONE', #8312, 0.4614999999999880864 ) ;
#35249 = CARTESIAN_POINT ( 'NONE',  ( 1.365923996832131609E-16, -0.9481888444201347355, 0.09803024984676507458 ) ) ;
#35250 = CARTESIAN_POINT ( 'NONE',  ( 0.5089221226418110255, -1.111225213825750568, 0.6024461477417591970 ) ) ;
#35251 = APPROVAL_DATE_TIME ( #10359, #33040 ) ;
#35252 = CARTESIAN_POINT ( 'NONE',  ( 0.000000000000000000, 0.08637707520836798714, 0.000000000000000000 ) ) ;
#35253 = CARTESIAN_POINT ( 'NONE',  ( -0.04154009738085516490, 0.4523583096281902916, -0.1287716261385808969 ) ) ;
#35254 = CARTESIAN_POINT ( 'NONE',  ( -0.04574984450155272081, -0.06505050184192864848, 0.4827809015761243550 ) ) ;
#35255 = ORIENTED_EDGE ( 'NONE', *, *, #14285, .T. ) ;
#35256 = CARTESIAN_POINT ( 'NONE',  ( -0.3000000000000000999, -1.990692974992658737, -0.4647843861454829528 ) ) ;
#35257 = DIRECTION ( 'NONE',  ( -1.000000000000000000, -0.000000000000000000, -0.000000000000000000 ) ) ;
#35258 = CARTESIAN_POINT ( 'NONE',  ( 0.08603282679394133603, -0.7798095055049161228, 0.06400130418535010524 ) ) ;
#35259 = ORIENTED_EDGE ( 'NONE', *, *, #28657, .F. ) ;
#35260 = AXIS2_PLACEMENT_3D ( 'NONE', #24142, #39748, #36663 ) ;
#35261 = CARTESIAN_POINT ( 'NONE',  ( -0.1873388932668324236, 0.5325605939836577374, 0.09999999999999975575 ) ) ;
#35262 = CARTESIAN_POINT ( 'NONE',  ( 0.6508285628959425972, -1.351727978844563749, 0.7336055660202295270 ) ) ;
#35264 = VERTEX_POINT ( 'NONE', #18497 ) ;
#35263 = VERTEX_POINT ( 'NONE', #34128 ) ;
#35265 = LINE ( 'NONE', #28881, #17873 ) ;
#35266 = ORIENTED_EDGE ( 'NONE', *, *, #23306, .F. ) ;
#35267 = DIRECTION ( 'NONE',  ( 0.000000000000000000, -3.330669073875470114E-16, -1.000000000000000000 ) ) ;
#35268 = LOCAL_TIME ( 0, 53, 7.000000000000000000, #38701 ) ;
#35269 = DIRECTION ( 'NONE',  ( 0.000000000000000000, 0.000000000000000000, -1.000000000000000000 ) ) ;
#35270 = FACE_OUTER_BOUND ( 'NONE', #33782, .T. ) ;
#35271 = ORIENTED_EDGE ( 'NONE', *, *, #22661, .F. ) ;
#35272 = CARTESIAN_POINT ( 'NONE',  ( 0.1376369211866255993, -0.6843090735930908997, 0.7406414737086894906 ) ) ;
#35273 = VECTOR ( 'NONE', #13710, 39.37007874015748143 ) ;
#35274 = CARTESIAN_POINT ( 'NONE',  ( 0.09128336968152271635, -0.5703653419453503792, 0.2228016259242908137 ) ) ;
#35275 = CARTESIAN_POINT ( 'NONE',  ( 0.01633901792732134900, -0.5702388794319304122, 0.5330440696850335947 ) ) ;
#35276 = CARTESIAN_POINT ( 'NONE',  ( 0.09962249923029198317, -0.6318392586327593596, 0.3999921429806476691 ) ) ;
#35278 = CARTESIAN_POINT ( 'NONE',  ( -0.1208133668958378537, -0.5051731972035429230, 0.3159170889047719366 ) ) ;
#35277 = CARTESIAN_POINT ( 'NONE',  ( 0.5462348416196847189, -1.594646255991501338, -0.4868944820179722521 ) ) ;
#35279 = CARTESIAN_POINT ( 'NONE',  ( 0.1519119642568272921, -0.9326923694292597045, 0.3322815801383296463 ) ) ;
#35280 = ORIENTED_EDGE ( 'NONE', *, *, #22736, .F. ) ;
#35281 = APPROVAL ( #12692, 'UNSPECIFIED' ) ;
#35282 = ORIENTED_EDGE ( 'NONE', *, *, #25741, .F. ) ;
#35283 = CARTESIAN_POINT ( 'NONE',  ( 0.3177856290042974652, -1.645584934368151009, 0.5182417262812344383 ) ) ;
#35284 = CARTESIAN_POINT ( 'NONE',  ( 0.1153471832944766712, -0.4465912132367801934, 0.1463508116155961547 ) ) ;
#35285 = CARTESIAN_POINT ( 'NONE',  ( -0.05138886601527986597, 0.2591656398409026285, -0.3946081992295794039 ) ) ;
#35286 = FACE_OUTER_BOUND ( 'NONE', #902, .T. ) ;
#35287 = DIRECTION ( 'NONE',  ( 1.000000000000000000, -0.000000000000000000, -0.000000000000000000 ) ) ;
#35288 = CIRCLE ( 'NONE', #26757, 0.03000000000000029379 ) ;
#35289 = EDGE_LOOP ( 'NONE', ( #27014, #30762, #1537, #37940 ) ) ;
#35290 = CARTESIAN_POINT ( 'NONE',  ( 0.5893014856854912331, -1.253657609334210665, 0.7958531859040811618 ) ) ;
#35291 = B_SPLINE_SURFACE_WITH_KNOTS ( 'NONE', 3, 1, ( 
 ( #353, #31979 ),
 ( #15726, #28275 ),
 ( #9562, #6655 ),
 ( #34656, #561 ) ),
 .UNSPECIFIED., .F., .F., .F.,
 ( 4, 4 ),
 ( 2, 2 ),
 ( 0.000000000000000000, 1.000000000000000000 ),
 ( 0.000000000000000000, 1.000000000000000000 ),
 .UNSPECIFIED. ) ;
#35292 = EDGE_CURVE ( 'NONE', #36006, #15118, #31194, .T. ) ;
#35293 = CARTESIAN_POINT ( 'NONE',  ( -0.2300000000000000655, 0.5182417262804733804, 0.3749999999999999445 ) ) ;
#35294 = DIRECTION ( 'NONE',  ( -3.389636702121535101E-31, -0.4685245517976796559, 0.8834504764630461970 ) ) ;
#35295 = CARTESIAN_POINT ( 'NONE',  ( 0.04308611741967136727, 0.4845711164928941939, -0.09763251765259810255 ) ) ;
#35296 = CARTESIAN_POINT ( 'NONE',  ( 0.5116966680315802041, -1.675313993414271341, -0.6001126952423705418 ) ) ;
#35297 = CARTESIAN_POINT ( 'NONE',  ( 0.2282131427976650528, -0.9177001319490483144, 0.6643802175654811570 ) ) ;
#35298 = CARTESIAN_POINT ( 'NONE',  ( 0.02235124290213176892, -0.07000983313419581466, 0.5077112423787075723 ) ) ;
#35299 = EDGE_CURVE ( 'NONE', #13132, #12586, #7645, .T. ) ;
#35300 = CARTESIAN_POINT ( 'NONE',  ( 0.6792220396283762396, -1.521116734023811201, 0.4455427699610711723 ) ) ;
#35301 = EDGE_CURVE ( 'NONE', #25941, #23695, #37617, .T. ) ;
#35302 = VERTEX_POINT ( 'NONE', #33721 ) ;
#35303 = DIRECTION ( 'NONE',  ( -1.000000000000000000, -0.000000000000000000, -0.000000000000000000 ) ) ;
#35304 = CARTESIAN_POINT ( 'NONE',  ( 0.2103800470826229507, -0.8725428098432390644, 0.6529641895999598322 ) ) ;
#35305 = EDGE_CURVE ( 'NONE', #9001, #7421, #17878, .T. ) ;
#35306 = CARTESIAN_POINT ( 'NONE',  ( -0.02000000000000000042, -2.183180860297908144, -0.4937760292030871079 ) ) ;
#35307 = EDGE_CURVE ( 'NONE', #9331, #6967, #20633, .T. ) ;
#35308 = DIRECTION ( 'NONE',  ( -1.000000000000000000, -0.000000000000000000, -0.000000000000000000 ) ) ;
#35309 = EDGE_CURVE ( 'NONE', #17498, #34509, #2916, .T. ) ;
#35310 = CARTESIAN_POINT ( 'NONE',  ( 0.09606123864389597145, -0.9124172847158124044, 0.5866022920368346716 ) ) ;
#35311 = ORIENTED_EDGE ( 'NONE', *, *, #6180, .T. ) ;
#35312 = CARTESIAN_POINT ( 'NONE',  ( -0.01895494625228242788, -0.3623053290766977130, -0.3730957266516564674 ) ) ;
#35313 = CARTESIAN_POINT ( 'NONE',  ( 0.01548846960707524721, 0.000000000000000000, 0.000000000000000000 ) ) ;
#35314 = DIRECTION ( 'NONE',  ( 0.000000000000000000, 3.330669073875469621E-16, 1.000000000000000000 ) ) ;
#35315 = CARTESIAN_POINT ( 'NONE',  ( 0.6547994310234585003, -1.589707258511555255, -0.5155029497116575543 ) ) ;
#35316 = CARTESIAN_POINT ( 'NONE',  ( 0.4602903487706154206, -1.228384066590711754, 0.6755160344941316675 ) ) ;
#35318 = DIRECTION ( 'NONE',  ( 1.000000000000000000, 2.276539994720212446E-15, 0.000000000000000000 ) ) ;
#35317 = CARTESIAN_POINT ( 'NONE',  ( -0.05464101615137786222, -2.198867511061768809, -0.9423512173156428640 ) ) ;
#35319 = CARTESIAN_POINT ( 'NONE',  ( 0.4928237909781065240, -1.082648202709539431, 0.5731206881285608734 ) ) ;
#35320 = ORIENTED_EDGE ( 'NONE', *, *, #17335, .T. ) ;
#35321 = DATE_AND_TIME ( #25877, #13509 ) ;
#35322 = DIRECTION ( 'NONE',  ( -1.387778780781449620E-15, -6.590151126658398618E-16, -1.000000000000000000 ) ) ;
#35323 = VERTEX_POINT ( 'NONE', #30653 ) ;
#35324 =( BOUNDED_SURFACE ( )  B_SPLINE_SURFACE ( 3, 2, ( 
 ( #26720, #2227, #4474 ),
 ( #23632, #11071, #36150 ),
 ( #13937, #30188, #26507 ),
 ( #33467, #33275, #1423 ) ),
 .UNSPECIFIED., .F., .F., .F. ) 
 B_SPLINE_SURFACE_WITH_KNOTS ( ( 4, 4 ),
 ( 3, 3 ),
 ( 0.003771772523746863212, 0.004062699796700002322 ),
 ( 0.000000000000000000, 1.000000000000000000 ),
 .UNSPECIFIED. ) 
 GEOMETRIC_REPRESENTATION_ITEM ( )  RATIONAL_B_SPLINE_SURFACE ( (
 ( 1.000000000000000000, 0.7270749630179166312, 1.000000000000000000),
 ( 1.000000000000000000, 0.7198896738069492374, 1.000000000000000000),
 ( 1.000000000000000000, 0.7126463349551879212, 1.000000000000000000),
 ( 1.000000000000000000, 0.7054447009685870240, 1.000000000000000000) ) ) 
 REPRESENTATION_ITEM ( '' )  SURFACE ( )  );
#35325 = CARTESIAN_POINT ( 'NONE',  ( 0.07156345257519909631, -0.6773993882840948499, 0.4940002351035037709 ) ) ;
#35326 = EDGE_CURVE ( 'NONE', #16165, #5083, #2252, .T. ) ;
#35328 = CARTESIAN_POINT ( 'NONE',  ( 0.2002482725081971004, -0.6266219077336198096, 0.3288090134007002341 ) ) ;
#35327 = CARTESIAN_POINT ( 'NONE',  ( 0.08705834347432826748, -0.7253769890809593779, 0.006460193196229412418 ) ) ;
#35329 = CARTESIAN_POINT ( 'NONE',  ( 0.06772995496177347530, -0.6134157779729459969, 0.01766292184562558848 ) ) ;
#35330 = APPLIED_PERSON_AND_ORGANIZATION_ASSIGNMENT ( #37926, #25176, ( #14383 ) ) ;
#35331 = ORIENTED_EDGE ( 'NONE', *, *, #5475, .F. ) ;
#35332 = CARTESIAN_POINT ( 'NONE',  ( -0.02000000000000000042, -1.737515812098395118, -0.8661170628529262228 ) ) ;
#35333 = CARTESIAN_POINT ( 'NONE',  ( 0.4949533726178510507, -1.379071206832592544, 0.8062209685769742284 ) ) ;
#35334 = VECTOR ( 'NONE', #17099, 39.37007874015748854 ) ;
#35335 = EDGE_LOOP ( 'NONE', ( #6278, #29965, #13646, #39779 ) ) ;
#35336 = CARTESIAN_POINT ( 'NONE',  ( 0.07115698274084111818, -1.324302356227759825, 0.5002514903164775317 ) ) ;
#35337 = CARTESIAN_POINT ( 'NONE',  ( 0.1499999999999994671, 0.5230810839623362130, 0.1699593469062180839 ) ) ;
#35338 = DIRECTION ( 'NONE',  ( -8.881784197001245421E-16, 2.361472542561082612E-16, -1.000000000000000000 ) ) ;
#35339 = DIRECTION ( 'NONE',  ( 1.000000000000000000, 0.000000000000000000, 0.000000000000000000 ) ) ;
#35340 = FACE_OUTER_BOUND ( 'NONE', #21870, .T. ) ;
#35341 = CARTESIAN_POINT ( 'NONE',  ( 0.08752988513861870157, -0.6847329015552422460, 0.1457151237251784470 ) ) ;
#35342 = DIRECTION ( 'NONE',  ( -0.01265474379914244447, -0.8659329421511298142, 0.4999999971568662160 ) ) ;
#35343 = CARTESIAN_POINT ( 'NONE',  ( 0.3908699498952687423, -1.745013346922102748, -0.7175586304900263279 ) ) ;
#35344 = FACE_OUTER_BOUND ( 'NONE', #12485, .T. ) ;
#35345 = DIRECTION ( 'NONE',  ( 0.9948684839163943749, 2.731847993664264244E-14, 0.1011765768836579149 ) ) ;
#35346 = PERSON_AND_ORGANIZATION ( #28500, #32463 ) ;
#35347 = CARTESIAN_POINT ( 'NONE',  ( -0.02000000000000000042, -1.584107902207569696, 0.1773406241487738566 ) ) ;
#35348 = CARTESIAN_POINT ( 'NONE',  ( 0.1717957286698658936, -1.383210011275196827, 0.4993402293719408913 ) ) ;
#35349 = CARTESIAN_POINT ( 'NONE',  ( 0.1849152241263185281, -0.7983094181796221989, 0.01806537668523729850 ) ) ;
#35350 = CARTESIAN_POINT ( 'NONE',  ( 0.2590198564899700573, -1.679471795743312290, 0.4182417262808776348 ) ) ;
#35351 = CARTESIAN_POINT ( 'NONE',  ( 0.2617320194804602096, -1.680740016843867979, 0.5479263650791303952 ) ) ;
#35352 = PERSON ( 'NAUO-PER5', 'UNSPECIFIED', 'UNSPECIFIED', ('UNSPECIFIED'), ('UNSPECIFIED'), ('UNSPECIFIED') ) ;
#35353 = EDGE_CURVE ( 'NONE', #7904, #7711, #12524, .T. ) ;
#35354 = CARTESIAN_POINT ( 'NONE',  ( -8.537024980200822558E-17, -0.6872203660140403514, 0.1122922589469583232 ) ) ;
#35355 = CARTESIAN_POINT ( 'NONE',  ( 0.5875654382963820810, -1.532386235059486346, -0.4097741950298078306 ) ) ;
#35356 = EDGE_CURVE ( 'NONE', #26267, #38006, #16686, .T. ) ;
#35357 = CARTESIAN_POINT ( 'NONE',  ( -0.05464101615137770263, -2.183180860297908144, -0.4937760292030871079 ) ) ;
#35358 = CARTESIAN_POINT ( 'NONE',  ( 0.1991480113865206902, -2.054949600705703983, -0.6841806413415666421 ) ) ;
#35359 = CARTESIAN_POINT ( 'NONE',  ( 0.2059260937967708482, -1.283047057827471082, -0.2869367607460444614 ) ) ;
#35360 = ADVANCED_FACE ( 'NONE', ( #6350 ), #9841, .F. ) ;
#35361 = EDGE_LOOP ( 'NONE', ( #8434, #27766, #6356, #31737, #737 ) ) ;
#35362 = EDGE_LOOP ( 'NONE', ( #28980, #10002, #26371, #2884 ) ) ;
#35363 = CARTESIAN_POINT ( 'NONE',  ( 0.02953079040095687308, -0.3810518745593889922, -0.3687679460475752902 ) ) ;
#35364 = EDGE_LOOP ( 'NONE', ( #710, #26455 ) ) ;
#35365 = CARTESIAN_POINT ( 'NONE',  ( -0.01895884884825279129, -0.07380796352548195383, 0.5147901372834200462 ) ) ;
#35366 = DIRECTION ( 'NONE',  ( -1.000000000000000000, -0.000000000000000000, -0.000000000000000000 ) ) ;
#35367 = CARTESIAN_POINT ( 'NONE',  ( 0.3644834194571767161, -1.092200917885892686, 0.7884070574448115432 ) ) ;
#35369 = ORIENTED_EDGE ( 'NONE', *, *, #38667, .F. ) ;
#35368 = CYLINDRICAL_SURFACE ( 'NONE', #25222, 0.5400000000000007017 ) ;
#35370 = CARTESIAN_POINT ( 'NONE',  ( 0.5484966004669556972, -1.177603726185705080, 0.6257892858931851654 ) ) ;
#35371 = CARTESIAN_POINT ( 'NONE',  ( 0.05082303569918648206, 0.4330427793496112732, -0.1918498709088735932 ) ) ;
#35372 = VERTEX_POINT ( 'NONE', #15367 ) ;
#35373 = CARTESIAN_POINT ( 'NONE',  ( 0.6009178235190556494, -1.482100521748198396, -0.6278260014982935955 ) ) ;
#35374 = ORIENTED_EDGE ( 'NONE', *, *, #11536, .T. ) ;
#35375 = CARTESIAN_POINT ( 'NONE',  ( 0.3270948354918082890, -1.639212714906252311, 0.5750488052645271742 ) ) ;
#35376 = ADVANCED_FACE ( 'NONE', ( #39642 ), #29163, .F. ) ;
#35378 = CYLINDRICAL_SURFACE ( 'NONE', #2509, 0.04330708661417343591 ) ;
#35377 = DIRECTION ( 'NONE',  ( 1.000000000000000000, -0.000000000000000000, -0.000000000000000000 ) ) ;
#35379 = DIRECTION ( 'NONE',  ( 0.4999551463232372317, -0.8660512985181133550, 0.000000000000000000 ) ) ;
#35380 = CARTESIAN_POINT ( 'NONE',  ( 0.09698018536738627071, -1.424165361423572751, -0.3353914638860537312 ) ) ;
#35381 = EDGE_LOOP ( 'NONE', ( #8144, #9750, #10576, #12848, #32138, #36929, #14493, #264, #2478, #24302, #17550 ) ) ;
#35382 = CARTESIAN_POINT ( 'NONE',  ( 0.5446687329359086727, -1.168273840204911540, 0.5856983068966360451 ) ) ;
#35383 = CARTESIAN_POINT ( 'NONE',  ( 0.1266587039438421824, -0.9372301308308913503, 0.3362830365086449391 ) ) ;
#35384 = DIRECTION ( 'NONE',  ( 0.000000000000000000, 0.000000000000000000, -1.000000000000000000 ) ) ;
#35385 = DIRECTION ( 'NONE',  ( 0.4999551463232371762, -0.8660512985181134660, 0.000000000000000000 ) ) ;
#35386 = CARTESIAN_POINT ( 'NONE',  ( 0.1888634695993094692, -0.9417634414638629270, 0.6531452432017001986 ) ) ;
#35387 = CARTESIAN_POINT ( 'NONE',  ( 0.02211643768509126765, -0.6637935133132942811, 0.4930904770729322983 ) ) ;
#35388 = CARTESIAN_POINT ( 'NONE',  ( 0.4820730268389710194, -1.120100422993975275, 0.5182417262812748504 ) ) ;
#35389 = CARTESIAN_POINT ( 'NONE',  ( -0.1696286242763865582, 0.4941126639394797793, 0.3207424310465874506 ) ) ;
#35390 = CARTESIAN_POINT ( 'NONE',  ( 0.03113248654051816583, 0.5878163732725504298, -0.1704268771689479434 ) ) ;
#35391 = CYLINDRICAL_SURFACE ( 'NONE', #10651, 0.2149999999999999967 ) ;
#35392 = PERSON_AND_ORGANIZATION ( #28500, #32463 ) ;
#35393 = B_SPLINE_CURVE_WITH_KNOTS ( 'NONE', 3,
 ( #39752, #32760, #14252, #10980, #17340, #29897, #11165, #20850, #1922, #30281, #33375, #9088 ),
 .UNSPECIFIED., .F., .F.,
 ( 4, 2, 2, 2, 2, 4 ),
 ( 0.001091185218850428823, 0.001968393139851580542, 0.002845601060852732261, 0.003722808981853884414, 0.004161412942354461575, 0.004600016902855039169 ),
 .UNSPECIFIED. ) ;
#35394 = CARTESIAN_POINT ( 'NONE',  ( 0.07499999999999933109, 0.2900000000000004796, -5.122214988120493288E-16 ) ) ;
#35395 = CARTESIAN_POINT ( 'NONE',  ( 0.4850543146008196027, -1.678681405600182641, -0.6440782542835996605 ) ) ;
#35396 = CARTESIAN_POINT ( 'NONE',  ( 0.2127756690299808795, -1.279092926711003830, -0.7170389573829240026 ) ) ;
#35397 = PRODUCT ( 'Lower Pivot Bracket', 'Lower Pivot Bracket', '', ( #34592 ) ) ;
#35398 = CARTESIAN_POINT ( 'NONE',  ( 0.2011892967074957184, -1.251141541415955682, -0.3144976166544468099 ) ) ;
#35399 = CARTESIAN_POINT ( 'NONE',  ( 0.1784765141246957565, -1.731228076122506954, -0.6515962173610828634 ) ) ;
#35400 = EDGE_CURVE ( 'NONE', #31635, #33002, #38532, .T. ) ;
#35401 = CARTESIAN_POINT ( 'NONE',  ( 0.3109023401880776083, -1.751637589031094011, 0.6786626549772374339 ) ) ;
#35402 = CARTESIAN_POINT ( 'NONE',  ( 0.6906859043523344566, -1.496443130473642080, 0.4682586448533338497 ) ) ;
#35403 = ORIENTED_EDGE ( 'NONE', *, *, #35353, .T. ) ;
#35404 = CARTESIAN_POINT ( 'NONE',  ( 0.4519383542666973730, -1.131712119964726648, 0.4502564825975859386 ) ) ;
#35405 = ORIENTED_EDGE ( 'NONE', *, *, #18503, .F. ) ;
#35406 = EDGE_CURVE ( 'NONE', #33948, #1932, #40464, .T. ) ;
#35407 = CARTESIAN_POINT ( 'NONE',  ( 0.2565234391735137232, -1.677641732679920450, 0.5263822859174334123 ) ) ;
#35408 = CARTESIAN_POINT ( 'NONE',  ( 0.3114613613881818677, -1.004621970292722377, 0.7614557701602212569 ) ) ;
#35410 = ORIENTED_EDGE ( 'NONE', *, *, #23986, .T. ) ;
#35409 = CARTESIAN_POINT ( 'NONE',  ( -0.01548846960707517956, -0.3880410510314710182, 0.3755318131855027719 ) ) ;
#35412 = VERTEX_POINT ( 'NONE', #6086 ) ;
#35411 = ORIENTED_EDGE ( 'NONE', *, *, #39666, .F. ) ;
#35413 = CYLINDRICAL_SURFACE ( 'NONE', #29065, 0.1000000000000000194 ) ;
#35414 = ORIENTED_EDGE ( 'NONE', *, *, #10248, .F. ) ;
#35415 = DIRECTION ( 'NONE',  ( 0.000000000000000000, 0.000000000000000000, -1.000000000000000000 ) ) ;
#35416 = CARTESIAN_POINT ( 'NONE',  ( 0.6180462672592140771, -1.622470829695115135, -0.5097172539320682372 ) ) ;
#35417 = EDGE_CURVE ( 'NONE', #12111, #356, #13425, .T. ) ;
#35418 = ITEM_DEFINED_TRANSFORMATION ( 'NONE', 'NONE', #12780,  #27819 ) ;
#35419 = CYLINDRICAL_SURFACE ( 'NONE', #19850, 0.2500000000000000000 ) ;
#35420 = VERTEX_POINT ( 'NONE', #3034 ) ;
#35421 = ADVANCED_FACE ( 'NONE', ( #15578 ), #36394, .F. ) ;
#35422 = CARTESIAN_POINT ( 'NONE',  ( 0.2227485520779646233, -0.9426598342782120943, 0.6424711532909392897 ) ) ;
#35423 = CARTESIAN_POINT ( 'NONE',  ( 0.4058447956437031268, -1.613147253033901940, -0.3639822749465717600 ) ) ;
#35424 = CARTESIAN_POINT ( 'NONE',  ( 0.5173655358750550715, -1.478930200014486829, 0.7454170918323320683 ) ) ;
#35425 = CARTESIAN_POINT ( 'NONE',  ( 0.1915715022251594790, -0.5493874118981464383, 0.2939312971703439414 ) ) ;
#35426 = DIRECTION ( 'NONE',  ( 1.188678714063518227E-15, -1.000000000000000000, -3.263080277421930985E-16 ) ) ;
#35427 = CARTESIAN_POINT ( 'NONE',  ( -0.2399999999999999079, -2.831259187443150971, -0.3041590760046470887 ) ) ;
#35428 = CARTESIAN_POINT ( 'NONE',  ( -19685.03937007874265, 285.9652880572280083, -1.951739244310253252 ) ) ;
#35429 = CARTESIAN_POINT ( 'NONE',  ( 0.3849858519270614177, -1.672779373200289132, -0.3639115729092421425 ) ) ;
#35430 = DIRECTION ( 'NONE',  ( -0.9996235034872141823, 0.000000000000000000, -0.02743813543131554469 ) ) ;
#35431 = CARTESIAN_POINT ( 'NONE',  ( 0.6090682804592260080, -1.479034850722692696, 0.5736300833207230720 ) ) ;
#35432 = CARTESIAN_POINT ( 'NONE',  ( -1.494856848218599248E-05, -0.8613933088276938266, -0.04939037072607115747 ) ) ;
#35433 = PLANE ( 'NONE',  #15509 ) ;
#35434 = CARTESIAN_POINT ( 'NONE',  ( 0.4564594823903532217, -1.083519075567892953, -0.6177465903673754477 ) ) ;
#35435 = CARTESIAN_POINT ( 'NONE',  ( 0.1057086693319095883, -1.337907155632660716, 0.7376750060448485913 ) ) ;
#35436 = CARTESIAN_POINT ( 'NONE',  ( 0.1851443459949622949, -0.7907988577364570837, 0.1906562862421710969 ) ) ;
#35437 = PERSON_AND_ORGANIZATION_ROLE ( 'creator' ) ;
#35438 = EDGE_CURVE ( 'NONE', #18610, #11635, #13392, .T. ) ;
#35439 = DIRECTION ( 'NONE',  ( -1.000000000000000000, -0.000000000000000000, -0.000000000000000000 ) ) ;
#35440 = CARTESIAN_POINT ( 'NONE',  ( 0.4904112910084666432, -1.188461936721600720, 0.4182417262808778013 ) ) ;
#35441 = ORIENTED_EDGE ( 'NONE', *, *, #36090, .F. ) ;
#35442 = CARTESIAN_POINT ( 'NONE',  ( -0.07216878364870325802, 0.05141091571461162829, -0.1249999999999999029 ) ) ;
#35443 = CARTESIAN_POINT ( 'NONE',  ( -2.359223927328457648E-16, -0.01499999999999986587, -0.1699999999999995126 ) ) ;
#35444 = LINE ( 'NONE', #7244, #18022 ) ;
#35445 = EDGE_LOOP ( 'NONE', ( #3102, #22044, #36257 ) ) ;
#35446 = DIRECTION ( 'NONE',  ( -0.9378410757839559242, 0.1072489841977647268, 0.3300784330442382841 ) ) ;
#35447 = CARTESIAN_POINT ( 'NONE',  ( 0.1896045607153576118, -0.5049209053381719103, 0.1595777137938904078 ) ) ;
#35449 = ORIENTED_EDGE ( 'NONE', *, *, #14752, .F. ) ;
#35448 = VERTEX_POINT ( 'NONE', #19273 ) ;
#35450 = CARTESIAN_POINT ( 'NONE',  ( -0.2746410161513782033, -2.342996121808762044, -0.6842569225768811991 ) ) ;
#35451 = ORIENTED_EDGE ( 'NONE', *, *, #25654, .T. ) ;
#35452 = CARTESIAN_POINT ( 'NONE',  ( 0.1999999999999789724, -2.107936428766273629, -0.7005084057759867200 ) ) ;
#35453 = CARTESIAN_POINT ( 'NONE',  ( 0.4259076111796464836, -1.664108905841752195, -0.4991292961807995421 ) ) ;
#35454 = CARTESIAN_POINT ( 'NONE',  ( -0.05252049209742535446, 0.4488546425834959441, -0.1362647994370397020 ) ) ;
#35455 = B_SPLINE_CURVE_WITH_KNOTS ( 'NONE', 3,
 ( #17830, #36754, #39854, #11674, #8565, #26717 ),
 .UNSPECIFIED., .F., .F.,
 ( 4, 2, 4 ),
 ( 0.000000000000000000, 0.0007689356304541490605, 0.001537871260908298121 ),
 .UNSPECIFIED. ) ;
#35456 = ORIENTED_EDGE ( 'NONE', *, *, #28012, .F. ) ;
#35457 = CARTESIAN_POINT ( 'NONE',  ( 0.4443883236068807419, -1.706945807527836756, 0.8827363541034584093 ) ) ;
#35458 = CARTESIAN_POINT ( 'NONE',  ( 0.1091475376240157724, -0.6888598723991967709, 0.3909236133807777458 ) ) ;
#35459 = B_SPLINE_CURVE_WITH_KNOTS ( 'NONE', 3,
 ( #27368, #14189, #20979, #36396, #39893, #1862, #35995, #24271, #23478, #7801 ),
 .UNSPECIFIED., .F., .F.,
 ( 4, 2, 2, 2, 4 ),
 ( 7.271605333268061299E-15, 0.0003768098143164838490, 0.0007536196286256961708, 0.001130429442934908438, 0.001507239257244120598 ),
 .UNSPECIFIED. ) ;
#35460 = CARTESIAN_POINT ( 'NONE',  ( 0.003415692958229195764, -0.4932933441065976976, 0.3528940576573719734 ) ) ;
#35461 = CARTESIAN_POINT ( 'NONE',  ( 0.3955718155169024031, -1.346764816040846746, 0.8519979171323052158 ) ) ;
#35463 = CARTESIAN_POINT ( 'NONE',  ( 0.3455335085159372821, -1.741491928912728637, 0.4422736660380222062 ) ) ;
#35462 = CARTESIAN_POINT ( 'NONE',  ( 0.5446426061928973938, -1.595565423594093035, -0.4737885531983786480 ) ) ;
#35464 = CARTESIAN_POINT ( 'NONE',  ( 0.1179759873886401383, -1.125199527543434330, 0.6533949885475268671 ) ) ;
#35465 = VERTEX_POINT ( 'NONE', #31813 ) ;
#35466 = UNCERTAINTY_MEASURE_WITH_UNIT (LENGTH_MEASURE( 1.000000000000000082E-05 ), #11616, 'distance_accuracy_value', 'NONE');
#35467 = DIRECTION ( 'NONE',  ( 1.417484439069006026E-31, -3.885780586188048878E-16, -1.000000000000000000 ) ) ;
#35468 = CARTESIAN_POINT ( 'NONE',  ( 0.1916429764873162911, -0.5530848051578395319, 0.2366777123144251094 ) ) ;
#35469 = CARTESIAN_POINT ( 'NONE',  ( 0.3365215356197720498, -1.138376801642753788, -0.5155029497116575543 ) ) ;
#35470 = DIRECTION ( 'NONE',  ( 0.8660512985181133550, 0.4999551463232372872, 0.000000000000000000 ) ) ;
#35471 = CARTESIAN_POINT ( 'NONE',  ( 0.07551600056043764053, -1.312274329810509066, 0.4837890602591397582 ) ) ;
#35472 = DIRECTION ( 'NONE',  ( -1.000000000000000000, -0.000000000000000000, -0.000000000000000000 ) ) ;
#35473 = CARTESIAN_POINT ( 'NONE',  ( 0.4683780286950792182, -1.066659082333339059, 0.7984748632466120988 ) ) ;
#35474 = CARTESIAN_POINT ( 'NONE',  ( 0.1499999999999993561, 0.2372406987223596164, -0.4850946823762614102 ) ) ;
#35475 = CARTESIAN_POINT ( 'NONE',  ( 0.007696911294830250348, -0.8993530900274140372, 0.5044786313595001070 ) ) ;
#35476 = VECTOR ( 'NONE', #15428, 39.37007874015748143 ) ;
#35477 = CARTESIAN_POINT ( 'NONE',  ( 0.03170874437002939306, 0.4481116538287104878, -0.2027256324086052497 ) ) ;
#35478 = CARTESIAN_POINT ( 'NONE',  ( 0.5654596793231598806, -1.618818539163461301, 0.5682417262808788783 ) ) ;
#35479 = ORIENTED_EDGE ( 'NONE', *, *, #12011, .F. ) ;
#35480 = CARTESIAN_POINT ( 'NONE',  ( 0.2949679976356796018, -0.9947731076855342858, 0.7382632246787314001 ) ) ;
#35481 = CARTESIAN_POINT ( 'NONE',  ( 0.04229956186878614660, -0.008769846780145499829, 0.4686106502047106548 ) ) ;
#35482 = FACE_OUTER_BOUND ( 'NONE', #13152, .T. ) ;
#35483 = VECTOR ( 'NONE', #39703, 39.37007874015748854 ) ;
#35484 = ORIENTED_EDGE ( 'NONE', *, *, #2355, .F. ) ;
#35485 = CARTESIAN_POINT ( 'NONE',  ( -0.2399999999999999079, -3.647187793141847045, -0.4766722536777797115 ) ) ;
#35486 = DIRECTION ( 'NONE',  ( 0.000000000000000000, 0.000000000000000000, -1.000000000000000000 ) ) ;
#35487 = CARTESIAN_POINT ( 'NONE',  ( 0.3564725003429615735, -1.740492809915490824, -0.4610359798238701234 ) ) ;
#35488 = CARTESIAN_POINT ( 'NONE',  ( -0.01548846960707545191, -0.5198120922912051745, -0.07362328916749329155 ) ) ;
#35489 = CARTESIAN_POINT ( 'NONE',  ( 0.2275226583839362604, -1.223163572956847966, 0.7306588133906862792 ) ) ;
#35490 = ORIENTED_EDGE ( 'NONE', *, *, #30129, .F. ) ;
#35491 = CARTESIAN_POINT ( 'NONE',  ( -0.02869942827333507931, -0.2420058122830170133, -0.4357544236535315640 ) ) ;
#35492 = CARTESIAN_POINT ( 'NONE',  ( 0.3625960434667531151, -1.762758894398492204, -0.5926935080085831142 ) ) ;
#35493 = CARTESIAN_POINT ( 'NONE',  ( 0.5641559342961582901, -1.318727562814529186, -0.4122610257295771796 ) ) ;
#35494 = CARTESIAN_POINT ( 'NONE',  ( 0.1943568813818912500, -1.255085766440153350, -0.7153666819277929578 ) ) ;
#35495 = CARTESIAN_POINT ( 'NONE',  ( 0.3987602141185838667, -1.146724837527934193, 0.7205486833366475663 ) ) ;
#35497 = CARTESIAN_POINT ( 'NONE',  ( 0.3204139389452054232, -1.755336229099436318, 0.4849083929475442867 ) ) ;
#35496 = DIRECTION ( 'NONE',  ( -1.000000000000000000, -7.857794173099924470E-32, -8.628166150854818811E-32 ) ) ;
#35498 = CARTESIAN_POINT ( 'NONE',  ( 0.5752615338540276735, -1.540169966941223656, -0.5501209398761891523 ) ) ;
#35499 = ORIENTED_EDGE ( 'NONE', *, *, #21048, .T. ) ;
#35500 = COORDINATED_UNIVERSAL_TIME_OFFSET ( 0, 0, .AHEAD. ) ;
#35501 = CARTESIAN_POINT ( 'NONE',  ( -0.2399999999999999079, -4.098813193844367042, -0.6491724279539748954 ) ) ;
#35502 = VERTEX_POINT ( 'NONE', #9384 ) ;
#35503 = CARTESIAN_POINT ( 'NONE',  ( 0.4157477866045977688, -1.588835819673688254, 0.6151641792345675652 ) ) ;
#35505 = CARTESIAN_POINT ( 'NONE',  ( 0.2018805221389261828, -0.6980253832968265071, 0.3378735216469233582 ) ) ;
#35504 = LINE ( 'NONE', #1011, #11213 ) ;
#35506 = LINE ( 'NONE', #36323, #28994 ) ;
#35507 = ORIENTED_EDGE ( 'NONE', *, *, #21825, .F. ) ;
#35508 = TOROIDAL_SURFACE ( 'NONE', #26340, 1.986674066779348768, 0.01499999999999999944 ) ;
#35509 = EDGE_LOOP ( 'NONE', ( #32258, #37428, #14398, #29188 ) ) ;
#35510 = FACE_OUTER_BOUND ( 'NONE', #1543, .T. ) ;
#35511 = ADVANCED_FACE ( 'NONE', ( #34488 ), #29547, .F. ) ;
#35512 = EDGE_CURVE ( 'NONE', #6859, #31663, #9617, .T. ) ;
#35513 = CARTESIAN_POINT ( 'NONE',  ( 0.1561817513097121801, -0.7009449418526539910, 0.4986987260078958317 ) ) ;
#35514 = ORIENTED_EDGE ( 'NONE', *, *, #31346, .F. ) ;
#35515 = CARTESIAN_POINT ( 'NONE',  ( 0.4845663548694630895, -1.649128766679687885, -0.4001533324282806059 ) ) ;
#35516 = CARTESIAN_POINT ( 'NONE',  ( 0.01896931156526852555, -0.5123785568735317320, 0.08888416637129550879 ) ) ;
#35517 = AXIS2_PLACEMENT_3D ( 'NONE', #2022, #11273, #23840 ) ;
#35518 = CARTESIAN_POINT ( 'NONE',  ( 0.1853469541905378160, -0.8336531673994818092, 0.1643568276252908300 ) ) ;
#35519 = ORIENTED_EDGE ( 'NONE', *, *, #12663, .F. ) ;
#35520 = DIRECTION ( 'NONE',  ( 1.000000000000000000, 0.000000000000000000, 7.515112548955565209E-16 ) ) ;
#35522 = EDGE_CURVE ( 'NONE', #26696, #33794, #3215, .T. ) ;
#35521 = CIRCLE ( 'NONE', #9890, 0.05000000000000000971 ) ;
#35523 = CARTESIAN_POINT ( 'NONE',  ( 0.4310150799785918418, -1.695525730796878294, 0.6145840607228283403 ) ) ;
#35524 = CARTESIAN_POINT ( 'NONE',  ( 0.3926032618789480622, -1.756026311479843782, -0.5284552501753819742 ) ) ;
#35525 = EDGE_CURVE ( 'NONE', #3174, #17938, #34605, .T. ) ;
#35526 = FACE_OUTER_BOUND ( 'NONE', #12793, .T. ) ;
#35527 = CARTESIAN_POINT ( 'NONE',  ( 0.2219270030867450672, -1.605284576339639058, -0.6971167956771215923 ) ) ;
#35528 = CARTESIAN_POINT ( 'NONE',  ( 0.3827394763927673971, -1.608088298394132254, 0.5182417262812428760 ) ) ;
#35529 = CARTESIAN_POINT ( 'NONE',  ( 0.08016251834805442067, -1.309203902574839207, 0.5631135398343307674 ) ) ;
#35530 = PERSON_AND_ORGANIZATION_ROLE ( 'creator' ) ;
#35531 = CARTESIAN_POINT ( 'NONE',  ( 0.6577877771461339007, -1.521478526558629918, -0.6177285882837185715 ) ) ;
#35532 = CARTESIAN_POINT ( 'NONE',  ( 0.1847778408806958483, -0.8190323103295640284, 0.04085703638754438483 ) ) ;
#35533 = CARTESIAN_POINT ( 'NONE',  ( 0.4753073865181790536, -1.208389560008542585, 0.5132863017525766125 ) ) ;
#35534 = CARTESIAN_POINT ( 'NONE',  ( 0.2641583310953224961, -1.686482484943033766, 0.5673961214706590983 ) ) ;
#35535 = ADVANCED_FACE ( 'NONE', ( #10821 ), #986, .F. ) ;
#35536 = PRODUCT_DEFINITION ( 'UNKNOWN', '', #37152, #38872 ) ;
#35537 = CARTESIAN_POINT ( 'NONE',  ( 0.2949739106045629056, -1.710307911171992323, 0.7406796427396996618 ) ) ;
#35538 = CARTESIAN_POINT ( 'NONE',  ( 0.5866118575717673700, -1.567667628983530514, -0.4946522480570327285 ) ) ;
#35539 = CARTESIAN_POINT ( 'NONE',  ( -0.1603938765018561030, 0.4636889572247975266, 0.3382895567582887564 ) ) ;
#35540 = AXIS2_PLACEMENT_3D ( 'NONE', #6923, #12693, #25254 ) ;
#35541 = CARTESIAN_POINT ( 'NONE',  ( 0.04582889109739276406, -0.3361233334070946599, 0.3523147457849545305 ) ) ;
#35542 = CARTESIAN_POINT ( 'NONE',  ( 0.1826134026666640375, -1.261648033191452578, 0.4282186462236585722 ) ) ;
#35543 = CIRCLE ( 'NONE', #15200, 0.1000000000000000194 ) ;
#35544 = APPLICATION_CONTEXT ( 'configuration controlled 3d designs of mechanical parts and assemblies' ) ;
#35545 = EDGE_LOOP ( 'NONE', ( #30337, #23415, #14269, #28644, #5831, #22094 ) ) ;
#35546 = ORIENTED_EDGE ( 'NONE', *, *, #20803, .F. ) ;
#35547 = VECTOR ( 'NONE', #20702, 39.37007874015748143 ) ;
#35548 =( BOUNDED_SURFACE ( )  B_SPLINE_SURFACE ( 3, 2, ( 
 ( #25713, #12970, #16656 ),
 ( #35179, #6771, #22859 ),
 ( #19554, #12757, #13363 ),
 ( #9863, #25318, #4087 ) ),
 .UNSPECIFIED., .F., .F., .T. ) 
 B_SPLINE_SURFACE_WITH_KNOTS ( ( 4, 4 ),
 ( 3, 3 ),
 ( 1.965170647738601062E-15, 0.0007359428493836263222 ),
 ( 0.000000000000000000, 1.000000000000000000 ),
 .UNSPECIFIED. ) 
 GEOMETRIC_REPRESENTATION_ITEM ( )  RATIONAL_B_SPLINE_SURFACE ( (
 ( 1.000000000000000000, 0.8602827799852004187, 1.000000000000000000),
 ( 1.000000000000000000, 0.8187812255249553584, 1.000000000000000000),
 ( 1.000000000000000000, 0.7657952688647495787, 1.000000000000000000),
 ( 1.000000000000000000, 0.6984366549430200966, 1.000000000000000000) ) ) 
 REPRESENTATION_ITEM ( '' )  SURFACE ( )  );
#35549 = CARTESIAN_POINT ( 'NONE',  ( 0.4094665197507286747, -1.132124008075320098, 0.5707417262808780478 ) ) ;
#35550 = EDGE_LOOP ( 'NONE', ( #25410, #9092, #26510, #19766 ) ) ;
#35551 = AXIS2_PLACEMENT_3D ( 'NONE', #22370, #19278, #38180 ) ;
#35552 = CARTESIAN_POINT ( 'NONE',  ( -0.03159140494780145886, -0.05458666898339269852, 0.4890560705835251265 ) ) ;
#35553 = CARTESIAN_POINT ( 'NONE',  ( 0.5776039811709874350, -1.609991024422577466, -0.4771844860517738818 ) ) ;
#35555 = B_SPLINE_CURVE_WITH_KNOTS ( 'NONE', 3,
 ( #36908, #15312, #12232, #21086 ),
 .UNSPECIFIED., .F., .F.,
 ( 4, 4 ),
 ( 8.673617379883833249E-19, 0.0003934542678113530680 ),
 .UNSPECIFIED. ) ;
#35554 = TOROIDAL_SURFACE ( 'NONE', #28338, 0.07749999999977555398, 0.01000000000000000021 ) ;
#35556 = CARTESIAN_POINT ( 'NONE',  ( 0.5529494632797998799, -1.383080504355475249, 0.6300486131270075507 ) ) ;
#35558 = VERTEX_POINT ( 'NONE', #10600 ) ;
#35557 = CARTESIAN_POINT ( 'NONE',  ( 0.1499999999999993561, 0.000000000000000000, 0.000000000000000000 ) ) ;
#35559 = CARTESIAN_POINT ( 'NONE',  ( 0.5136166297679740644, -1.127695158652323615, 0.6751074532211280843 ) ) ;
#35560 = CARTESIAN_POINT ( 'NONE',  ( 0.3879575449432395851, -1.659955875966154126, -0.6176084244450640304 ) ) ;
#35561 = ORIENTED_EDGE ( 'NONE', *, *, #35188, .F. ) ;
#35562 = CYLINDRICAL_SURFACE ( 'NONE', #4763, 0.1033070866141734129 ) ;
#35563 = VERTEX_POINT ( 'NONE', #26065 ) ;
#35564 = CARTESIAN_POINT ( 'NONE',  ( 0.3293980905737597942, -1.639100469172996677, 0.6107778528379868010 ) ) ;
#35566 = CARTESIAN_POINT ( 'NONE',  ( -0.04229956186878663926, -0.2683474741743150926, 0.3842687663629376082 ) ) ;
#35565 = CARTESIAN_POINT ( 'NONE',  ( 0.6126507545533108612, -1.600805309556822209, 0.4340437436598985066 ) ) ;
#35567 = CARTESIAN_POINT ( 'NONE',  ( -0.01548846960707517956, -0.3880410510314797334, -0.3755318131854984420 ) ) ;
#35568 = CARTESIAN_POINT ( 'NONE',  ( 0.01274160805156434109, -1.703734511057651835, -0.3678759453203773178 ) ) ;
#35569 = ORIENTED_EDGE ( 'NONE', *, *, #19299, .T. ) ;
#35570 = TOROIDAL_SURFACE ( 'NONE', #25718, 0.9237847906030132172, 0.01499999999999999944 ) ;
#35571 = CARTESIAN_POINT ( 'NONE',  ( 0.5447008582413235267, -1.168329489522004216, 0.5018407269173935648 ) ) ;
#35572 = CARTESIAN_POINT ( 'NONE',  ( 0.2001178498007331608, -0.8475313208254383612, 0.3327188987815731802 ) ) ;
#35573 = CARTESIAN_POINT ( 'NONE',  ( 0.1999999999999789724, -2.097675824466503247, -0.7286991843995637153 ) ) ;
#35574 = EDGE_CURVE ( 'NONE', #15099, #5283, #7474, .T. ) ;
#35575 = CARTESIAN_POINT ( 'NONE',  ( 0.3657412124346848259, -2.011863122366571055, -0.5036770633976842548 ) ) ;
#35576 = CARTESIAN_POINT ( 'NONE',  ( 0.1050961439476602449, -0.8310223100206696190, 0.2465440532630112369 ) ) ;
#35577 = DIRECTION ( 'NONE',  ( 1.000000000000000000, 2.341930812374887555E-31, -1.664003471950578127E-31 ) ) ;
#35578 = EDGE_CURVE ( 'NONE', #23080, #39766, #31141, .T. ) ;
#35579 = CARTESIAN_POINT ( 'NONE',  ( 0.05634304521267768928, 0.01028134608272430507, -0.4588823192046728727 ) ) ;
#35580 = EDGE_CURVE ( 'NONE', #26731, #20917, #11074, .T. ) ;
#35581 = CARTESIAN_POINT ( 'NONE',  ( -0.1589247078932900514, 0.4934387919092068087, 0.3384493358270272978 ) ) ;
#35582 = AXIS2_PLACEMENT_3D ( 'NONE', #21436, #39717, #33964 ) ;
#35583 = DIRECTION ( 'NONE',  ( 0.000000000000000000, 0.000000000000000000, -1.000000000000000000 ) ) ;
#35584 = AXIS2_PLACEMENT_3D ( 'NONE', #16759, #13847, #32367 ) ;
#35585 = CARTESIAN_POINT ( 'NONE',  ( 0.03309060444528726108, 0.5154120966056442432, 0.07470591001490144156 ) ) ;
#35586 = DIRECTION ( 'NONE',  ( 1.000000000000000000, 0.000000000000000000, 0.000000000000000000 ) ) ;
#35587 = CARTESIAN_POINT ( 'NONE',  ( 0.03113248654051816583, -0.03575622569115821658, -0.1978615321325044307 ) ) ;
#35588 = VECTOR ( 'NONE', #25028, 39.37007874015748143 ) ;
#35589 = B_SPLINE_CURVE_WITH_KNOTS ( 'NONE', 3,
 ( #21010, #26970, #11134, #2493, #30065, #1702, #39504, #15035, #27584, #14221 ),
 .UNSPECIFIED., .F., .F.,
 ( 4, 3, 3, 4 ),
 ( 0.002857558714824972711, 0.003238527401515360615, 0.003619527401515320545, 0.003619558715365647078 ),
 .UNSPECIFIED. ) ;
#35590 = CARTESIAN_POINT ( 'NONE',  ( 0.06488195170228858166, -1.341118445645211654, 0.5728004737317409223 ) ) ;
#35591 = CARTESIAN_POINT ( 'NONE',  ( 0.1809266711160160690, -0.4989356743641660263, 0.1166738295573907097 ) ) ;
#35592 = CARTESIAN_POINT ( 'NONE',  ( 0.1048189938829944684, -1.403947404827792012, 0.6087930347991732383 ) ) ;
#35593 = EDGE_CURVE ( 'NONE', #1786, #9066, #35738, .T. ) ;
#35594 = CARTESIAN_POINT ( 'NONE',  ( 0.3504004095185141443, -1.746198910743387733, 0.4438683260553373811 ) ) ;
#35595 = CARTESIAN_POINT ( 'NONE',  ( 0.3581651676567015330, -1.812542450072600841, -0.6671711558045307910 ) ) ;
#35596 = CARTESIAN_POINT ( 'NONE',  ( 0.3012979652686071930, -1.678591049238880917, 0.8711002189715364441 ) ) ;
#35597 = CARTESIAN_POINT ( 'NONE',  ( -0.2399999999999999079, -2.003129936916423048, -0.4197911229995844873 ) ) ;
#35598 = ORIENTED_EDGE ( 'NONE', *, *, #14283, .T. ) ;
#35599 = EDGE_LOOP ( 'NONE', ( #424, #18510, #26469 ) ) ;
#35600 = CARTESIAN_POINT ( 'NONE',  ( -0.2746410161513779258, -3.705001275441084818, -0.3950781284944322458 ) ) ;
#35601 = ORIENTED_EDGE ( 'NONE', *, *, #28356, .F. ) ;
#35602 = CARTESIAN_POINT ( 'NONE',  ( -0.2746410161513782033, -2.289343986263487896, -0.7686455968847020204 ) ) ;
#35603 = VECTOR ( 'NONE', #17664, 39.37007874015748854 ) ;
#35604 = CARTESIAN_POINT ( 'NONE',  ( 0.6024792198024999657, -1.483053084053396420, 0.5847252747985980381 ) ) ;
#35606 = ORIENTED_EDGE ( 'NONE', *, *, #5851, .T. ) ;
#35605 = CARTESIAN_POINT ( 'NONE',  ( 0.5524261267419869892, -1.184164381802659927, 0.6057417262809862146 ) ) ;
#35608 = ORIENTED_EDGE ( 'NONE', *, *, #12008, .T. ) ;
#35607 = ORIENTED_EDGE ( 'NONE', *, *, #19748, .T. ) ;
#35609 = CARTESIAN_POINT ( 'NONE',  ( -0.2300000000000000100, 0.5182417262804744906, 0.3749999999999995559 ) ) ;
#35610 = VECTOR ( 'NONE', #35838, 39.37007874015748143 ) ;
#35611 = ORIENTED_EDGE ( 'NONE', *, *, #35783, .F. ) ;
#35612 = AXIS2_PLACEMENT_3D ( 'NONE', #280, #12777, #25338 ) ;
#35613 = CARTESIAN_POINT ( 'NONE',  ( -0.01400817393110175522, -0.5278220070374219919, 0.1759774557947419160 ) ) ;
#35614 = DIRECTION ( 'NONE',  ( 1.000000000000000000, 0.000000000000000000, 0.000000000000000000 ) ) ;
#35615 = DIRECTION ( 'NONE',  ( -1.000000000000000000, -2.276539994720197063E-15, 0.000000000000000000 ) ) ;
#35616 = DATE_TIME_ROLE ( 'classification_date' ) ;
#35617 = AXIS2_PLACEMENT_3D ( 'NONE', #16947, #16342, #25813 ) ;
#35618 = CARTESIAN_POINT ( 'NONE',  ( 0.004127512716747100754, -0.5275076572294757904, 0.1483282180229316405 ) ) ;
#35620 = ORIENTED_EDGE ( 'NONE', *, *, #22365, .T. ) ;
#35619 = VERTEX_POINT ( 'NONE', #20478 ) ;
#35621 = CARTESIAN_POINT ( 'NONE',  ( 0.09109308586799420848, -0.7953216885135077074, 0.2706080309223847236 ) ) ;
#35622 = EDGE_CURVE ( 'NONE', #33009, #2590, #11026, .T. ) ;
#35623 = DIRECTION ( 'NONE',  ( 0.000000000000000000, 0.000000000000000000, -1.000000000000000000 ) ) ;
#35624 = CARTESIAN_POINT ( 'NONE',  ( 0.5236184131203611702, -1.488138999244633220, 0.7296234892006074890 ) ) ;
#35625 = DIRECTION ( 'NONE',  ( 2.465190328815661892E-32, 1.000000000000000000, 6.656013887802287108E-31 ) ) ;
#35626 = CARTESIAN_POINT ( 'NONE',  ( 0.5039816396062418713, -1.584398255417020174, -0.4834617919644653150 ) ) ;
#35627 = CARTESIAN_POINT ( 'NONE',  ( 0.2161879510971927432, -1.277123080371499242, -0.3144976166544468099 ) ) ;
#35628 = EDGE_CURVE ( 'NONE', #2643, #8839, #3721, .T. ) ;
#35629 = CARTESIAN_POINT ( 'NONE',  ( 0.3186320389496528627, -1.760431904683431359, 0.5682417262808792113 ) ) ;
#35630 = DIRECTION ( 'NONE',  ( 0.9823333030490228879, -0.1871397384865027547, 0.000000000000000000 ) ) ;
#35631 = EDGE_CURVE ( 'NONE', #28175, #2063, #29218, .T. ) ;
#35632 = CARTESIAN_POINT ( 'NONE',  ( 0.4211301194118072244, -1.688827985529782527, 0.4182417262808776903 ) ) ;
#35633 = FACE_OUTER_BOUND ( 'NONE', #36753, .T. ) ;
#35634 = CARTESIAN_POINT ( 'NONE',  ( -0.2399999999999999079, -2.511040369707300268, -0.4948468226404901804 ) ) ;
#35635 = CARTESIAN_POINT ( 'NONE',  ( 3.473743519314094728E-08, -0.7045837285689108276, -0.1152398889879612948 ) ) ;
#35636 = CARTESIAN_POINT ( 'NONE',  ( 0.2672861266253624413, -0.9758538585998212112, 0.7531240496249852479 ) ) ;
#35638 = EDGE_CURVE ( 'NONE', #40101, #3578, #11423, .T. ) ;
#35637 =( NAMED_UNIT ( * ) SI_UNIT ( $, .STERADIAN. ) SOLID_ANGLE_UNIT ( ) );
#35639 = AXIS2_PLACEMENT_3D ( 'NONE', #12986, #21449, #37875 ) ;
#35640 = DIRECTION ( 'NONE',  ( -0.8660512985181130219, -0.4999551463232378978, -3.305494428309464757E-15 ) ) ;
#35641 = CARTESIAN_POINT ( 'NONE',  ( 0.1233923337978296703, -1.433947342477501108, 0.6209663710929820279 ) ) ;
#35642 = CARTESIAN_POINT ( 'NONE',  ( 0.2554252512568409572, -0.9178124959013912454, 0.5002157811656953168 ) ) ;
#35643 = CALENDAR_DATE ( 2026, 13, 10 ) ;
#35644 = VECTOR ( 'NONE', #22014, 39.37007874015748143 ) ;
#35645 = AXIS2_PLACEMENT_3D ( 'NONE', #16239, #19525, #7336 ) ;
#35646 = EDGE_CURVE ( 'NONE', #19133, #37952, #36381, .T. ) ;
#35647 = ADVANCED_FACE ( 'NONE', ( #14178 ), #19974, .T. ) ;
#35648 = AXIS2_PLACEMENT_3D ( 'NONE', #3319, #22476, #22692 ) ;
#35649 = ADVANCED_FACE ( 'NONE', ( #35984 ), #20562, .F. ) ;
#35650 = CARTESIAN_POINT ( 'NONE',  ( 0.7227111374362353846, -1.527409785822605448, -0.4111404562665418871 ) ) ;
#35651 = DIRECTION ( 'NONE',  ( 7.771561172376107616E-16, -7.170354002788761615E-17, 1.000000000000000000 ) ) ;
#35652 = AXIS2_PLACEMENT_3D ( 'NONE', #9164, #18027, #9365 ) ;
#35653 = VERTEX_POINT ( 'NONE', #24618 ) ;
#35654 = FACE_OUTER_BOUND ( 'NONE', #39419, .T. ) ;
#35655 = CARTESIAN_POINT ( 'NONE',  ( 0.002952521020825130300, -0.5558164471492254011, 0.2655225723378386027 ) ) ;
#35656 = CARTESIAN_POINT ( 'NONE',  ( 0.2209260011871197471, -1.309027873449325918, -0.6184399470714002645 ) ) ;
#35657 = ORIENTED_EDGE ( 'NONE', *, *, #38948, .F. ) ;
#35658 = CARTESIAN_POINT ( 'NONE',  ( 0.3269417016373100116, -1.755644436858573076, 0.4716675315899548360 ) ) ;
#35659 = CARTESIAN_POINT ( 'NONE',  ( 0.5195754528810989648, -1.145330933930835959, 0.8096739517683957388 ) ) ;
#35661 = ORIENTED_EDGE ( 'NONE', *, *, #11197, .T. ) ;
#35660 = ORIENTED_EDGE ( 'NONE', *, *, #36036, .T. ) ;
#35662 = DIRECTION ( 'NONE',  ( 0.000000000000000000, 0.8951985963847274297, -0.4456674466806093138 ) ) ;
#35663 = ORIENTED_EDGE ( 'NONE', *, *, #15038, .T. ) ;
#35664 = CARTESIAN_POINT ( 'NONE',  ( 0.3657108496600825487, -1.757413321709223375, -0.5058915056509059038 ) ) ;
#35665 = CARTESIAN_POINT ( 'NONE',  ( 0.2362067350217224027, -1.230737272509785374, 0.4282273956715025864 ) ) ;
#35666 = AXIS2_PLACEMENT_3D ( 'NONE', #9423, #9033, #15403 ) ;
#35667 = CARTESIAN_POINT ( 'NONE',  ( -0.2399999999999999079, -2.139295658456680904, -0.2024034539465678073 ) ) ;
#35668 = ORIENTED_EDGE ( 'NONE', *, *, #3900, .T. ) ;
#35669 = CARTESIAN_POINT ( 'NONE',  ( 0.09374999999999988898, -0.4830108143257719755, 0.3319492704185081910 ) ) ;
#35670 = CARTESIAN_POINT ( 'NONE',  ( 0.09324156912962643096, -0.6558780651247091420, 0.2654224007799687035 ) ) ;
#35671 = CONICAL_SURFACE ( 'NONE', #36303, 0.07499999999999991396, 0.6931599075767558293 ) ;
#35672 = CARTESIAN_POINT ( 'NONE',  ( 0.07626770091217156822, -0.8479114564755200201, 0.8336461691634142745 ) ) ;
#35673 = CIRCLE ( 'NONE', #17931, 0.5400000000000018119 ) ;
#35674 = CARTESIAN_POINT ( 'NONE',  ( 0.1925202373472624240, -0.9012288813172684154, 0.7215585555966789189 ) ) ;
#35676 = CARTESIAN_POINT ( 'NONE',  ( 0.3137153524386490644, -1.648232696675291375, 0.5962818595802683586 ) ) ;
#35675 = CARTESIAN_POINT ( 'NONE',  ( 0.1676876122360048404, -1.285305603201868374, 0.9459303112033679017 ) ) ;
#35677 = CARTESIAN_POINT ( 'NONE',  ( 0.3140370939074847434, -1.084786762411256378, 0.6412117272335754459 ) ) ;
#35678 = ORIENTED_EDGE ( 'NONE', *, *, #19848, .F. ) ;
#35679 = B_SPLINE_CURVE_WITH_KNOTS ( 'NONE', 3,
 ( #29135, #32414, #7105, #788 ),
 .UNSPECIFIED., .F., .F.,
 ( 4, 4 ),
 ( 1.753349224617995719E-05, 0.001120479941338546354 ),
 .UNSPECIFIED. ) ;
#35680 = ORIENTED_EDGE ( 'NONE', *, *, #33352, .T. ) ;
#35681 = VECTOR ( 'NONE', #33916, 39.37007874015748143 ) ;
#35682 = EDGE_CURVE ( 'NONE', #5190, #9409, #14711, .T. ) ;
#35683 = CARTESIAN_POINT ( 'NONE',  ( 0.3666170748374983357, -1.617430218101400197, 0.5510161745712417458 ) ) ;
#35684 = CARTESIAN_POINT ( 'NONE',  ( 0.1897362042065962873, -0.5343739875968438469, 0.1562402822563540850 ) ) ;
#35685 = EDGE_CURVE ( 'NONE', #39819, #10668, #15397, .T. ) ;
#35686 = AXIS2_PLACEMENT_3D ( 'NONE', #39332, #10754, #36046 ) ;
#35687 = CARTESIAN_POINT ( 'NONE',  ( 0.6935470237484337996, -1.428868995382490237, 0.5856070495622788252 ) ) ;
#35688 = CARTESIAN_POINT ( 'NONE',  ( -0.03301200226531718351, -0.5156245478783716418, -0.07469833545740128811 ) ) ;
#35689 = CARTESIAN_POINT ( 'NONE',  ( 0.1909286924077254199, -1.257064795538238577, -0.7137147910238503812 ) ) ;
#35690 = DIRECTION ( 'NONE',  ( 1.000000000000000000, 0.000000000000000000, 0.000000000000000000 ) ) ;
#35691 = CARTESIAN_POINT ( 'NONE',  ( 0.4220340746365390805, -1.009949560908969035, 0.7308913177996746446 ) ) ;
#35692 = CARTESIAN_POINT ( 'NONE',  ( 7.512581982576723358E-16, 0.3059742766594581997, -3.756290991288361679E-16 ) ) ;
#35693 = CARTESIAN_POINT ( 'NONE',  ( 0.06842911028247611327, -1.327649046458937443, 0.5682133453004688528 ) ) ;
#35694 = AXIS2_PLACEMENT_3D ( 'NONE', #22318, #10162, #38331 ) ;
#35695 = FACE_OUTER_BOUND ( 'NONE', #978, .T. ) ;
#35696 = FACE_OUTER_BOUND ( 'NONE', #4775, .T. ) ;
#35697 = CARTESIAN_POINT ( 'NONE',  ( 0.3113442856022401450, -1.065761248458108046, 0.7391908608033311845 ) ) ;
#35698 = CARTESIAN_POINT ( 'NONE',  ( -0.04139678531769525743, -0.2626830136224073131, -0.3904580303439415534 ) ) ;
#35699 = CIRCLE ( 'NONE', #27813, 0.1400000000000005684 ) ;
#35700 = ORIENTED_EDGE ( 'NONE', *, *, #23991, .F. ) ;
#35701 = FACE_OUTER_BOUND ( 'NONE', #32675, .T. ) ;
#35702 = CARTESIAN_POINT ( 'NONE',  ( -0.02953079040095700838, 0.09152108205202039160, -0.5223162075576429642 ) ) ;
#35703 = FACE_OUTER_BOUND ( 'NONE', #11315, .T. ) ;
#35704 = CARTESIAN_POINT ( 'NONE',  ( 0.6590705178848084156, -1.601721441849921268, 0.5182417262812423209 ) ) ;
#35705 = VECTOR ( 'NONE', #6145, 39.37007874015748854 ) ;
#35706 = CARTESIAN_POINT ( 'NONE',  ( 0.2784898103895053767, -1.320042667948280846, 0.5909764709513882774 ) ) ;
#35707 = ORIENTED_EDGE ( 'NONE', *, *, #30679, .F. ) ;
#35708 = CARTESIAN_POINT ( 'NONE',  ( 0.4621675984227249789, -1.110867290327286261, 0.5635151220948720896 ) ) ;
#35709 = CARTESIAN_POINT ( 'NONE',  ( 0.04285640132273748487, 0.07199195674534319966, 0.4895487002729358439 ) ) ;
#35710 = CARTESIAN_POINT ( 'NONE',  ( 0.3204479958614548929, -1.182666560659948907, 0.5682417262808776570 ) ) ;
#35711 = DIRECTION ( 'NONE',  ( -2.465190328815661892E-32, -1.000000000000000000, -6.656013887802287108E-31 ) ) ;
#35712 = CARTESIAN_POINT ( 'NONE',  ( 0.3497762486267798621, -1.084349969738368502, 0.7277452793936995956 ) ) ;
#35714 = LINE ( 'NONE', #7523, #40454 ) ;
#35713 = DIRECTION ( 'NONE',  ( 1.000000000000000000, -0.000000000000000000, -0.000000000000000000 ) ) ;
#35715 = DIRECTION ( 'NONE',  ( -1.000000000000000000, 0.000000000000000000, 0.000000000000000000 ) ) ;
#35716 = VERTEX_POINT ( 'NONE', #10898 ) ;
#35717 = DIRECTION ( 'NONE',  ( -0.9848077530122080203, -0.1736481776669303589, 4.095352323445923521E-18 ) ) ;
#35718 = ORIENTED_EDGE ( 'NONE', *, *, #21070, .F. ) ;
#35719 = CARTESIAN_POINT ( 'NONE',  ( 0.3806051526081477010, -1.502956011673624026, 0.8238138617331723923 ) ) ;
#35721 = CARTESIAN_POINT ( 'NONE',  ( 0.1111486238615575634, -0.9218372719158527406, 0.08682267064788348754 ) ) ;
#35720 = CARTESIAN_POINT ( 'NONE',  ( 0.08893475363215910812, -0.5779476940138750241, 0.05184119719358894901 ) ) ;
#35722 = CARTESIAN_POINT ( 'NONE',  ( 0.1886749731537993857, -1.710201859072882691, -0.3585638508453504181 ) ) ;
#35723 = EDGE_LOOP ( 'NONE', ( #11164, #26326, #14561, #14279 ) ) ;
#35724 = CIRCLE ( 'NONE', #33757, 0.1600000000000007527 ) ;
#35725 = ORIENTED_EDGE ( 'NONE', *, *, #3126, .T. ) ;
#35726 = LINE ( 'NONE', #1207, #20840 ) ;
#35727 = CARTESIAN_POINT ( 'NONE',  ( 0.1223120210888352516, -0.5860525448271070026, 0.2865477404261148608 ) ) ;
#35728 = ORIENTED_EDGE ( 'NONE', *, *, #7152, .F. ) ;
#35729 = CARTESIAN_POINT ( 'NONE',  ( 0.1874453682798400689, -0.6903079694140360489, 0.04813715558869984673 ) ) ;
#35730 = CARTESIAN_POINT ( 'NONE',  ( 0.05561310505366579698, -0.4442420632723498852, 0.1228816621031077888 ) ) ;
#35731 = AXIS2_PLACEMENT_3D ( 'NONE', #7567, #7959, #20336 ) ;
#35732 = VECTOR ( 'NONE', #2437, 39.37007874015749564 ) ;
#35733 = CARTESIAN_POINT ( 'NONE',  ( -2.112273405726188513E-14, -2.097675824466503691, -0.6968637352380161465 ) ) ;
#35734 = PRODUCT_DEFINITION_SHAPE ( 'NONE', 'NONE',  #40648 ) ;
#35735 = CARTESIAN_POINT ( 'NONE',  ( 0.2145758709995234104, -1.243149601538450000, 0.4716904324752760336 ) ) ;
#35736 = CARTESIAN_POINT ( 'NONE',  ( 0.3946758974465285896, -1.754660907246334833, -0.5213155647942423476 ) ) ;
#35737 = CARTESIAN_POINT ( 'NONE',  ( 0.3434800707737146741, -1.169184835483404905, 0.4282596159937968605 ) ) ;
#35738 = CIRCLE ( 'NONE', #9453, 0.06250000000000001388 ) ;
#35739 = CARTESIAN_POINT ( 'NONE',  ( 0.7346172259536333238, -1.494169854247700657, 0.6985599367358283907 ) ) ;
#35740 = CIRCLE ( 'NONE', #2254, 0.01499999999999995087 ) ;
#35741 = DIRECTION ( 'NONE',  ( -0.000000000000000000, -0.9396926207859078728, -0.3420201433256705448 ) ) ;
#35742 = CARTESIAN_POINT ( 'NONE',  ( 0.1499999999999993561, 0.000000000000000000, 0.000000000000000000 ) ) ;
#35743 = DATE_TIME_ROLE ( 'creation_date' ) ;
#35744 = B_SPLINE_CURVE_WITH_KNOTS ( 'NONE', 3,
 ( #40057, #6657, #30618, #27535, #3379, #25419, #39873, #2445, #11693, #12099, #37743, #24449, #36771, #9761, #8801, #21381, #15934, #11498 ),
 .UNSPECIFIED., .F., .F.,
 ( 4, 2, 2, 2, 2, 2, 2, 2, 4 ),
 ( -0.002633528389679740730, -0.001975271857855738500, -0.001317015326031736704, -0.0006587587942077344737, -5.022623837326774254E-07, 0.0006577542694402691188, 0.001316010801264271782, 0.001974267333088273579, 0.002632523864912275375 ),
 .UNSPECIFIED. ) ;
#35745 = CARTESIAN_POINT ( 'NONE',  ( 0.1499999999999993561, 4.163336342344336410E-17, 0.1249999999999999584 ) ) ;
#35746 = CARTESIAN_POINT ( 'NONE',  ( 0.04230170315644143225, 0.2684795119051849865, 0.3841679273482342949 ) ) ;
#35747 = CARTESIAN_POINT ( 'NONE',  ( 0.1846016914021299526, -0.8353733999320747117, 0.06670577366108822182 ) ) ;
#35748 = CARTESIAN_POINT ( 'NONE',  ( 0.4144545104481285880, -1.243517080461129076, 0.4993477989703495878 ) ) ;
#35749 = DIRECTION ( 'NONE',  ( 1.000000000000000000, 0.000000000000000000, 1.138269997360105631E-15 ) ) ;
#35750 = CARTESIAN_POINT ( 'NONE',  ( 0.05848126963139189949, -0.9969932945501481791, 0.7623047753129613691 ) ) ;
#35751 = CARTESIAN_POINT ( 'NONE',  ( 0.5909067581049517459, -1.559819890239460882, -0.5597400662906658608 ) ) ;
#35752 = AXIS2_PLACEMENT_3D ( 'NONE', #34845, #3587, #19440 ) ;
#35753 = FACE_OUTER_BOUND ( 'NONE', #25147, .T. ) ;
#35754 = CYLINDRICAL_SURFACE ( 'NONE', #21267, 0.02000000000000003858 ) ;
#35755 = CARTESIAN_POINT ( 'NONE',  ( -0.04229883635638079231, -0.2789693855191311411, 0.3765531589812280977 ) ) ;
#35756 = AXIS2_PLACEMENT_3D ( 'NONE', #5295, #15398, #21168 ) ;
#35757 = VERTEX_POINT ( 'NONE', #1449 ) ;
#35758 = AXIS2_PLACEMENT_3D ( 'NONE', #11815, #27274, #33842 ) ;
#35759 = ORIENTED_EDGE ( 'NONE', *, *, #39919, .T. ) ;
#35760 = AXIS2_PLACEMENT_3D ( 'NONE', #602, #19076, #35110 ) ;
#35761 = CARTESIAN_POINT ( 'NONE',  ( 0.1435064959217801916, -1.283467536720964697, 0.5197417262808780025 ) ) ;
#35762 = VERTEX_POINT ( 'NONE', #4498 ) ;
#35763 = AXIS2_PLACEMENT_3D ( 'NONE', #34773, #9482, #282 ) ;
#35764 = CARTESIAN_POINT ( 'NONE',  ( 0.08989401589083206856, -0.5588208839049469967, 0.1462139476000107741 ) ) ;
#35765 = CARTESIAN_POINT ( 'NONE',  ( 0.3474212099432354983, -1.070521011291321933, 0.7674123779357524544 ) ) ;
#35767 = VERTEX_POINT ( 'NONE', #40223 ) ;
#35766 = CARTESIAN_POINT ( 'NONE',  ( -0.04582889109739315958, 0.4790149006698655176, 0.08746027838083748895 ) ) ;
#35768 = CARTESIAN_POINT ( 'NONE',  ( 0.5265921910155209051, -1.145228776028037521, 0.6635139613180396356 ) ) ;
#35769 = CIRCLE ( 'NONE', #39732, 0.009999999999999975922 ) ;
#35770 = CARTESIAN_POINT ( 'NONE',  ( 0.1279017468704548299, -0.4488044174422846089, 0.1457404026636500427 ) ) ;
#35771 = ORIENTED_EDGE ( 'NONE', *, *, #38152, .F. ) ;
#35772 = DIRECTION ( 'NONE',  ( -0.8155480960843040084, -0.4959942097372370129, -0.2981124735404419579 ) ) ;
#35773 = AXIS2_PLACEMENT_3D ( 'NONE', #16082, #28624, #494 ) ;
#35774 = CARTESIAN_POINT ( 'NONE',  ( 0.3308004652115096866, -1.635985480546734205, 0.6545755976240583696 ) ) ;
#35776 = CARTESIAN_POINT ( 'NONE',  ( -0.04154009738085443632, -0.4523583096281919014, 0.1287716261385827843 ) ) ;
#35775 = CARTESIAN_POINT ( 'NONE',  ( 0.6318873531608050209, -1.583827858112001552, 0.4267529692672295538 ) ) ;
#35777 = CARTESIAN_POINT ( 'NONE',  ( -0.08000000000000000167, -1.845925619402022155, -0.2644148183989317724 ) ) ;
#35778 = CARTESIAN_POINT ( 'NONE',  ( 0.09811733985272647063, -1.358709011939960964, -0.3562893400942814259 ) ) ;
#35779 = ORIENTED_EDGE ( 'NONE', *, *, #29072, .F. ) ;
#35780 = CARTESIAN_POINT ( 'NONE',  ( -0.2399999999999999079, -3.811657270145150989, -0.1642545796697100491 ) ) ;
#35781 = CARTESIAN_POINT ( 'NONE',  ( 0.1831885191726025097, -1.261723239126609775, -0.7105730338104595534 ) ) ;
#35782 = CARTESIAN_POINT ( 'NONE',  ( 0.01548846960707511190, -0.2306506793133099031, -0.4716198300880795613 ) ) ;
#35783 = EDGE_CURVE ( 'NONE', #30904, #29395, #18651, .T. ) ;
#35784 = CARTESIAN_POINT ( 'NONE',  ( 0.1962839440205723096, -0.9538400423320417820, 0.6688300417027344125 ) ) ;
#35785 = FACE_OUTER_BOUND ( 'NONE', #14115, .T. ) ;
#35786 = APPLIED_DATE_AND_TIME_ASSIGNMENT ( #9515, #31725, ( #39812 ) ) ;
#35787 = AXIS2_PLACEMENT_3D ( 'NONE', #30361, #1987, #11228 ) ;
#35788 = CARTESIAN_POINT ( 'NONE',  ( 0.4716580862946758157, -1.112877053019780016, 0.5495408069278913121 ) ) ;
#35789 = AXIS2_PLACEMENT_3D ( 'NONE', #23567, #20066, #11012 ) ;
#35790 = AXIS2_PLACEMENT_3D ( 'NONE', #1671, #20578, #30036 ) ;
#35791 = LINE ( 'NONE', #38063, #21909 ) ;
#35792 = DIRECTION ( 'NONE',  ( 1.000000000000000000, 0.000000000000000000, 0.000000000000000000 ) ) ;
#35793 = DIRECTION ( 'NONE',  ( 1.000000000000000000, 2.341930812374887555E-31, -1.664003471950578127E-31 ) ) ;
#35794 = CARTESIAN_POINT ( 'NONE',  ( 0.4370582351334127980, -1.114183277624516410, -0.6414096453823977528 ) ) ;
#35795 = CARTESIAN_POINT ( 'NONE',  ( 0.4165761542997364897, -1.741708882820427906, 0.5182417262812423209 ) ) ;
#35796 = APPROVAL_PERSON_ORGANIZATION ( #36794, #32073, #30218 ) ;
#35797 = CARTESIAN_POINT ( 'NONE',  ( 0.3554163599750468361, -1.162345695606875839, 0.4422132562362469099 ) ) ;
#35798 = CARTESIAN_POINT ( 'NONE',  ( -0.05464101615137796630, -1.622350287959229087, -0.08960079202753243321 ) ) ;
#35799 = VECTOR ( 'NONE', #8818, 39.37007874015748143 ) ;
#35800 = DIRECTION ( 'NONE',  ( 0.000000000000000000, 0.000000000000000000, -1.000000000000000000 ) ) ;
#35801 = CARTESIAN_POINT ( 'NONE',  ( 0.4764113678702300847, -1.677356869750545210, 0.4781561135235793403 ) ) ;
#35802 = CARTESIAN_POINT ( 'NONE',  ( 1.127432441697302489E-16, -0.01499999999999992832, 0.07499999999999998335 ) ) ;
#35803 = CARTESIAN_POINT ( 'NONE',  ( 0.3049719670396321414, -1.696434107116652434, 0.8435498759739918917 ) ) ;
#35804 = DIRECTION ( 'NONE',  ( 0.8660512985181135770, 0.4999551463232370652, 0.000000000000000000 ) ) ;
#35805 = ORIENTED_EDGE ( 'NONE', *, *, #29321, .F. ) ;
#35806 = EDGE_CURVE ( 'NONE', #33666, #22635, #5513, .T. ) ;
#35807 = VERTEX_POINT ( 'NONE', #4691 ) ;
#35808 = DIRECTION ( 'NONE',  ( -2.465190328815661892E-32, -1.000000000000000000, -6.656013887802287108E-31 ) ) ;
#35809 = ORIENTED_EDGE ( 'NONE', *, *, #20493, .F. ) ;
#35810 = LINE ( 'NONE', #16481, #32227 ) ;
#35811 = EDGE_CURVE ( 'NONE', #14767, #28470, #23283, .T. ) ;
#35812 = CARTESIAN_POINT ( 'NONE',  ( 0.4942140488756893713, -1.327628134470207222, 0.8104097437034657458 ) ) ;
#35814 = ORIENTED_EDGE ( 'NONE', *, *, #10193, .T. ) ;
#35813 = CARTESIAN_POINT ( 'NONE',  ( 0.008457857042273673326, -0.6665957502853808725, -0.01121200989691692289 ) ) ;
#35815 = VECTOR ( 'NONE', #21890, 39.37007874015748854 ) ;
#35816 = EDGE_CURVE ( 'NONE', #24060, #20188, #39024, .T. ) ;
#35818 = ORIENTED_EDGE ( 'NONE', *, *, #7894, .T. ) ;
#35817 = ORIENTED_EDGE ( 'NONE', *, *, #17335, .F. ) ;
#35819 = CARTESIAN_POINT ( 'NONE',  ( 0.05948319379729941764, -1.278145653519860536, 0.5182417262812423209 ) ) ;
#35820 = ORIENTED_EDGE ( 'NONE', *, *, #34392, .F. ) ;
#35821 = ORIENTED_EDGE ( 'NONE', *, *, #39120, .T. ) ;
#35822 = CARTESIAN_POINT ( 'NONE',  ( 0.1426205952518595221, -1.218146753663991610, 0.9251587076902523243 ) ) ;
#35824 = FACE_OUTER_BOUND ( 'NONE', #2735, .T. ) ;
#35823 = CARTESIAN_POINT ( 'NONE',  ( 0.04087116408466945350, 0.4416914123362158384, 0.1656680454788718726 ) ) ;
#35825 = APPLIED_APPROVAL_ASSIGNMENT ( #6886, ( #2626 ) ) ;
#35826 = CARTESIAN_POINT ( 'NONE',  ( -0.2300000000000000655, 0.5182417262804733804, 0.3749999999999999445 ) ) ;
#35827 = SECURITY_CLASSIFICATION_LEVEL ( 'unclassified' ) ;
#35828 = CARTESIAN_POINT ( 'NONE',  ( -0.002762107553692768041, -0.4210325180397656020, -0.1178596299512813528 ) ) ;
#35830 = VERTEX_POINT ( 'NONE', #15129 ) ;
#35829 = EDGE_LOOP ( 'NONE', ( #18014, #30566 ) ) ;
#35831 = CARTESIAN_POINT ( 'NONE',  ( 0.2310385060053183892, -0.9417727088514467049, 0.6570708109900642580 ) ) ;
#35832 = AXIS2_PLACEMENT_3D ( 'NONE', #4320, #13975, #25956 ) ;
#35833 = CARTESIAN_POINT ( 'NONE',  ( 0.04409305177916850171, -0.9987702684838598577, 0.6897599509476122215 ) ) ;
#35834 = CARTESIAN_POINT ( 'NONE',  ( 0.1255995385913393214, -0.7272598595541045485, 0.5480802707321428269 ) ) ;
#35835 = CARTESIAN_POINT ( 'NONE',  ( 0.1134734767189682914, -0.5850338423759841033, 0.2884401093049815956 ) ) ;
#35836 = DIRECTION ( 'NONE',  ( 0.000000000000000000, 5.978086547377981840E-31, 1.000000000000000000 ) ) ;
#35837 = ADVANCED_FACE ( 'NONE', ( #5858 ), #30970, .F. ) ;
#35838 = DIRECTION ( 'NONE',  ( 0.4999551463232372317, -0.8660512985181134660, 0.000000000000000000 ) ) ;
#35839 = FACE_OUTER_BOUND ( 'NONE', #31938, .T. ) ;
#35840 = CARTESIAN_POINT ( 'NONE',  ( 0.3853942601747663566, -1.722288293259479852, 0.6094916416589982733 ) ) ;
#35841 = CARTESIAN_POINT ( 'NONE',  ( 0.4221466955848551250, -1.651713303066375760, -0.3505199372179519379 ) ) ;
#35842 = CARTESIAN_POINT ( 'NONE',  ( 0.06277511499740180689, -1.333345291044720771, 0.5336558136334552671 ) ) ;
#35843 = DIRECTION ( 'NONE',  ( 1.000000000000000000, 0.000000000000000000, 0.000000000000000000 ) ) ;
#35844 = CARTESIAN_POINT ( 'NONE',  ( 0.08402806910823619468, -1.261043216642898868, -0.5155029497116575543 ) ) ;
#35845 = CARTESIAN_POINT ( 'NONE',  ( 0.01142394431942996696, -0.9136163810232513782, 0.01885333890477661895 ) ) ;
#35846 = CARTESIAN_POINT ( 'NONE',  ( 0.5775506772830608648, -1.469745956246417240, 0.6985825451078249149 ) ) ;
#35847 = CARTESIAN_POINT ( 'NONE',  ( 0.4972320539234349468, -1.080138254241686413, 0.5197417262808780025 ) ) ;
#35848 = AXIS2_PLACEMENT_3D ( 'NONE', #19882, #35111, #6917 ) ;
#35849 = VECTOR ( 'NONE', #13323, 39.37007874015748143 ) ;
#35850 = DIRECTION ( 'NONE',  ( 0.000000000000000000, 0.000000000000000000, -1.000000000000000000 ) ) ;
#35851 = CARTESIAN_POINT ( 'NONE',  ( 0.03762609415277568675, -1.032875954121303508, 0.6996461994120862782 ) ) ;
#35852 = CARTESIAN_POINT ( 'NONE',  ( 0.4919302148474398173, -1.082157928207513331, 0.5818935738131040258 ) ) ;
#35853 = PERSON_AND_ORGANIZATION ( #28500, #32463 ) ;
#35854 = CARTESIAN_POINT ( 'NONE',  ( 0.4624512237511245738, -1.047046041135732741, 0.8530670246638676346 ) ) ;
#35855 = APPLIED_APPROVAL_ASSIGNMENT ( #36280, ( #24016 ) ) ;
#35856 = DIRECTION ( 'NONE',  ( -0.4999551463232372317, 0.8660512985181134660, -0.000000000000000000 ) ) ;
#35857 = CIRCLE ( 'NONE', #8925, 0.01750000000000001554 ) ;
#35858 = CARTESIAN_POINT ( 'NONE',  ( 0.4809364209501173493, -1.175687667482560927, 0.4182417262808778013 ) ) ;
#35859 = EDGE_CURVE ( 'NONE', #22853, #39958, #18419, .T. ) ;
#35860 = ORIENTED_EDGE ( 'NONE', *, *, #17728, .T. ) ;
#35861 = CARTESIAN_POINT ( 'NONE',  ( 0.3198746602526446603, -1.759624966644469879, 0.5626316659645647089 ) ) ;
#35862 = CARTESIAN_POINT ( 'NONE',  ( 0.002367394983744824412, -0.5282119844061545777, 0.1443450864220834906 ) ) ;
#35863 = EDGE_CURVE ( 'NONE', #12532, #14064, #23256, .T. ) ;
#35864 = CARTESIAN_POINT ( 'NONE',  ( -2.070754768975509919, -0.09959325338431655739, 0.1000000000000005745 ) ) ;
#35865 = VERTEX_POINT ( 'NONE', #18227 ) ;
#35866 = CARTESIAN_POINT ( 'NONE',  ( 0.2109795887149964189, -1.360945235397178044, -0.5155029497116575543 ) ) ;
#35867 = EDGE_CURVE ( 'NONE', #37622, #24860, #38371, .T. ) ;
#35868 = CARTESIAN_POINT ( 'NONE',  ( 0.5289273032196292190, -1.159758851219879094, 0.8099624798310959273 ) ) ;
#35870 = VERTEX_POINT ( 'NONE', #19457 ) ;
#35869 = ORIENTED_EDGE ( 'NONE', *, *, #18964, .F. ) ;
#35871 = CARTESIAN_POINT ( 'NONE',  ( 0.02997031417520805083, -2.054978514977984450, -0.7138428137902104176 ) ) ;
#35872 = ORIENTED_EDGE ( 'NONE', *, *, #5390, .F. ) ;
#35873 = DIRECTION ( 'NONE',  ( 0.000000000000000000, 0.000000000000000000, -1.000000000000000000 ) ) ;
#35874 = DIRECTION ( 'NONE',  ( -1.000000000000000000, -0.000000000000000000, -0.000000000000000000 ) ) ;
#35875 = CARTESIAN_POINT ( 'NONE',  ( -0.05252359774140372833, 0.4432374118283854969, -0.1535299757497269879 ) ) ;
#35876 = ORIENTED_EDGE ( 'NONE', *, *, #241, .F. ) ;
#35877 = CARTESIAN_POINT ( 'NONE',  ( 0.008954545898026106121, -0.6173803428054009945, 0.003786539670926606597 ) ) ;
#35879 = EDGE_CURVE ( 'NONE', #25455, #29556, #6831, .T. ) ;
#35878 = CIRCLE ( 'NONE', #37851, 0.1946589359789743512 ) ;
#35880 = CARTESIAN_POINT ( 'NONE',  ( 0.09589697510153505355, -0.6621991411919149195, 0.2946228100768590319 ) ) ;
#35881 = CARTESIAN_POINT ( 'NONE',  ( 0.1581441334961056766, -1.100692414099352368, 0.9862425334140708655 ) ) ;
#35882 = CARTESIAN_POINT ( 'NONE',  ( 0.08736941714279185256, -0.5694091105756469151, 0.2584125436657497832 ) ) ;
#35884 = DIRECTION ( 'NONE',  ( 0.01455087615875041117, 0.9998941303973198913, 0.000000000000000000 ) ) ;
#35883 = CARTESIAN_POINT ( 'NONE',  ( 0.1144236352178722299, -0.5058114079956718134, -0.01341456787975157591 ) ) ;
#35885 = EDGE_CURVE ( 'NONE', #15800, #32375, #22344, .T. ) ;
#35886 = CARTESIAN_POINT ( 'NONE',  ( 0.1362976124207936068, -1.175113777419627858, 0.6553486967042546629 ) ) ;
#35887 = CARTESIAN_POINT ( 'NONE',  ( -0.09579104668929040722, -0.04310840302197994911, 0.09999999999999951983 ) ) ;
#35888 = ORIENTED_EDGE ( 'NONE', *, *, #8470, .F. ) ;
#35889 = ORIENTED_EDGE ( 'NONE', *, *, #6996, .T. ) ;
#35890 = CYLINDRICAL_SURFACE ( 'NONE', #3580, 0.01500000000000005669 ) ;
#35891 = EDGE_CURVE ( 'NONE', #9404, #9161, #9977, .T. ) ;
#35892 = CARTESIAN_POINT ( 'NONE',  ( 0.2059853976207044468, -0.5424875326118652197, 0.4059703345962285548 ) ) ;
#35893 = AXIS2_PLACEMENT_3D ( 'NONE', #12021, #21289, #24578 ) ;
#35894 = CARTESIAN_POINT ( 'NONE',  ( -0.03171893264487379849, 0.2437375926088032885, -0.4645571062479579294 ) ) ;
#35895 = LINE ( 'NONE', #39375, #31108 ) ;
#35896 = FACE_OUTER_BOUND ( 'NONE', #10819, .T. ) ;
#35897 = DIRECTION ( 'NONE',  ( -7.771561172376107616E-16, 7.170354002788761615E-17, -1.000000000000000000 ) ) ;
#35898 = CARTESIAN_POINT ( 'NONE',  ( 0.6179353394495007423, -1.299228382567916285, 0.5682417262808777680 ) ) ;
#35899 = DIRECTION ( 'NONE',  ( 0.000000000000000000, 0.000000000000000000, -1.000000000000000000 ) ) ;
#35900 = LINE ( 'NONE', #26443, #4174 ) ;
#35901 = VECTOR ( 'NONE', #1824, 39.37007874015748143 ) ;
#35902 = CARTESIAN_POINT ( 'NONE',  ( 0.5026267308880598694, -1.652365288181674829, -0.5975130115846424284 ) ) ;
#35903 = VERTEX_POINT ( 'NONE', #28287 ) ;
#35904 = CARTESIAN_POINT ( 'NONE',  ( 0.4254380803681816481, -1.182152342139886514, 0.7222371136035362627 ) ) ;
#35905 = CARTESIAN_POINT ( 'NONE',  ( 0.7059656540691128246, -1.571716619208481935, -0.5155029497116575543 ) ) ;
#35906 = CARTESIAN_POINT ( 'NONE',  ( -0.05634115714581187234, -0.2655021207500423142, -0.3743162705049757344 ) ) ;
#35907 = APPROVAL_PERSON_ORGANIZATION ( #16705, #36670, #26368 ) ;
#35908 = ORIENTED_EDGE ( 'NONE', *, *, #8244, .F. ) ;
#35909 = CARTESIAN_POINT ( 'NONE',  ( -2.070754768975509919, -0.09959325338431655739, 0.09813923389047504720 ) ) ;
#35910 = DIRECTION ( 'NONE',  ( 1.000000000000000000, 2.410886674703102177E-13, -1.702189702233166186E-12 ) ) ;
#35911 = B_SPLINE_CURVE_WITH_KNOTS ( 'NONE', 3,
 ( #11442, #24007, #27678, #20916, #5245, #14724 ),
 .UNSPECIFIED., .F., .F.,
 ( 4, 2, 4 ),
 ( 0.000000000000000000, 0.0004951616201126960402, 0.0009903232402253920805 ),
 .UNSPECIFIED. ) ;
#35912 = ADVANCED_FACE ( 'NONE', ( #19249 ), #3394, .F. ) ;
#35913 = CARTESIAN_POINT ( 'NONE',  ( -2.070754768975509474, -0.09959325338431655739, 0.08500000000000142164 ) ) ;
#35914 = DIRECTION ( 'NONE',  ( 0.01455087615875041117, 0.9998941303973198913, 0.000000000000000000 ) ) ;
#35915 = CONICAL_SURFACE ( 'NONE', #21494, 0.01999999999999927530, 1.047197551196600962 ) ;
#35916 = CARTESIAN_POINT ( 'NONE',  ( 0.1955472856704882634, -1.153870291027489170, 0.7502753263242120108 ) ) ;
#35917 = ORIENTED_EDGE ( 'NONE', *, *, #6354, .F. ) ;
#35918 = DIRECTION ( 'NONE',  ( 0.8660512985181139101, 0.4999551463232363990, 0.000000000000000000 ) ) ;
#35919 = SHAPE_REPRESENTATION ( 'Pivot body rivet', ( #27819 ), #25262 ) ;
#35920 = CARTESIAN_POINT ( 'NONE',  ( 0.3688287100932481910, -1.620193688671676124, -0.3664956448573821746 ) ) ;
#35921 = CARTESIAN_POINT ( 'NONE',  ( 0.3791840186072914509, -1.765062149505512545, -0.4492540378293045644 ) ) ;
#35922 = DIRECTION ( 'NONE',  ( 1.000000000000000000, 1.188678714063518030E-15, 5.551115123125745108E-17 ) ) ;
#35923 = CARTESIAN_POINT ( 'NONE',  ( 0.4797981269282615147, -1.258694402034498561, 0.5894615839076718933 ) ) ;
#35925 = CARTESIAN_POINT ( 'NONE',  ( 0.3624061103390691096, -1.968824918581854932, -0.4968426515055719972 ) ) ;
#35924 = FACE_OUTER_BOUND ( 'NONE', #17562, .T. ) ;
#35926 = CARTESIAN_POINT ( 'NONE',  ( 0.5809658878212304867, -1.521239092202069321, -0.4539086719639525702 ) ) ;
#35927 = ORIENTED_EDGE ( 'NONE', *, *, #39382, .T. ) ;
#35928 = CARTESIAN_POINT ( 'NONE',  ( 0.4278413765848551042, -1.120299553241070001, -0.3830631589809550541 ) ) ;
#35929 = ORIENTED_EDGE ( 'NONE', *, *, #1902, .T. ) ;
#35930 = CARTESIAN_POINT ( 'NONE',  ( -0.1044460467970231704, -0.4741855622371820567, 0.3602693341844405150 ) ) ;
#35931 = CARTESIAN_POINT ( 'NONE',  ( 0.4148514316362570953, -1.579328421602780086, 0.6899777374673161656 ) ) ;
#35933 = CARTESIAN_POINT ( 'NONE',  ( 0.4480646913441767576, -1.099213350020603386, -0.6275147848854656374 ) ) ;
#35932 = CARTESIAN_POINT ( 'NONE',  ( 0.08965783709418552461, -0.5679113859805221542, 0.1161394655102304663 ) ) ;
#35934 = CARTESIAN_POINT ( 'NONE',  ( 0.1811099676929339986, -1.851639177593427998, -0.3465146202863149671 ) ) ;
#35935 = ADVANCED_FACE ( 'NONE', ( #28711 ), #27876, .F. ) ;
#35936 = ORIENTED_EDGE ( 'NONE', *, *, #26595, .F. ) ;
#35937 = AXIS2_PLACEMENT_3D ( 'NONE', #30333, #27268, #5029 ) ;
#35938 = EDGE_CURVE ( 'NONE', #20037, #23493, #3008, .T. ) ;
#35939 = DIRECTION ( 'NONE',  ( -0.4999999999999968359, 0.7308273574226419322, 0.4646411234949411884 ) ) ;
#35940 = CARTESIAN_POINT ( 'NONE',  ( 0.5745002926870975690, -1.499201178651017763, 0.5855314181424956521 ) ) ;
#35941 = VERTEX_POINT ( 'NONE', #25210 ) ;
#35942 = DIRECTION ( 'NONE',  ( 0.000000000000000000, 0.000000000000000000, -1.000000000000000000 ) ) ;
#35943 = CARTESIAN_POINT ( 'NONE',  ( 0.04946288932099940361, -0.4418470831553522049, 0.1805342557390068325 ) ) ;
#35944 = ADVANCED_FACE ( 'NONE', ( #19043 ), #37755, .F. ) ;
#35945 = CARTESIAN_POINT ( 'NONE',  ( 0.4040087334063396374, -1.746030677407556908, -0.4508910978256960300 ) ) ;
#35946 = CARTESIAN_POINT ( 'NONE',  ( 0.2170659164319594381, -1.241710086118905432, 0.4766412924577621002 ) ) ;
#35947 = DIRECTION ( 'NONE',  ( 0.4999551463232372317, -0.8660512985181133550, 0.000000000000000000 ) ) ;
#35948 = CARTESIAN_POINT ( 'NONE',  ( 0.08965528283357206141, -0.5631619445760863707, 0.1053715254844957705 ) ) ;
#35949 = CARTESIAN_POINT ( 'NONE',  ( 0.2256281918571345080, -0.6025195051315143102, 0.5087991896564706407 ) ) ;
#35950 = DIRECTION ( 'NONE',  ( 5.264498737790488644E-15, 0.7185945389471800615, 0.6954292836768448671 ) ) ;
#35951 = CARTESIAN_POINT ( 'NONE',  ( 0.08146858378016413882, -1.311453225872572403, 0.5631245198800998164 ) ) ;
#35952 = CARTESIAN_POINT ( 'NONE',  ( 0.5807707845827529969, -1.606612587616919496, -0.5663761035934116173 ) ) ;
#35953 = CARTESIAN_POINT ( 'NONE',  ( 0.03474878377840596305, 0.3591457335720743549, 0.3712550153170188216 ) ) ;
#35954 = LINE ( 'NONE', #20328, #24092 ) ;
#35955 = FACE_OUTER_BOUND ( 'NONE', #7967, .T. ) ;
#35956 = CARTESIAN_POINT ( 'NONE',  ( 0.1464731643940764827, -1.281649693683432734, 0.4243453113979892555 ) ) ;
#35957 = CARTESIAN_POINT ( 'NONE',  ( 0.3285791488923691106, -1.750622606776042423, 0.4882417262808776415 ) ) ;
#35958 = CARTESIAN_POINT ( 'NONE',  ( 0.5622555065282687226, -1.585093207106438973, -0.5030031773219529878 ) ) ;
#35959 = CARTESIAN_POINT ( 'NONE',  ( 6.300911482189779063E-14, -2.091072893779495345, -0.2612338433542039096 ) ) ;
#35960 = EDGE_CURVE ( 'NONE', #17597, #33435, #21304, .T. ) ;
#35961 = ADVANCED_FACE ( 'NONE', ( #12874 ), #33753, .T. ) ;
#35962 = DIRECTION ( 'NONE',  ( 0.3981087504120402465, 0.9173382270707809427, 0.000000000000000000 ) ) ;
#35963 = CARTESIAN_POINT ( 'NONE',  ( -0.04047161733260234984, -0.2415827978909579066, 0.4392067210493248997 ) ) ;
#35964 = ORIENTED_EDGE ( 'NONE', *, *, #27649, .F. ) ;
#35966 = ORIENTED_EDGE ( 'NONE', *, *, #33520, .F. ) ;
#35965 = B_SPLINE_SURFACE_WITH_KNOTS ( 'NONE', 5, 5, ( 
 ( #7587, #20357, #23042, #26528, #26140, #38848 ),
 ( #30019, #19943, #29410, #17658, #32477, #10475 ),
 ( #4495, #4303, #11092, #17057, #29811, #33092 ),
 ( #11286, #39068, #1849, #23652, #36173, #29603 ),
 ( #4900, #17466, #1445, #7982, #10894, #32878 ),
 ( #14364, #4688, #5101, #26739, #20558, #26928 ) ),
 .UNSPECIFIED., .F., .F., .F.,
 ( 6, 6 ),
 ( 6, 6 ),
 ( -6.477000000001651436, 6.477000000001639002 ),
 ( -2.080605796196421498, 4.396394203803585476 ),
 .UNSPECIFIED. ) ;
#35967 = CARTESIAN_POINT ( 'NONE',  ( 0.1060760254173120226, -1.412497056228485759, 0.5620039430078178633 ) ) ;
#35968 = CARTESIAN_POINT ( 'NONE',  ( 0.1437340355044557927, -1.283861693981850349, 0.4177417262808780229 ) ) ;
#35969 = ORIENTED_EDGE ( 'NONE', *, *, #22279, .F. ) ;
#35970 = DIRECTION ( 'NONE',  ( 1.000000000000000000, 7.857794173099924470E-32, 8.628166150854818811E-32 ) ) ;
#35971 = CARTESIAN_POINT ( 'NONE',  ( 0.6324675381817486119, -1.498808774185486525, -0.3951404225454540065 ) ) ;
#35972 = CARTESIAN_POINT ( 'NONE',  ( 0.4813074317656115819, -1.269335260105949770, 0.7818202548325017265 ) ) ;
#35974 = ORIENTED_EDGE ( 'NONE', *, *, #20545, .T. ) ;
#35973 = CARTESIAN_POINT ( 'NONE',  ( -0.1656815030311133141, 0.4813244629265694408, 0.1225468705240552458 ) ) ;
#35975 = CARTESIAN_POINT ( 'NONE',  ( 0.5031347454681565079, -1.114267567382387414, 0.6816460158534795033 ) ) ;
#35976 = CARTESIAN_POINT ( 'NONE',  ( 0.05634307799789379373, 0.4332460723641315403, -0.1515798417490722971 ) ) ;
#35977 = ORIENTED_EDGE ( 'NONE', *, *, #34676, .F. ) ;
#35978 = CARTESIAN_POINT ( 'NONE',  ( 0.5312361872299876664, -1.568664717035958001, -0.4868944820179721966 ) ) ;
#35979 = CARTESIAN_POINT ( 'NONE',  ( 0.03049314378765675612, -0.6057240897949897063, 0.3755447581365881082 ) ) ;
#35980 = CARTESIAN_POINT ( 'NONE',  ( 0.6912965087608118342, -1.498753872919812657, 0.4704591923298728218 ) ) ;
#35981 = CARTESIAN_POINT ( 'NONE',  ( -0.02000000000000000042, -2.183180860297908144, -0.4937760292030871079 ) ) ;
#35982 = CARTESIAN_POINT ( 'NONE',  ( 0.1991480113865258528, -2.054949600705707091, -0.6841806413415671972 ) ) ;
#35983 = ORIENTED_EDGE ( 'NONE', *, *, #38638, .F. ) ;
#35984 = FACE_OUTER_BOUND ( 'NONE', #32396, .T. ) ;
#35985 = B_SPLINE_CURVE_WITH_KNOTS ( 'NONE', 3,
 ( #33050, #30377, #1817, #4458, #2004, #10856 ),
 .UNSPECIFIED., .F., .F.,
 ( 4, 2, 4 ),
 ( 0.000000000000000000, 0.0004760980429614800708, 0.0009521960859229601417 ),
 .UNSPECIFIED. ) ;
#35986 = CARTESIAN_POINT ( 'NONE',  ( -0.02000000000000000042, -2.183180860297908144, -0.4937760292030871079 ) ) ;
#35987 = CARTESIAN_POINT ( 'NONE',  ( 0.3451269221721864899, -1.782955182391982696, 0.5182417262812423209 ) ) ;
#35988 = CARTESIAN_POINT ( 'NONE',  ( 0.3819577260478873026, -1.257944084395889783, 0.6070643466492523510 ) ) ;
#35989 = DIRECTION ( 'NONE',  ( -8.881784197001245421E-16, 2.361472542561082612E-16, -1.000000000000000000 ) ) ;
#35990 = EDGE_CURVE ( 'NONE', #10078, #11732, #35076, .T. ) ;
#35991 = CARTESIAN_POINT ( 'NONE',  ( 0.05083674528491994443, 0.04859289555129429894, -0.4711018118971372903 ) ) ;
#35992 = CARTESIAN_POINT ( 'NONE',  ( 0.1109049720484397705, -0.9286333197963668740, 0.1741076406654592235 ) ) ;
#35993 = CARTESIAN_POINT ( 'NONE',  ( 0.4234909963964844648, -1.082397635545747638, -0.5155029497116575543 ) ) ;
#35994 = DIRECTION ( 'NONE',  ( 0.000000000000000000, 0.000000000000000000, -1.000000000000000000 ) ) ;
#35995 = CARTESIAN_POINT ( 'NONE',  ( 0.4225253925792876730, -1.126620259732304064, 0.4991778718059378117 ) ) ;
#35996 = DIRECTION ( 'NONE',  ( 0.000000000000000000, 0.8063205929144886541, -0.5914787413272157846 ) ) ;
#35997 = DATE_TIME_ROLE ( 'creation_date' ) ;
#35998 = CARTESIAN_POINT ( 'NONE',  ( 0.0009472761255793785357, -0.9457358089336086460, 0.3226690514330370907 ) ) ;
#35999 = CARTESIAN_POINT ( 'NONE',  ( 0.1879272134313860199, -1.251865459589703633, -0.4009530412211869121 ) ) ;
#36000 = CIRCLE ( 'NONE', #20245, 0.1699999999999995404 ) ;
#36001 = DIRECTION ( 'NONE',  ( 0.000000000000000000, 0.000000000000000000, -1.000000000000000000 ) ) ;
#36002 = CARTESIAN_POINT ( 'NONE',  ( 0.4897592102757906130, -1.696528537887749932, -0.5984293649392183889 ) ) ;
#36003 = CARTESIAN_POINT ( 'NONE',  ( 0.5986518128144662221, -1.465474987463235790, 0.6057417262805031566 ) ) ;
#36004 = DIRECTION ( 'NONE',  ( 1.188678714063518227E-15, -1.000000000000000000, -3.263080277421930985E-16 ) ) ;
#36005 = DIRECTION ( 'NONE',  ( -0.8660512985181132439, -0.4999551463232375093, 0.000000000000000000 ) ) ;
#36006 = VERTEX_POINT ( 'NONE', #31190 ) ;
#36007 = ORIENTED_EDGE ( 'NONE', *, *, #20230, .T. ) ;
#36008 = CARTESIAN_POINT ( 'NONE',  ( 0.1766277944084894969, -0.4884173451829000867, 0.1430110528971104966 ) ) ;
#36009 = ORIENTED_EDGE ( 'NONE', *, *, #39683, .F. ) ;
#36010 = CARTESIAN_POINT ( 'NONE',  ( 0.4617378601122623105, -1.664140217285515089, -0.4140004630914397299 ) ) ;
#36011 = CARTESIAN_POINT ( 'NONE',  ( 0.6016038281123217146, -1.483041495014917333, 0.5656544979527685646 ) ) ;
#36012 = B_SPLINE_CURVE_WITH_KNOTS ( 'NONE', 3,
 ( #813, #9636, #19698, #25896 ),
 .UNSPECIFIED., .F., .F.,
 ( 4, 4 ),
 ( 0.005342362744812973255, 0.005869326880028568477 ),
 .UNSPECIFIED. ) ;
#36014 = VERTEX_POINT ( 'NONE', #40632 ) ;
#36013 = CARTESIAN_POINT ( 'NONE',  ( -0.0003981876585745823885, -0.7315818264868999554, -0.01661212268152491636 ) ) ;
#36015 = ORIENTED_EDGE ( 'NONE', *, *, #10524, .T. ) ;
#36016 = CARTESIAN_POINT ( 'NONE',  ( 0.3151595171820714136, -1.185655525176347647, 0.5568032880584220523 ) ) ;
#36017 = ORIENTED_EDGE ( 'NONE', *, *, #34401, .F. ) ;
#36018 = CARTESIAN_POINT ( 'NONE',  ( -0.0002811468384461541072, -0.6516915277880520607, 0.4786751619668931368 ) ) ;
#36020 = FACE_OUTER_BOUND ( 'NONE', #35225, .T. ) ;
#36019 = DIRECTION ( 'NONE',  ( 0.8660512985181134660, 0.4999551463232372317, 0.000000000000000000 ) ) ;
#36021 = CARTESIAN_POINT ( 'NONE',  ( 0.6213189662415743442, -1.606914084853001246, -0.4645767070828071277 ) ) ;
#36022 = CONTEXT_DEPENDENT_SHAPE_REPRESENTATION ( #11655, #39020 ) ;
#36023 = CARTESIAN_POINT ( 'NONE',  ( -0.2746410161513782033, -2.183180860297908144, -0.9552969701112735690 ) ) ;
#36025 = ORIENTED_EDGE ( 'NONE', *, *, #30408, .F. ) ;
#36024 = ORIENTED_EDGE ( 'NONE', *, *, #2430, .F. ) ;
#36026 = B_SPLINE_CURVE_WITH_KNOTS ( 'NONE', 3,
 ( #38267, #12784, #1085, #25962, #32107, #7392, #16677, #3521, #35205, #9885, #29229, #16284, #22459, #32295, #37882, #34985, #16472, #6793, #19377, #9697, #31911, #7007, #3730, #10317, #3914, #29014 ),
 .UNSPECIFIED., .F., .F.,
 ( 4, 2, 2, 2, 2, 2, 2, 2, 2, 2, 2, 2, 4 ),
 ( 0.000000000000000000, 0.0009027245942062626840, 0.001805449188412525368, 0.002708173782618787835, 0.003610898376825050736, 0.004513622971031313637, 0.005416347565237575670, 0.007221796753650082390, 0.009027245942062589110, 0.01083269513047509409, 0.01263814431888760081, 0.01354086891309385157, 0.01444359350730010406 ),
 .UNSPECIFIED. ) ;
#36027 = CARTESIAN_POINT ( 'NONE',  ( 0.1462251280849438395, -0.8510050163060884909, 0.5114821326872159846 ) ) ;
#36028 = CARTESIAN_POINT ( 'NONE',  ( 0.07520564851098779369, -1.153270212343224133, 0.7613220868928463059 ) ) ;
#36029 = CARTESIAN_POINT ( 'NONE',  ( 0.08994178283652765060, -0.5440620458595929465, 0.1575062128599965250 ) ) ;
#36030 = CARTESIAN_POINT ( 'NONE',  ( 0.4876370588746136159, -1.406030492629142259, 0.8039593740868691274 ) ) ;
#36031 = CARTESIAN_POINT ( 'NONE',  ( 0.03693592009331247289, -1.103750244955626236, 0.6430833370955907347 ) ) ;
#36032 = CARTESIAN_POINT ( 'NONE',  ( 0.4699303087857425454, -1.591526288972971992, -0.4356248681750835017 ) ) ;
#36033 = LINE ( 'NONE', #39514, #152 ) ;
#36034 = CARTESIAN_POINT ( 'NONE',  ( 0.4109940520397017960, -1.749134648671465619, -0.4344985177731692239 ) ) ;
#36035 = CARTESIAN_POINT ( 'NONE',  ( 0.3656312763845015468, -1.616885411836818998, -0.3263777939557699903 ) ) ;
#36036 = EDGE_CURVE ( 'NONE', #5749, #13059, #28714, .T. ) ;
#36037 = FACE_OUTER_BOUND ( 'NONE', #12056, .T. ) ;
#36038 = EDGE_CURVE ( 'NONE', #28752, #29747, #40440, .T. ) ;
#36039 = CARTESIAN_POINT ( 'NONE',  ( 0.1999999999999789724, -2.183180860297921466, -0.7137760292030871367 ) ) ;
#36040 = CARTESIAN_POINT ( 'NONE',  ( -0.1210148435730035998, -0.5061394519556905447, 0.1438724812234790928 ) ) ;
#36041 = CARTESIAN_POINT ( 'NONE',  ( 0.01140463913857075844, -0.9214766123526784147, 0.03400881840692861202 ) ) ;
#36042 = DIRECTION ( 'NONE',  ( 0.8660512985181133550, 0.4999551463232372872, 0.000000000000000000 ) ) ;
#36043 = SHAPE_REPRESENTATION_RELATIONSHIP ( 'NONE' , 'NONE' ,  #24383, #5371 ) ;
#36044 = EDGE_CURVE ( 'NONE', #19627, #556, #21938, .T. ) ;
#36045 = CARTESIAN_POINT ( 'NONE',  ( 0.006363676076506938339, -0.8374434632259925015, 0.09472199571917780392 ) ) ;
#36046 = DIRECTION ( 'NONE',  ( 0.000000000000000000, 0.000000000000000000, -1.000000000000000000 ) ) ;
#36047 = EDGE_CURVE ( 'NONE', #38179, #24800, #39983, .T. ) ;
#36048 = CARTESIAN_POINT ( 'NONE',  ( -0.001733054258001554731, -0.9004704535694999512, 0.2409329515054920989 ) ) ;
#36049 = CARTESIAN_POINT ( 'NONE',  ( 0.4925986438152862856, -1.082524672201789828, 0.5763763218629267548 ) ) ;
#36050 = COORDINATED_UNIVERSAL_TIME_OFFSET ( 0, 0, .AHEAD. ) ;
#36051 = CARTESIAN_POINT ( 'NONE',  ( 0.2803613453953150980, -0.7205873319272890765, 0.6521004353453685454 ) ) ;
#36052 = CARTESIAN_POINT ( 'NONE',  ( 0.4186432780919981389, -1.612034538517056692, -0.6668481824684691084 ) ) ;
#36053 = DIRECTION ( 'NONE',  ( 1.060606950627616773E-16, 6.122684696619993730E-17, 1.000000000000000000 ) ) ;
#36054 = EDGE_CURVE ( 'NONE', #30626, #33071, #5540, .T. ) ;
#36055 = ORIENTED_EDGE ( 'NONE', *, *, #32777, .T. ) ;
#36056 = CARTESIAN_POINT ( 'NONE',  ( 0.1739430406544926755, -1.555536796503983243, -0.6758258725061466743 ) ) ;
#36057 = APPLIED_PERSON_AND_ORGANIZATION_ASSIGNMENT ( #14694, #1411, ( #11166 ) ) ;
#36058 = CARTESIAN_POINT ( 'NONE',  ( 0.01371903225206740247, -0.6635012362921914875, 0.4961661892038754518 ) ) ;
#36059 = CARTESIAN_POINT ( 'NONE',  ( -0.2746410161513776482, -3.672249662662566472, -0.1880352225538197142 ) ) ;
#36061 = ORIENTED_EDGE ( 'NONE', *, *, #14426, .F. ) ;
#36060 = FACE_OUTER_BOUND ( 'NONE', #27081, .T. ) ;
#36062 = CARTESIAN_POINT ( 'NONE',  ( 0.06843411546424661707, -1.327640554429453168, 0.5682417262808774350 ) ) ;
#36063 = CARTESIAN_POINT ( 'NONE',  ( 0.4605766076693431632, -1.054687064863744750, 0.7953974510635947182 ) ) ;
#36065 = ORIENTED_EDGE ( 'NONE', *, *, #22000, .F. ) ;
#36064 = ORIENTED_EDGE ( 'NONE', *, *, #29485, .T. ) ;
#36066 = CARTESIAN_POINT ( 'NONE',  ( 0.08761651290939830028, -1.378853951282039469, -0.6937690615011236073 ) ) ;
#36067 = ORIENTED_EDGE ( 'NONE', *, *, #21836, .F. ) ;
#36068 = CARTESIAN_POINT ( 'NONE',  ( 0.3569902980463470765, -1.891667118059767283, -0.4992937296425578042 ) ) ;
#36069 = CARTESIAN_POINT ( 'NONE',  ( 0.4575915118593487652, -1.228153751895449952, 0.6022438500237607961 ) ) ;
#36070 = B_SPLINE_CURVE_WITH_KNOTS ( 'NONE', 3,
 ( #31265, #21184, #3079, #28170, #34, #31456 ),
 .UNSPECIFIED., .F., .F.,
 ( 4, 2, 4 ),
 ( 0.002342563885389197919, 0.002942418546801120038, 0.003542273208213042156 ),
 .UNSPECIFIED. ) ;
#36071 = CARTESIAN_POINT ( 'NONE',  ( -0.05076541221973576712, 0.4633004642377308580, -0.09914728473419241739 ) ) ;
#36072 = ORIENTED_EDGE ( 'NONE', *, *, #36044, .T. ) ;
#36073 = CARTESIAN_POINT ( 'NONE',  ( 0.6055916563817613785, -1.479479184092913790, 0.5526975506195442867 ) ) ;
#36074 = EDGE_CURVE ( 'NONE', #24795, #31373, #23336, .T. ) ;
#36075 = CARTESIAN_POINT ( 'NONE',  ( 0.2731210195084670111, -0.9705246840574025535, 0.7137744440085082021 ) ) ;
#36076 = CARTESIAN_POINT ( 'NONE',  ( 0.2855206935027220227, -1.611758747868883290, 0.9420719997129571865 ) ) ;
#36077 = CARTESIAN_POINT ( 'NONE',  ( 0.09770673769026198829, -0.5470910535863472424, 0.1715607505604543614 ) ) ;
#36079 = CARTESIAN_POINT ( 'NONE',  ( 0.3006692146602689131, -1.655694840352218034, 0.5887342810090384626 ) ) ;
#36078 = CARTESIAN_POINT ( 'NONE',  ( 0.1356501467668746463, -1.176154491973367078, 0.9233203751264872361 ) ) ;
#36080 = CARTESIAN_POINT ( 'NONE',  ( 0.3816210699381897276, -1.147921404532277645, 0.5682417262808778791 ) ) ;
#36081 = ORIENTED_EDGE ( 'NONE', *, *, #23626, .F. ) ;
#36082 = ORIENTED_EDGE ( 'NONE', *, *, #29388, .T. ) ;
#36083 = DIRECTION ( 'NONE',  ( 7.771561172376107616E-16, -7.170354002788761615E-17, 1.000000000000000000 ) ) ;
#36084 = CARTESIAN_POINT ( 'NONE',  ( 0.2007258555610571815, -0.5966229082202755274, 0.3439381669633011507 ) ) ;
#36085 = DIRECTION ( 'NONE',  ( 0.000000000000000000, 0.000000000000000000, -1.000000000000000000 ) ) ;
#36086 = EDGE_CURVE ( 'NONE', #28931, #7674, #6596, .T. ) ;
#36087 = CARTESIAN_POINT ( 'NONE',  ( -0.04140212552917923311, -0.4524976860274254054, -0.1292082980168287876 ) ) ;
#36088 = EDGE_CURVE ( 'NONE', #35941, #12958, #10163, .T. ) ;
#36089 = CARTESIAN_POINT ( 'NONE',  ( 0.07098271911918006827, -1.324513431496047611, 0.5012323767505566519 ) ) ;
#36090 = EDGE_CURVE ( 'NONE', #2531, #4571, #10815, .T. ) ;
#36091 = CARTESIAN_POINT ( 'NONE',  ( 0.1031893334089009490, -1.411522619511051513, 0.5048512516234096026 ) ) ;
#36092 = CARTESIAN_POINT ( 'NONE',  ( 0.6181559592477333664, -1.299230524387357866, 0.5730398182776358373 ) ) ;
#36093 = CARTESIAN_POINT ( 'NONE',  ( -0.1157923916715204865, -0.5295015842444287246, 0.1380392329925466954 ) ) ;
#36094 = CARTESIAN_POINT ( 'NONE',  ( 0.01548846960706656145, 0.5203207976468126050, -0.08861466064782015650 ) ) ;
#36095 = CARTESIAN_POINT ( 'NONE',  ( 0.05999999999999990757, 0.000000000000000000, 0.4614999999999880864 ) ) ;
#36096 = CARTESIAN_POINT ( 'NONE',  ( 0.4578775569534166423, -1.222985555920403256, 0.6583285616417049457 ) ) ;
#36097 = CARTESIAN_POINT ( 'NONE',  ( -0.03309059653085742736, -0.08822156176787991633, -0.5132714489379855971 ) ) ;
#36098 = CARTESIAN_POINT ( 'NONE',  ( -0.04211812644076833728, -0.2825523317586257077, -0.3743635450761886863 ) ) ;
#36099 = EDGE_CURVE ( 'NONE', #23099, #13465, #21994, .T. ) ;
#36100 = ORIENTED_EDGE ( 'NONE', *, *, #628, .T. ) ;
#36101 = CARTESIAN_POINT ( 'NONE',  ( -0.2746410161513779258, -3.985676108854518507, -0.7623095129438225426 ) ) ;
#36102 = DIRECTION ( 'NONE',  ( -1.000000000000000000, -9.860761315262660705E-32, -5.551115123125790098E-17 ) ) ;
#36103 = CARTESIAN_POINT ( 'NONE',  ( 0.4099814236516951538, -1.131125796475745737, 0.5236811888078589661 ) ) ;
#36104 = CARTESIAN_POINT ( 'NONE',  ( 0.03817455972094940114, -0.8539075176413860602, 0.3579164544551949878 ) ) ;
#36105 = ORIENTED_EDGE ( 'NONE', *, *, #34894, .T. ) ;
#36106 = DIRECTION ( 'NONE',  ( -1.252096997096119587E-14, 1.000000000000000000, -2.162712994984206616E-14 ) ) ;
#36107 = CYLINDRICAL_SURFACE ( 'NONE', #9880, 0.2000000000000000111 ) ;
#36108 = DIRECTION ( 'NONE',  ( 1.000000000000000000, -0.000000000000000000, -0.000000000000000000 ) ) ;
#36109 = CYLINDRICAL_SURFACE ( 'NONE', #13408, 1.991674066779353547 ) ;
#36110 = CARTESIAN_POINT ( 'NONE',  ( 0.4760168417944102837, -1.251435095516215235, 0.6187594006579745232 ) ) ;
#36112 = CARTESIAN_POINT ( 'NONE',  ( 0.5382307432915078849, -1.161159458769174257, 0.5682417262808779901 ) ) ;
#36111 = CARTESIAN_POINT ( 'NONE',  ( 0.5640992009001688512, -1.512213347522166185, 0.5182417262812423209 ) ) ;
#36113 = CARTESIAN_POINT ( 'NONE',  ( 0.2042269006659602204, -0.9243050108670398668, 0.3357924985444922794 ) ) ;
#36114 = EDGE_LOOP ( 'NONE', ( #414, #25922 ) ) ;
#36115 = CARTESIAN_POINT ( 'NONE',  ( 0.5360540090424209536, -1.620675673019976504, 0.4182417262808776903 ) ) ;
#36116 = EDGE_LOOP ( 'NONE', ( #16651, #4664 ) ) ;
#36117 = DIRECTION ( 'NONE',  ( -1.000000000000000000, -0.000000000000000000, -0.000000000000000000 ) ) ;
#36118 = CARTESIAN_POINT ( 'NONE',  ( 0.4138156062724669959, -1.589593685339665941, 0.5765124207693830272 ) ) ;
#36120 = CARTESIAN_POINT ( 'NONE',  ( 0.1957193385055910895, -0.7828756236076227504, 0.3030586162759186242 ) ) ;
#36119 = CARTESIAN_POINT ( 'NONE',  ( 0.08939090954650172338, -0.5761542031603253955, 0.09289087833756660972 ) ) ;
#36121 = CARTESIAN_POINT ( 'NONE',  ( 0.1785188695711833751, -1.263798542596899610, 0.4993478297628262119 ) ) ;
#36122 = ORIENTED_EDGE ( 'NONE', *, *, #21854, .T. ) ;
#36123 = VERTEX_POINT ( 'NONE', #16966 ) ;
#36124 = DIRECTION ( 'NONE',  ( -1.000000000000000000, -2.341930812374887555E-31, 1.664003471950578127E-31 ) ) ;
#36125 = CARTESIAN_POINT ( 'NONE',  ( 0.1192180282511240558, -0.5521284355774265240, 0.1795391081213666140 ) ) ;
#36126 = ORIENTED_EDGE ( 'NONE', *, *, #9212, .T. ) ;
#36127 = CARTESIAN_POINT ( 'NONE',  ( 0.02881195911414203767, -0.4889334074056480017, 0.09563129189200124392 ) ) ;
#36128 = ADVANCED_FACE ( 'NONE', ( #10578, #38563 ), #22950, .F. ) ;
#36129 = CARTESIAN_POINT ( 'NONE',  ( 0.6109174031409076999, -1.589286328436636975, 0.4250233519115255154 ) ) ;
#36130 = CARTESIAN_POINT ( 'NONE',  ( 0.1086196161304056745, -1.292942797799375265, 0.4408190352604076656 ) ) ;
#36131 = EDGE_CURVE ( 'NONE', #18976, #20310, #343, .T. ) ;
#36132 = AXIS2_PLACEMENT_3D ( 'NONE', #2062, #4933, #17290 ) ;
#36133 = DIRECTION ( 'NONE',  ( -0.8304108868527259046, -0.5068230121326142701, 0.2314048257260277464 ) ) ;
#36134 = CARTESIAN_POINT ( 'NONE',  ( 0.3902882956839560658, -1.753951228373453519, -0.4725945316380958383 ) ) ;
#36135 = CARTESIAN_POINT ( 'NONE',  ( 0.7062706752423565382, -1.445327451526715823, 0.7203384021836691797 ) ) ;
#36136 = CONICAL_SURFACE ( 'NONE', #22361, 0.1400000000000004297, 1.047197551196599630 ) ;
#36137 = CARTESIAN_POINT ( 'NONE',  ( 0.07734919244711804809, -1.330214924570791490, 0.4791524173686232957 ) ) ;
#36138 = CARTESIAN_POINT ( 'NONE',  ( 0.03664605387828104993, -0.2484618661253095717, -0.4118464167359250361 ) ) ;
#36139 = CARTESIAN_POINT ( 'NONE',  ( 0.6182991044115986323, -1.621655261782950941, -0.4927229840283234297 ) ) ;
#36140 = CARTESIAN_POINT ( 'NONE',  ( 0.2200771146567370995, -1.355300809693532837, 0.4882188858632743877 ) ) ;
#36141 = CARTESIAN_POINT ( 'NONE',  ( 0.6205175308492241193, -1.587685600206998338, 0.6075176836741390529 ) ) ;
#36142 = LINE ( 'NONE', #7954, #21202 ) ;
#36143 = CARTESIAN_POINT ( 'NONE',  ( -0.05634301242525831949, 0.4332457820339853383, -0.1515812001271586162 ) ) ;
#36144 =( BOUNDED_SURFACE ( )  B_SPLINE_SURFACE ( 3, 2, ( 
 ( #6256, #8524, #27471 ),
 ( #34230, #24976, #5832 ),
 ( #9332, #34031, #37510 ),
 ( #5646, #6040, #18608 ),
 ( #17992, #2981, #24801 ),
 ( #36914, #37127, #15531 ),
 ( #15319, #21092, #37320 ),
 ( #18199, #27875, #21696 ),
 ( #27665, #30749, #33617 ),
 ( #21516, #30946, #21913 ),
 ( #39806, #36714, #8726 ),
 ( #18393, #5427, #2373 ),
 ( #34439, #12238, #14916 ),
 ( #2569, #24592, #8940 ),
 ( #15104, #2770, #31167 ),
 ( #39996, #28083, #40611 ),
 ( #12427, #11817, #21303 ),
 ( #9129, #33844, #24191 ),
 ( #18826, #31370, #24378 ),
 ( #40197, #3175, #11633 ),
 ( #12031, #40413, #15716 ),
 ( #30853, #18508, #31061 ) ),
 .UNSPECIFIED., .F., .F., .F. ) 
 B_SPLINE_SURFACE_WITH_KNOTS ( ( 4, 2, 2, 2, 2, 2, 2, 2, 2, 2, 4 ),
 ( 3, 3 ),
 ( 0.002013519961495851326, 0.002780892266055759107, 0.003548264570615667322, 0.004315636875175575538, 0.004699323027455529211, 0.005083009179735483753, 0.005466695332015438294, 0.005850381484295391968, 0.006617753788855299316, 0.007385126093415207531, 0.008152498397975115746 ),
 ( 0.000000000000000000, 1.000000000000000000 ),
 .UNSPECIFIED. ) 
 GEOMETRIC_REPRESENTATION_ITEM ( )  RATIONAL_B_SPLINE_SURFACE ( (
 ( 1.000000000000000000, 0.7283825911960393196, 1.000000000000000000),
 ( 1.000000000000000000, 0.7404375345927475260, 1.000000000000000000),
 ( 1.000000000000000000, 0.7521483142435417824, 1.000000000000000000),
 ( 1.000000000000000000, 0.7744460733777035477, 1.000000000000000000),
 ( 1.000000000000000000, 0.7845612039379376013, 1.000000000000000000),
 ( 1.000000000000000000, 0.8022035258264773594, 1.000000000000000000),
 ( 1.000000000000000000, 0.8093965293320570797, 1.000000000000000000),
 ( 1.000000000000000000, 0.8169028692726044705, 1.000000000000000000),
 ( 1.000000000000000000, 0.8188329634862745454, 1.000000000000000000),
 ( 1.000000000000000000, 0.8214004505364636000, 1.000000000000000000),
 ( 1.000000000000000000, 0.8220602406261303674, 1.000000000000000000),
 ( 1.000000000000000000, 0.8220736605435321476, 1.000000000000000000),
 ( 1.000000000000000000, 0.8214126668415425714, 1.000000000000000000),
 ( 1.000000000000000000, 0.8188520474558570461, 1.000000000000000000),
 ( 1.000000000000000000, 0.8169545908333386564, 1.000000000000000000),
 ( 1.000000000000000000, 0.8094771004221671395, 1.000000000000000000),
 ( 1.000000000000000000, 0.8022723753809033465, 1.000000000000000000),
 ( 1.000000000000000000, 0.7845733350635970549, 1.000000000000000000),
 ( 1.000000000000000000, 0.7744472902495431743, 1.000000000000000000),
 ( 1.000000000000000000, 0.7522916829161283570, 1.000000000000000000),
 ( 1.000000000000000000, 0.7403553004667449144, 1.000000000000000000),
 ( 1.000000000000000000, 0.7283825911960383204, 1.000000000000000000) ) ) 
 REPRESENTATION_ITEM ( '' )  SURFACE ( )  );
#36145 = EDGE_CURVE ( 'NONE', #5313, #15674, #27241, .T. ) ;
#36146 = CARTESIAN_POINT ( 'NONE',  ( 0.002083146443013472390, -0.4777046557262296100, 0.1109577558998209867 ) ) ;
#36147 = CARTESIAN_POINT ( 'NONE',  ( 0.5986005277559497406, -1.542134511451966672, -0.4467108566020089877 ) ) ;
#36148 = ADVANCED_FACE ( 'NONE', ( #29710 ), #35890, .T. ) ;
#36149 = CYLINDRICAL_SURFACE ( 'NONE', #36343, 0.07499999999999977518 ) ;
#36150 = CARTESIAN_POINT ( 'NONE',  ( 0.5926747167100170355, -1.589032888346250338, 0.4182417262808776903 ) ) ;
#36151 = CARTESIAN_POINT ( 'NONE',  ( -0.04139678531769583336, -0.2901741387554249707, 0.3704845587920869154 ) ) ;
#36152 = EDGE_CURVE ( 'NONE', #354, #7026, #30314, .T. ) ;
#36153 = ORIENTED_EDGE ( 'NONE', *, *, #5663, .F. ) ;
#36154 = VERTEX_POINT ( 'NONE', #24172 ) ;
#36155 = DIRECTION ( 'NONE',  ( 0.8660512985181133550, 0.4999551463232370652, 0.000000000000000000 ) ) ;
#36156 = EDGE_CURVE ( 'NONE', #29592, #34829, #10481, .T. ) ;
#36157 = CARTESIAN_POINT ( 'NONE',  ( 0.3206535937437295369, -1.182295409031864697, 0.3157417262808777658 ) ) ;
#36158 = ORIENTED_EDGE ( 'NONE', *, *, #33145, .T. ) ;
#36159 = CARTESIAN_POINT ( 'NONE',  ( 0.01548846960707511190, -0.2306506793134033284, 0.4716198300880330985 ) ) ;
#36160 = CARTESIAN_POINT ( 'NONE',  ( -0.04582713223189560647, 0.3361263728083093150, -0.3523178389613189077 ) ) ;
#36161 = CARTESIAN_POINT ( 'NONE',  ( 0.5542078555708851439, -1.385725491393886788, 0.6184366861635991475 ) ) ;
#36162 = CONICAL_SURFACE ( 'NONE', #7243, 0.1400000000000012623, 1.047197551196601850 ) ;
#36164 = ORIENTED_EDGE ( 'NONE', *, *, #3904, .F. ) ;
#36163 = CARTESIAN_POINT ( 'NONE',  ( -0.1638606670177130409, 0.5090623078239890908, 0.1147396705136482370 ) ) ;
#36165 = CARTESIAN_POINT ( 'NONE',  ( 0.4873263706924592098, -1.095012774062378513, 0.6880473194844076712 ) ) ;
#36166 = DIRECTION ( 'NONE',  ( -1.000000000000000000, -2.280301054154495132E-31, 1.664003471950577689E-31 ) ) ;
#36167 = ORIENTED_EDGE ( 'NONE', *, *, #28582, .F. ) ;
#36168 = FACE_OUTER_BOUND ( 'NONE', #27568, .T. ) ;
#36169 = VECTOR ( 'NONE', #5324, 39.37007874015748143 ) ;
#36170 = CARTESIAN_POINT ( 'NONE',  ( 0.2469025657576066068, -1.386664304572385431, 0.9158093811668733819 ) ) ;
#36172 = CARTESIAN_POINT ( 'NONE',  ( 0.4584717390208091770, -1.703043547193807017, -0.5155029497116575543 ) ) ;
#36171 = CARTESIAN_POINT ( 'NONE',  ( 0.6692142533638006929, -1.524953862027760287, 0.4346820991015040159 ) ) ;
#36173 = CARTESIAN_POINT ( 'NONE',  ( 0.3207148961678939481, -1.182401600646133089, 0.3667417262808778111 ) ) ;
#36174 = AXIS2_PLACEMENT_3D ( 'NONE', #6109, #25050, #18676 ) ;
#36175 = PLANE ( 'NONE',  #29035 ) ;
#36176 = ORIENTED_EDGE ( 'NONE', *, *, #3045, .T. ) ;
#36177 = CARTESIAN_POINT ( 'NONE',  ( -0.2746410161513779258, -1.874946189051298617, -0.07947534077849530143 ) ) ;
#36178 = CARTESIAN_POINT ( 'NONE',  ( 0.1536596445529309907, -1.277574755431482023, 0.4245438548657214928 ) ) ;
#36179 = DIRECTION ( 'NONE',  ( 1.848892746611741821E-31, 0.8983234858820565716, -0.4393346272634452432 ) ) ;
#36180 = CARTESIAN_POINT ( 'NONE',  ( 0.3010285249158310417, -1.239940644847210116, 0.6985209647544882161 ) ) ;
#36181 = CARTESIAN_POINT ( 'NONE',  ( -2.115421433687637455E-14, -2.107936428766274073, -0.7005084057759867200 ) ) ;
#36182 = EDGE_CURVE ( 'NONE', #16165, #5331, #13455, .T. ) ;
#36183 = CARTESIAN_POINT ( 'NONE',  ( 0.05562150110511221435, 0.02029635476683638168, -0.4604536315446552397 ) ) ;
#36184 = ADVANCED_FACE ( 'NONE', ( #37098 ), #8913, .F. ) ;
#36185 = FACE_OUTER_BOUND ( 'NONE', #20250, .T. ) ;
#36186 = CARTESIAN_POINT ( 'NONE',  ( -0.1212602505242198897, -0.5073146173415499227, 0.1498414178977029720 ) ) ;
#36187 = CARTESIAN_POINT ( 'NONE',  ( 0.3503153873832512422, -1.166694168676842391, 0.4149758699348384816 ) ) ;
#36188 = CARTESIAN_POINT ( 'NONE',  ( 0.6589248909250595698, -1.495897505467806310, 0.4182417262808776903 ) ) ;
#36189 = LINE ( 'NONE', #19961, #20683 ) ;
#36190 = APPLICATION_PROTOCOL_DEFINITION ( 'international standard', 'automotive_design', 2000, #40545 ) ;
#36191 = CIRCLE ( 'NONE', #22414, 0.01500000000000005843 ) ;
#36192 = CARTESIAN_POINT ( 'NONE',  ( 0.06465794909978246630, -1.338646149722257483, 0.5860318141376208434 ) ) ;
#36193 = CARTESIAN_POINT ( 'NONE',  ( 0.3848921974812524738, -1.145728365548885241, 0.5552085920578813116 ) ) ;
#36194 = CYLINDRICAL_SURFACE ( 'NONE', #27779, 0.2200000000000000566 ) ;
#36195 = TOROIDAL_SURFACE ( 'NONE', #39480, 0.5250000000000000222, 0.01499999999999999944 ) ;
#36196 = VECTOR ( 'NONE', #34787, 39.37007874015748143 ) ;
#36197 = CARTESIAN_POINT ( 'NONE',  ( 2.535788866453828974E-05, -0.4479327805637732252, 0.04122704326806578279 ) ) ;
#36198 = CARTESIAN_POINT ( 'NONE',  ( 0.3626185512632494334, -1.769924452066289122, -0.5899438298025727612 ) ) ;
#36199 = AXIS2_PLACEMENT_3D ( 'NONE', #29557, #32834, #26700 ) ;
#36200 = DIRECTION ( 'NONE',  ( -1.000000000000000000, -2.280301054154495132E-31, 1.664003471950577689E-31 ) ) ;
#36201 = DIRECTION ( 'NONE',  ( 0.9378410757839559242, 0.1072489841977647962, -0.3300784330442385062 ) ) ;
#36202 = ORIENTED_EDGE ( 'NONE', *, *, #26845, .T. ) ;
#36203 = ORIENTED_EDGE ( 'NONE', *, *, #20600, .T. ) ;
#36204 = CARTESIAN_POINT ( 'NONE',  ( 0.1746424574112480366, -0.5322842895853476808, 0.2164681121527878838 ) ) ;
#36205 = ORIENTED_EDGE ( 'NONE', *, *, #33826, .T. ) ;
#36206 = CARTESIAN_POINT ( 'NONE',  ( -0.08000000000000000167, -1.712002775963388235, -0.1631032362481502351 ) ) ;
#36208 = ORIENTED_EDGE ( 'NONE', *, *, #29637, .F. ) ;
#36207 = CARTESIAN_POINT ( 'NONE',  ( 0.5306537665242748725, -1.384128856765673987, 0.7879015558401659680 ) ) ;
#36210 = ORIENTED_EDGE ( 'NONE', *, *, #15696, .F. ) ;
#36209 = CARTESIAN_POINT ( 'NONE',  ( -0.001735234428706586285, -0.8394157820079461985, 0.07324090056792484371 ) ) ;
#36211 = ORIENTED_EDGE ( 'NONE', *, *, #4697, .T. ) ;
#36212 = CARTESIAN_POINT ( 'NONE',  ( 0.1559516411203765995, -0.6020992908152480450, 0.5335147605418883998 ) ) ;
#36213 = CARTESIAN_POINT ( 'NONE',  ( 0.04547705972580577682, -0.8635874790222509700, 0.7385780690550703964 ) ) ;
#36215 = CARTESIAN_POINT ( 'NONE',  ( 0.1327588654869316098, -1.278667161109435790, 0.6047653525011950082 ) ) ;
#36214 = CARTESIAN_POINT ( 'NONE',  ( -2.070754768975504589, -0.09959325338431362917, 0.3599999999999976552 ) ) ;
#36216 = CYLINDRICAL_SURFACE ( 'NONE', #8205, 0.03000000000000029379 ) ;
#36217 = ITEM_DEFINED_TRANSFORMATION ( 'NONE', 'NONE', #33115,  #27819 ) ;
#36218 = TOROIDAL_SURFACE ( 'NONE', #764, 0.08830708661417323302, 0.01499999999999999944 ) ;
#36219 = CARTESIAN_POINT ( 'NONE',  ( -0.1688017273025779752, 0.4914669153062978801, 0.3250764289764314086 ) ) ;
#36221 = ORIENTED_EDGE ( 'NONE', *, *, #38921, .F. ) ;
#36220 = ORIENTED_EDGE ( 'NONE', *, *, #27386, .T. ) ;
#36222 = AXIS2_PLACEMENT_3D ( 'NONE', #12709, #38210, #37814 ) ;
#36223 = DIRECTION ( 'NONE',  ( 0.000000000000000000, 0.000000000000000000, 1.000000000000000000 ) ) ;
#36224 = CARTESIAN_POINT ( 'NONE',  ( 0.02818252482944432619, -0.9358868228192540606, 0.6083748332521794477 ) ) ;
#36225 = CARTESIAN_POINT ( 'NONE',  ( 0.09604050016782572641, -0.6082561981476365398, 0.2968782915989965354 ) ) ;
#36226 = AXIS2_PLACEMENT_3D ( 'NONE', #17749, #2130, #14665 ) ;
#36227 = CARTESIAN_POINT ( 'NONE',  ( 0.1162496453231300075, -0.5482924977647862796, 0.1535821627971732661 ) ) ;
#36228 = CARTESIAN_POINT ( 'NONE',  ( 0.04800852669519790200, -1.175821727638011405, 0.6650279943451450348 ) ) ;
#36229 = DIRECTION ( 'NONE',  ( -1.000000000000000000, -7.857794173099924470E-32, -8.628166150854818811E-32 ) ) ;
#36230 = CARTESIAN_POINT ( 'NONE',  ( 0.06581764578086063411, -1.340728352476672658, 0.5449258910593480776 ) ) ;
#36231 = AXIS2_PLACEMENT_3D ( 'NONE', #16376, #18658, #25453 ) ;
#36232 = CARTESIAN_POINT ( 'NONE',  ( -0.2746410161513770931, -2.599675038826658735, -0.8213992999509311943 ) ) ;
#36233 = CARTESIAN_POINT ( 'NONE',  ( 0.3921416614852478721, -1.728153360793264870, 0.4267968442986774802 ) ) ;
#36234 = CARTESIAN_POINT ( 'NONE',  ( 0.6540709664215760277, -1.593060928864740156, 0.5182417262812423209 ) ) ;
#36235 = CARTESIAN_POINT ( 'NONE',  ( 0.06923712653936904549, -0.5400029222721455247, 0.1457185332388703236 ) ) ;
#36236 = CARTESIAN_POINT ( 'NONE',  ( 0.3999999999999788169, -2.097675824466504135, -0.4688691127277798687 ) ) ;
#36237 = CARTESIAN_POINT ( 'NONE',  ( 0.01132828649437914691, -0.9450724994329757767, 0.1162305715099754139 ) ) ;
#36238 = CARTESIAN_POINT ( 'NONE',  ( 0.4370955311001439303, -1.230376993490756687, 0.5844175963752731295 ) ) ;
#36239 = CARTESIAN_POINT ( 'NONE',  ( -0.02000000000000000042, -1.845925619402022155, -0.2644148183989317724 ) ) ;
#36240 = CARTESIAN_POINT ( 'NONE',  ( 0.001061621656357588511, -0.7083572002807602130, 0.2962098885571950446 ) ) ;
#36241 = CARTESIAN_POINT ( 'NONE',  ( 0.2117717001728993131, -0.8880493388543053701, 0.3804667941236127282 ) ) ;
#36242 = APPROVAL_ROLE ( '' ) ;
#36243 = CARTESIAN_POINT ( 'NONE',  ( 0.4717011137366580176, -1.062550488221034151, 0.8575416557712804977 ) ) ;
#36244 = CIRCLE ( 'NONE', #819, 0.06819284191469469902 ) ;
#36245 = CARTESIAN_POINT ( 'NONE',  ( 0.07216878364870175921, 0.05141091571461216952, -0.1249999999999971689 ) ) ;
#36246 = CARTESIAN_POINT ( 'NONE',  ( 0.3187624475196638163, -1.760353637077040068, 0.5684082056346195788 ) ) ;
#36247 = AXIS2_PLACEMENT_3D ( 'NONE', #26154, #32100, #19959 ) ;
#36248 = EDGE_LOOP ( 'NONE', ( #5136, #7471, #6963, #32647 ) ) ;
#36249 = CARTESIAN_POINT ( 'NONE',  ( 0.08495623427412302142, -1.462573956620219828, -0.6626765092577833194 ) ) ;
#36250 = CARTESIAN_POINT ( 'NONE',  ( 0.1198448511384348769, -1.120590779523480629, 0.9040002884437861042 ) ) ;
#36251 = CIRCLE ( 'NONE', #2761, 0.01000000000000002970 ) ;
#36252 = CARTESIAN_POINT ( 'NONE',  ( 0.01054817777343857940, -0.5296544771352952319, 0.1457185332388703236 ) ) ;
#36254 = ORIENTED_EDGE ( 'NONE', *, *, #30529, .F. ) ;
#36253 = CARTESIAN_POINT ( 'NONE',  ( 0.3895837468212401400, -1.765804909494755437, -0.5282886827880538538 ) ) ;
#36255 = CARTESIAN_POINT ( 'NONE',  ( 0.1383891728403247035, 0.05441343863104571715, -0.01030292142312775466 ) ) ;
#36256 = CARTESIAN_POINT ( 'NONE',  ( 0.2143793204313029777, -0.6499299462495844448, 0.4116214953459712556 ) ) ;
#36258 = ORIENTED_EDGE ( 'NONE', *, *, #37614, .F. ) ;
#36257 = ORIENTED_EDGE ( 'NONE', *, *, #15688, .F. ) ;
#36259 = CARTESIAN_POINT ( 'NONE',  ( 0.02130150994101746853, -1.626723050439328855, -0.6382336971175220919 ) ) ;
#36260 = CARTESIAN_POINT ( 'NONE',  ( 0.6400160853294423191, -1.459529829645036081, -0.3976988710621562895 ) ) ;
#36261 = CARTESIAN_POINT ( 'NONE',  ( 0.1826249073287969926, -1.261667980084790530, 0.4182417262808780789 ) ) ;
#36262 = COORDINATED_UNIVERSAL_TIME_OFFSET ( 0, 0, .AHEAD. ) ;
#36263 = CARTESIAN_POINT ( 'NONE',  ( 0.4670213778778394831, -1.236191465557153757, 0.6057417262809817737 ) ) ;
#36264 = ORIENTED_EDGE ( 'NONE', *, *, #26606, .T. ) ;
#36265 = CARTESIAN_POINT ( 'NONE',  ( 0.5474628067970259693, -1.166699794256029987, -0.6317669042598009765 ) ) ;
#36266 = CARTESIAN_POINT ( 'NONE',  ( 0.2188233872650832412, -0.8909256067445749938, 0.6610102726906746939 ) ) ;
#36267 = CARTESIAN_POINT ( 'NONE',  ( 0.2500145865922475119, -1.478584986872982343, 1.008546107030279027 ) ) ;
#36268 = CARTESIAN_POINT ( 'NONE',  ( 0.09782311751919105236, -0.5505692872209160260, 0.1905127806560832637 ) ) ;
#36270 = CARTESIAN_POINT ( 'NONE',  ( -0.3000000000000000999, -3.970782550070895311, -0.6634248229925526763 ) ) ;
#36269 = CARTESIAN_POINT ( 'NONE',  ( 0.2117622885028031254, -1.433178199125996199, 0.9421946221852213199 ) ) ;
#36271 = CARTESIAN_POINT ( 'NONE',  ( 0.09537293942087692045, -0.9336651254918434395, 0.2369052016270806194 ) ) ;
#36272 = ORIENTED_EDGE ( 'NONE', *, *, #32338, .F. ) ;
#36273 = ORIENTED_EDGE ( 'NONE', *, *, #5929, .F. ) ;
#36274 = CARTESIAN_POINT ( 'NONE',  ( 0.05082303569918595471, -0.4631054925596488903, -0.09932635337952287757 ) ) ;
#36275 = CARTESIAN_POINT ( 'NONE',  ( 0.1898178091108482235, -0.5354154051322274066, 0.1678590518679249910 ) ) ;
#36276 = DIRECTION ( 'NONE',  ( 1.000000000000000000, -0.000000000000000000, -0.000000000000000000 ) ) ;
#36277 = VECTOR ( 'NONE', #6343, 39.37007874015748143 ) ;
#36278 = AXIS2_PLACEMENT_3D ( 'NONE', #9838, #9223, #34734 ) ;
#36279 = EDGE_CURVE ( 'NONE', #12586, #36726, #29196, .T. ) ;
#36280 = APPROVAL ( #14859, 'UNSPECIFIED' ) ;
#36281 = DIRECTION ( 'NONE',  ( 0.4999551463232373427, -0.8660512985181134660, 0.000000000000000000 ) ) ;
#36282 = CIRCLE ( 'NONE', #8706, 0.03000000000000003011 ) ;
#36283 = CARTESIAN_POINT ( 'NONE',  ( 0.07814782694598980395, -1.316809471941703613, 0.4837547526852793434 ) ) ;
#36284 = CARTESIAN_POINT ( 'NONE',  ( 0.1763210608552490954, -1.872198378222803106, -0.6852895742237601340 ) ) ;
#36285 = CARTESIAN_POINT ( 'NONE',  ( 0.1048644750963132199, -1.410528588406870787, 0.5685427134957244943 ) ) ;
#36286 = CARTESIAN_POINT ( 'NONE',  ( 0.3304381985390301701, -0.8896417797241282788, 0.6549085351719812209 ) ) ;
#36287 = B_SPLINE_SURFACE_WITH_KNOTS ( 'NONE', 3, 3, ( 
 ( #9574, #25619, #21936, #754, #37752, #963, #6670, #19452, #22152, #13260, #22341, #34668, #6276, #35072, #12645, #25000, #6472, #12870, #28708, #31990, #3802, #34861, #25209, #32179, #25431 ),
 ( #9974, #37532, #19041, #31789, #34462, #9771, #9356, #31572, #18850, #19645, #31391, #15948, #3195, #3390, #3603, #28493, #22544, #15735, #38349, #28285, #7074, #16358, #28893, #10184, #366 ),
 ( #151, #3990, #16171, #572, #25830, #22753, #35279, #29506, #10793, #7880, #23749, #20262, #13661, #26841, #23364, #29922, #19839, #35677, #20058, #7480, #13853, #17575, #29313, #26226, #36080 ),
 ( #1764, #26648, #32783, #36271, #17368, #32374, #1346, #1161, #14276, #16962, #7265, #32986, #33203, #38748, #17157, #10574, #23148, #38561, #10384, #39369, #4200, #30117, #11189, #26426, #16765 ),
 ( #39179, #32589, #11005, #8093, #14073, #38963, #29706, #20670, #1552, #22947, #23562, #20452, #13472, #5008, #26039, #35464, #4585, #35886, #4404, #7697, #4793, #36492, #11607, #15083, #8498 ),
 ( #33398, #27031, #9107, #8910, #17760, #30311, #2138, #14677, #39558, #12210, #2546, #18578, #39777, #24352, #11392, #30523, #1949, #27247, #14464, #37293, #23964, #33591, #8306, #14889, #20877 ),
 ( #5205, #24169, #27638, #21487, #2348, #36693, #11998, #21063, #5400, #34202, #17963, #27448, #5615, #24565, #37095, #11794, #39973, #21673, #36886, #8695, #15287, #40386, #21273, #33810, #18171 ) ),
 .UNSPECIFIED., .F., .F., .F.,
 ( 4, 1, 1, 1, 4 ),
 ( 4, 1, 1, 1, 1, 1, 1, 1, 1, 1, 1, 1, 1, 1, 1, 1, 1, 1, 1, 1, 1, 1, 4 ),
 ( 0.000000000000000000, 0.2500000000000000000, 0.5000000000000000000, 0.7500000000000000000, 1.000000000000000000 ),
 ( 0.000000000000000000, 0.06250000000000000000, 0.1250000000000000000, 0.1666666666666666574, 0.1875000000000000000, 0.2500000000000000000, 0.3125000000000000000, 0.3750000000000000000, 0.4375000000000000000, 0.5000000000000000000, 0.5555555555555555802, 0.5625000000000000000, 0.6250000000000000000, 0.6875000000000000000, 0.7500000000000000000, 0.7812500000000000000, 0.8125000000000000000, 0.8437500000000000000, 0.8750000000000000000, 0.9062500000000000000, 0.9375000000000000000, 0.9687500000000000000, 1.000000000000000000 ),
 .UNSPECIFIED. ) ;
#36288 = DIRECTION ( 'NONE',  ( -0.4395832838285286814, -0.2366097102993482970, 0.8664769942535033298 ) ) ;
#36289 = DIRECTION ( 'NONE',  ( -0.4999999999999980016, -0.1032193326399760414, -0.8598521787896800106 ) ) ;
#36290 = CARTESIAN_POINT ( 'NONE',  ( -4.314083075427408721E-33, 0.1428018198284763673, -0.1638325989215043410 ) ) ;
#36291 = DIRECTION ( 'NONE',  ( 0.000000000000000000, -1.000000000000000000, 3.330669073875470607E-16 ) ) ;
#36292 = CARTESIAN_POINT ( 'NONE',  ( -0.04582897286455887842, -0.06484386734940761343, -0.4825967645925829941 ) ) ;
#36293 = CARTESIAN_POINT ( 'NONE',  ( -0.04308449196698393990, -0.2425978208598452146, -0.4306872647601475146 ) ) ;
#36294 = VERTEX_POINT ( 'NONE', #39563 ) ;
#36295 = CARTESIAN_POINT ( 'NONE',  ( 0.3099399546549871931, -0.9171249783946038292, 0.5994493976520077760 ) ) ;
#36296 = CIRCLE ( 'NONE', #28416, 0.7750185148639454624 ) ;
#36297 = CARTESIAN_POINT ( 'NONE',  ( 0.1424029337235096226, -1.400533250147911746, -0.6250000000000000000 ) ) ;
#36298 = EDGE_CURVE ( 'NONE', #33486, #38078, #16084, .T. ) ;
#36299 = CARTESIAN_POINT ( 'NONE',  ( 0.1364971356285234749, -1.133499090544220156, 0.7558102704853532083 ) ) ;
#36300 = ORIENTED_EDGE ( 'NONE', *, *, #37649, .T. ) ;
#36301 = EDGE_CURVE ( 'NONE', #26649, #12308, #20330, .T. ) ;
#36302 = CARTESIAN_POINT ( 'NONE',  ( 0.05562144613422628087, 0.2542273817772385258, 0.3844451335760726840 ) ) ;
#36303 = AXIS2_PLACEMENT_3D ( 'NONE', #2053, #17279, #32708 ) ;
#36304 = TOROIDAL_SURFACE ( 'NONE', #4762, 0.04999999999999998196, 0.1700000000000000400 ) ;
#36305 = CARTESIAN_POINT ( 'NONE',  ( 0.4000323062371948235, -1.610924870193226388, -0.3620271583837152418 ) ) ;
#36306 = CARTESIAN_POINT ( 'NONE',  ( 0.03174060074382504398, -0.5170807408089640456, -0.08825076429300719727 ) ) ;
#36307 = CARTESIAN_POINT ( 'NONE',  ( 0.1901749068777572604, -1.944933594392276088, -0.3001565292664163942 ) ) ;
#36308 = EDGE_CURVE ( 'NONE', #3047, #9108, #23318, .T. ) ;
#36309 = CARTESIAN_POINT ( 'NONE',  ( 0.4780493526100274004, -1.254977130501546467, 0.6087998174934282636 ) ) ;
#36311 = CARTESIAN_POINT ( 'NONE',  ( 0.1734973056165642902, -1.209394307038482497, -0.5155029497116575543 ) ) ;
#36310 = CARTESIAN_POINT ( 'NONE',  ( 0.3980789824590564852, -1.137894033439979635, 0.4906765649267371132 ) ) ;
#36312 = ADVANCED_FACE ( 'NONE', ( #14893 ), #36448, .F. ) ;
#36313 = FACE_OUTER_BOUND ( 'NONE', #34233, .T. ) ;
#36314 = ORIENTED_EDGE ( 'NONE', *, *, #21233, .F. ) ;
#36315 = EDGE_CURVE ( 'NONE', #11533, #22491, #1769, .T. ) ;
#36316 = CARTESIAN_POINT ( 'NONE',  ( 0.5860257985473389386, -1.592810714289445650, 0.4182417262808776903 ) ) ;
#36317 = ORIENTED_EDGE ( 'NONE', *, *, #23735, .F. ) ;
#36318 = CARTESIAN_POINT ( 'NONE',  ( 0.1895943254151421786, -0.6407273034312881421, 0.008518417185872215538 ) ) ;
#36319 = CARTESIAN_POINT ( 'NONE',  ( 0.06062184886820209256, -0.5472141424593505166, 0.2036466807051401096 ) ) ;
#36320 = AXIS2_PLACEMENT_3D ( 'NONE', #32742, #29664, #32945 ) ;
#36322 = CARTESIAN_POINT ( 'NONE',  ( 0.05634304521267768928, -2.731847993664263218E-15, -0.4588823192046729837 ) ) ;
#36321 = CARTESIAN_POINT ( 'NONE',  ( 0.08990334728944714138, -0.5646811812073189163, 0.1486427366963163632 ) ) ;
#36323 = CARTESIAN_POINT ( 'NONE',  ( -2.915087563824520450E-32, 7.160938508832261116E-17, 0.2149999999999999967 ) ) ;
#36324 = ORIENTED_EDGE ( 'NONE', *, *, #2201, .F. ) ;
#36325 = B_SPLINE_CURVE_WITH_KNOTS ( 'NONE', 3,
 ( #29023, #39046, #4667, #14548, #30190, #33469, #33073, #40045, #8179, #24049, #33676, #33277 ),
 .UNSPECIFIED., .F., .F.,
 ( 4, 2, 2, 2, 2, 4 ),
 ( 0.000000000000000000, 0.0005853004908840498495, 0.001170600981768099699, 0.001755901472652149440, 0.002048551718094174419, 0.002341201963536199832 ),
 .UNSPECIFIED. ) ;
#36326 = ORIENTED_EDGE ( 'NONE', *, *, #18291, .T. ) ;
#36327 = DIRECTION ( 'NONE',  ( 1.000000000000000000, 0.000000000000000000, 0.000000000000000000 ) ) ;
#36328 = CARTESIAN_POINT ( 'NONE',  ( 0.4635535538083537244, -1.314077908205018241, 0.8227958598471974971 ) ) ;
#36329 = APPLICATION_CONTEXT ( 'configuration controlled 3d designs of mechanical parts and assemblies' ) ;
#36330 = VERTEX_POINT ( 'NONE', #39372 ) ;
#36331 = CARTESIAN_POINT ( 'NONE',  ( 0.3207912813105621153, -1.758981359444245385, 0.5311847171115458011 ) ) ;
#36332 = CARTESIAN_POINT ( 'NONE',  ( 0.03647060353176064668, -0.5060729159580577008, 0.07645842516611485451 ) ) ;
#36333 = EDGE_CURVE ( 'NONE', #35762, #25919, #14397, .T. ) ;
#36334 = B_SPLINE_CURVE_WITH_KNOTS ( 'NONE', 3,
 ( #28179, #44, #24701, #18718, #34135, #15430 ),
 .UNSPECIFIED., .F., .F.,
 ( 4, 2, 4 ),
 ( 0.0008728868357568681348, 0.001510076209140402432, 0.002147265582523936404 ),
 .UNSPECIFIED. ) ;
#36335 = CARTESIAN_POINT ( 'NONE',  ( 0.3639973713284520018, -1.769128485143046436, -0.4349400384763179583 ) ) ;
#36336 = APPLIED_PERSON_AND_ORGANIZATION_ASSIGNMENT ( #24084, #26944, ( #25296 ) ) ;
#36337 = CARTESIAN_POINT ( 'NONE',  ( 0.1891515964196448796, -1.246317699220909958, 0.4467030175713385121 ) ) ;
#36338 = CONICAL_SURFACE ( 'NONE', #29764, 0.4488493849861021068, 1.047197551196599408 ) ;
#36339 = CARTESIAN_POINT ( 'NONE',  ( 0.03113248654051816583, -0.3458405862425447119, -0.1052451372150005060 ) ) ;
#36340 = CARTESIAN_POINT ( 'NONE',  ( 0.08988759086353000083, -0.6029188970129375491, 0.1463085495562314320 ) ) ;
#36341 = CARTESIAN_POINT ( 'NONE',  ( 0.6419406851146725046, -1.339736372716090917, 0.8215813590131169075 ) ) ;
#36342 = CIRCLE ( 'NONE', #28447, 0.06000000000000021289 ) ;
#36343 = AXIS2_PLACEMENT_3D ( 'NONE', #38434, #13552, #13732 ) ;
#36344 = DIRECTION ( 'NONE',  ( 0.000000000000000000, 0.000000000000000000, -1.000000000000000000 ) ) ;
#36345 = CARTESIAN_POINT ( 'NONE',  ( -0.02000000000000000042, -2.551729310907437043, -0.5086726180052709712 ) ) ;
#36346 = CARTESIAN_POINT ( 'NONE',  ( 0.6269135997112185166, -1.610086856713869308, -0.5704037409038575923 ) ) ;
#36347 = CARTESIAN_POINT ( 'NONE',  ( 0.04308558661661603117, 0.3346374335305056791, 0.3638133228716420309 ) ) ;
#36348 = CARTESIAN_POINT ( 'NONE',  ( 0.5750090102395998271, -1.613396230683133759, 0.5672260050467223813 ) ) ;
#36349 = DIRECTION ( 'NONE',  ( 0.000000000000000000, 0.000000000000000000, -1.000000000000000000 ) ) ;
#36350 = AXIS2_PLACEMENT_3D ( 'NONE', #15359, #20937, #2216 ) ;
#36351 = CARTESIAN_POINT ( 'NONE',  ( -0.1055448275397413149, -0.4799318856336941552, 0.3601683063145866837 ) ) ;
#36352 = CARTESIAN_POINT ( 'NONE',  ( 0.06825878040686909898, -0.8404074238475144343, 0.8024108098889147778 ) ) ;
#36353 = CARTESIAN_POINT ( 'NONE',  ( 0.5756165940928597013, -1.567873191104453223, -0.5835715271696909623 ) ) ;
#36354 = DIRECTION ( 'NONE',  ( -1.000000000000000000, -0.000000000000000000, -0.000000000000000000 ) ) ;
#36355 = CARTESIAN_POINT ( 'NONE',  ( 0.3047936848243344432, -1.756875962071034580, 0.5682417262361116883 ) ) ;
#36356 = ORIENTED_EDGE ( 'NONE', *, *, #25869, .T. ) ;
#36357 = EDGE_CURVE ( 'NONE', #19345, #10240, #24267, .T. ) ;
#36358 = FACE_OUTER_BOUND ( 'NONE', #3086, .T. ) ;
#36359 = CARTESIAN_POINT ( 'NONE',  ( 0.3625960434667522825, -1.762758894398491760, -0.5926935080085824481 ) ) ;
#36360 = CARTESIAN_POINT ( 'NONE',  ( 0.08778601674903806218, -0.5530204048924579618, 0.1461273381126583226 ) ) ;
#36361 = CARTESIAN_POINT ( 'NONE',  ( 0.6079668211846660508, -1.561367219176452714, -0.4113520219294763969 ) ) ;
#36362 = CIRCLE ( 'NONE', #940, 0.06000000000000045575 ) ;
#36363 = EDGE_CURVE ( 'NONE', #32520, #33386, #15086, .T. ) ;
#36364 = CARTESIAN_POINT ( 'NONE',  ( 0.4992372981854732439, -1.293093988718565956, 0.7065005728875947133 ) ) ;
#36366 = ORIENTED_EDGE ( 'NONE', *, *, #21857, .T. ) ;
#36365 = CARTESIAN_POINT ( 'NONE',  ( 0.05999999999999990757, 0.5878163732725504298, -0.1704268771689479434 ) ) ;
#36367 = CARTESIAN_POINT ( 'NONE',  ( 0.3302065591133839240, -0.9317669992161012882, 0.6252562391197076241 ) ) ;
#36368 = EDGE_CURVE ( 'NONE', #36928, #27541, #31844, .T. ) ;
#36369 = DIRECTION ( 'NONE',  ( 0.000000000000000000, 0.9510565162951392093, -0.3090169943749916381 ) ) ;
#36370 = VERTEX_POINT ( 'NONE', #3553 ) ;
#36371 = DIRECTION ( 'NONE',  ( 0.000000000000000000, 0.000000000000000000, 1.000000000000000000 ) ) ;
#36372 = AXIS2_PLACEMENT_3D ( 'NONE', #10454, #19921, #1046 ) ;
#36373 = VERTEX_POINT ( 'NONE', #31350 ) ;
#36374 = CIRCLE ( 'NONE', #14059, 0.1400000000000004297 ) ;
#36375 = CARTESIAN_POINT ( 'NONE',  ( 0.1127314162110860801, -0.9204869745937769299, 0.7651726503946431057 ) ) ;
#36377 = CARTESIAN_POINT ( 'NONE',  ( 0.1878447062321111916, -0.5357678935135709031, 0.07285347281293909349 ) ) ;
#36376 = CARTESIAN_POINT ( 'NONE',  ( 0.6981984480215006617, -1.496421087833687213, 0.4851264061261034710 ) ) ;
#36378 = DIRECTION ( 'NONE',  ( 0.000000000000000000, 3.330669073875470114E-16, 1.000000000000000000 ) ) ;
#36379 = DIRECTION ( 'NONE',  ( 1.000000000000000000, 6.779273404243070203E-32, 4.314083075427407763E-32 ) ) ;
#36380 = ORIENTED_EDGE ( 'NONE', *, *, #13256, .F. ) ;
#36381 = CIRCLE ( 'NONE', #26562, 0.04500000000000030365 ) ;
#36382 = CARTESIAN_POINT ( 'NONE',  ( -7.709217208076694605E-10, -2.079844940525741315, -0.6906928555465188246 ) ) ;
#36383 = FACE_OUTER_BOUND ( 'NONE', #20821, .T. ) ;
#36384 = ADVANCED_FACE ( 'NONE', ( #25574 ), #12212, .F. ) ;
#36385 = VECTOR ( 'NONE', #39328, 39.37007874015748143 ) ;
#36386 = EDGE_CURVE ( 'NONE', #26082, #20946, #33557, .T. ) ;
#36387 = CARTESIAN_POINT ( 'NONE',  ( 0.2377172976805353166, -1.126050835660724836, 0.7471600383748348007 ) ) ;
#36388 = CARTESIAN_POINT ( 'NONE',  ( -2.359223927328457648E-16, -0.02999999999999984276, -0.1699999999999995126 ) ) ;
#36389 = EDGE_CURVE ( 'NONE', #32357, #16250, #19376, .T. ) ;
#36390 = CARTESIAN_POINT ( 'NONE',  ( 0.04293324258486909406, 0.07181764475133010917, -0.4893676133895061842 ) ) ;
#36391 = ADVANCED_FACE ( 'NONE', ( #34010 ), #22251, .F. ) ;
#36392 = CARTESIAN_POINT ( 'NONE',  ( 0.2283924689359978499, -0.9952348863919213695, 0.5666251819813739043 ) ) ;
#36393 = CARTESIAN_POINT ( 'NONE',  ( 0.6589703859825570831, -1.564329074718757484, 0.3667417262808780887 ) ) ;
#36394 =( BOUNDED_SURFACE ( )  B_SPLINE_SURFACE ( 3, 2, ( 
 ( #21356, #8566, #33897 ),
 ( #5696, #11675, #30797 ),
 ( #2617, #5271, #40041 ),
 ( #5881, #21559, #17831 ),
 ( #12289, #27712, #24845 ),
 ( #21139, #31214, #34278 ),
 ( #40246, #37367, #9178 ),
 ( #39855, #12083, #2224 ),
 ( #11475, #21745, #24644 ),
 ( #24232, #18656, #14761 ),
 ( #33668, #24042, #36755 ),
 ( #36570, #8375, #5482 ) ),
 .UNSPECIFIED., .F., .F., .T. ) 
 B_SPLINE_SURFACE_WITH_KNOTS ( ( 4, 2, 2, 2, 2, 4 ),
 ( 3, 3 ),
 ( 0.000000000000000000, 0.0002379057407600430744, 0.0004758114815200861487, 0.0009516229630401722974, 0.001427434444560258392, 0.001903245926080344595 ),
 ( 0.000000000000000000, 1.000000000000000000 ),
 .UNSPECIFIED. ) 
 GEOMETRIC_REPRESENTATION_ITEM ( )  RATIONAL_B_SPLINE_SURFACE ( (
 ( 1.000000000000000000, 0.8659230874819799917, 1.000000000000000000),
 ( 1.000000000000000000, 0.8654830159531572420, 1.000000000000000000),
 ( 1.000000000000000000, 0.8634833282782717889, 1.000000000000000000),
 ( 1.000000000000000000, 0.8560673753524404850, 1.000000000000000000),
 ( 1.000000000000000000, 0.8505305545019991031, 1.000000000000000000),
 ( 1.000000000000000000, 0.8302514985868648667, 1.000000000000000000),
 ( 1.000000000000000000, 0.8122569203425941131, 1.000000000000000000),
 ( 1.000000000000000000, 0.7769176656627446720, 1.000000000000000000),
 ( 1.000000000000000000, 0.7592262555998681162, 1.000000000000000000),
 ( 1.000000000000000000, 0.7244430868634086362, 1.000000000000000000),
 ( 1.000000000000000000, 0.7073027160842355610, 1.000000000000000000),
 ( 1.000000000000000000, 0.6906290772346568296, 1.000000000000000000) ) ) 
 REPRESENTATION_ITEM ( '' )  SURFACE ( )  );
#36395 = CARTESIAN_POINT ( 'NONE',  ( 0.05283102792148736127, 0.2421768296208689775, -0.4008516595826039364 ) ) ;
#36396 = CARTESIAN_POINT ( 'NONE',  ( 0.4095772007298983941, -1.132452871991625143, 0.4852699800312822997 ) ) ;
#36397 = B_SPLINE_CURVE_WITH_KNOTS ( 'NONE', 5,
 ( #25901, #13121, #38419, #16411, #10257, #3860 ),
 .UNSPECIFIED., .F., .F.,
 ( 6, 6 ),
 ( 12.39904547089488496, 12.50424887933038676 ),
 .UNSPECIFIED. ) ;
#36398 = CARTESIAN_POINT ( 'NONE',  ( 0.01548846960703785525, -0.09061086148575045462, 0.5171215251571049665 ) ) ;
#36399 = CALENDAR_DATE ( 2026, 13, 10 ) ;
#36400 = AXIS2_PLACEMENT_3D ( 'NONE', #32677, #17047, #10062 ) ;
#36401 = CARTESIAN_POINT ( 'NONE',  ( 0.06310204368368470262, -1.326805032915164162, 0.6102011665707310906 ) ) ;
#36402 = CARTESIAN_POINT ( 'NONE',  ( 0.3605539653964052182, -1.159620486319301813, 0.5253391196606768121 ) ) ;
#36403 = CARTESIAN_POINT ( 'NONE',  ( -0.05464101615137786222, -2.183180860297908144, -0.4937760292030871079 ) ) ;
#36404 = CIRCLE ( 'NONE', #39690, 0.6115209409081865388 ) ;
#36405 = VERTEX_POINT ( 'NONE', #6829 ) ;
#36406 = AXIS2_PLACEMENT_3D ( 'NONE', #15658, #28207, #72 ) ;
#36407 = PRODUCT_DEFINITION_SHAPE ( 'NONE', 'NONE',  #40662 ) ;
#36408 = CARTESIAN_POINT ( 'NONE',  ( 2.003769519753459454E-05, -0.4887874499424059715, -0.02467011407665378395 ) ) ;
#36409 = CARTESIAN_POINT ( 'NONE',  ( 0.3939420568793829402, -1.988526800673050321, -0.5001229575649985826 ) ) ;
#36410 = CARTESIAN_POINT ( 'NONE',  ( 0.0004801912913160456516, -0.4395057766670965038, 0.1677942470109538287 ) ) ;
#36411 = CARTESIAN_POINT ( 'NONE',  ( -0.2399999999999999079, -2.768941938641841904, -0.5551618215276492574 ) ) ;
#36412 = AXIS2_PLACEMENT_3D ( 'NONE', #17966, #5012, #30527 ) ;
#36413 = VERTEX_POINT ( 'NONE', #17114 ) ;
#36414 = ORIENTED_EDGE ( 'NONE', *, *, #17315, .F. ) ;
#36415 = TOROIDAL_SURFACE ( 'NONE', #30492, 0.9237847906030132172, 0.01499999999999999944 ) ;
#36416 = CARTESIAN_POINT ( 'NONE',  ( 0.1733962078978711074, -0.5203934806767281929, 0.1236872031806311029 ) ) ;
#36417 = EDGE_LOOP ( 'NONE', ( #10277, #24448, #15874, #30495 ) ) ;
#36418 = CARTESIAN_POINT ( 'NONE',  ( 2.090519358671640883E-16, 0.2900000000000004241, -0.07500000000000042744 ) ) ;
#36419 = EDGE_CURVE ( 'NONE', #30626, #26082, #11011, .T. ) ;
#36420 = DIRECTION ( 'NONE',  ( 0.4261641068392654774, -0.9046458721742397513, 0.000000000000000000 ) ) ;
#36422 = ORIENTED_EDGE ( 'NONE', *, *, #10233, .T. ) ;
#36421 = CARTESIAN_POINT ( 'NONE',  ( -0.001329024702343150049, -0.8150860535562964859, 0.03600470908344870907 ) ) ;
#36423 = EDGE_CURVE ( 'NONE', #22311, #35502, #1644, .T. ) ;
#36424 = ORIENTED_EDGE ( 'NONE', *, *, #12225, .F. ) ;
#36425 = CARTESIAN_POINT ( 'NONE',  ( 0.5521441265314278590, -1.306365183234622585, 0.8936522956502730430 ) ) ;
#36426 = ORIENTED_EDGE ( 'NONE', *, *, #7490, .F. ) ;
#36427 = CARTESIAN_POINT ( 'NONE',  ( 0.2059273467974227778, -1.283046334493782359, -0.7137159211901564770 ) ) ;
#36429 = CARTESIAN_POINT ( 'NONE',  ( 0.1658945499291084036, -1.260523426758859644, 0.6030236252751928205 ) ) ;
#36428 = CARTESIAN_POINT ( 'NONE',  ( -0.02231181081520701784, -0.4612879682508957413, -0.2235517164227203701 ) ) ;
#36430 = CARTESIAN_POINT ( 'NONE',  ( 0.3516101416147200953, -1.741639419776285891, -0.7019724635597545115 ) ) ;
#36431 = PERSON_AND_ORGANIZATION ( #20137, #32613 ) ;
#36432 = AXIS2_PLACEMENT_3D ( 'NONE', #26870, #36528, #7915 ) ;
#36433 = CARTESIAN_POINT ( 'NONE',  ( -0.2746410161513770931, -3.217981293616048344, -0.2530108926800491709 ) ) ;
#36435 = ORIENTED_EDGE ( 'NONE', *, *, #29541, .F. ) ;
#36434 = VERTEX_POINT ( 'NONE', #32331 ) ;
#36436 = CARTESIAN_POINT ( 'NONE',  ( 0.01170466158157320614, -0.7209202686218528777, -0.1115487569099005288 ) ) ;
#36437 = DIRECTION ( 'NONE',  ( -1.000000000000000000, -0.000000000000000000, -0.000000000000000000 ) ) ;
#36438 = AXIS2_PLACEMENT_3D ( 'NONE', #14377, #14190, #11305 ) ;
#36439 = CARTESIAN_POINT ( 'NONE',  ( 0.09213258466004858871, -0.5863880887348119630, 0.2398429810774082571 ) ) ;
#36440 = CIRCLE ( 'NONE', #14118, 0.4615209409081865166 ) ;
#36441 = CARTESIAN_POINT ( 'NONE',  ( 0.01128729522873459998, -0.9461985897320852601, 0.1796480652156055013 ) ) ;
#36442 = CARTESIAN_POINT ( 'NONE',  ( -0.02000000000000000042, -2.183180860297908144, -0.4937760292030871079 ) ) ;
#36443 = APPLIED_SECURITY_CLASSIFICATION_ASSIGNMENT ( #2940, ( #4217 ) ) ;
#36444 = CARTESIAN_POINT ( 'NONE',  ( 0.06485935661193353852, -1.341259894741156700, 0.5606283090912991263 ) ) ;
#36445 = FACE_OUTER_BOUND ( 'NONE', #18064, .T. ) ;
#36446 = CARTESIAN_POINT ( 'NONE',  ( 0.4079725984602744493, -1.712446521674362732, 0.4259523847339783953 ) ) ;
#36447 = ADVANCED_FACE ( 'NONE', ( #28855 ), #24633, .T. ) ;
#36448 = CONICAL_SURFACE ( 'NONE', #38407, 0.1600000000000016964, 1.047197551196601406 ) ;
#36449 = CARTESIAN_POINT ( 'NONE',  ( 0.08978098643734212791, 0.000000000000000000, 0.000000000000000000 ) ) ;
#36450 = LINE ( 'NONE', #30691, #13959 ) ;
#36451 = CARTESIAN_POINT ( 'NONE',  ( -0.1212602504878780296, -0.5073146173917506552, 0.1528658435936999238 ) ) ;
#36452 = CARTESIAN_POINT ( 'NONE',  ( -3.837675818371248128E-05, -0.9481486753962028446, 0.1506679456753735602 ) ) ;
#36453 = CARTESIAN_POINT ( 'NONE',  ( 0.3583927816463333693, -1.622105672670009380, -0.4230600629973198523 ) ) ;
#36454 = DIRECTION ( 'NONE',  ( -6.162975822039154730E-33, 0.9777314879352116961, -0.2098598043933068147 ) ) ;
#36455 = CARTESIAN_POINT ( 'NONE',  ( 5.463695987328526437E-16, -0.2899999999999993694, -7.171100983368691195E-16 ) ) ;
#36456 = CARTESIAN_POINT ( 'NONE',  ( 0.003441938119505853853, -0.5826794048688673788, 0.2512083064573837898 ) ) ;
#36457 = CARTESIAN_POINT ( 'NONE',  ( 0.1854168535569865883, -0.8697360073808750869, 0.1550939566555308846 ) ) ;
#36458 = CARTESIAN_POINT ( 'NONE',  ( 0.02418895824641892692, -0.9508555545350739768, 0.6316828188328664773 ) ) ;
#36459 = DATE_AND_TIME ( #35643, #32527 ) ;
#36460 = CARTESIAN_POINT ( 'NONE',  ( 0.5573545814012507149, -1.203739305690170402, 0.8778060520269345135 ) ) ;
#36461 = AXIS2_PLACEMENT_3D ( 'NONE', #30673, #33963, #39923 ) ;
#36462 = CONICAL_SURFACE ( 'NONE', #8859, 0.03999999999999950817, 1.047197551196597409 ) ;
#36463 = CARTESIAN_POINT ( 'NONE',  ( 0.3894066849061866842, -1.614605012626642910, -0.6684378029408698518 ) ) ;
#36464 = CARTESIAN_POINT ( 'NONE',  ( 0.3187246401137938112, -1.760368955180017236, 0.5676021236855325336 ) ) ;
#36465 = VECTOR ( 'NONE', #4226, 39.37007874015748143 ) ;
#36466 = ORIENTED_EDGE ( 'NONE', *, *, #19064, .F. ) ;
#36467 = CARTESIAN_POINT ( 'NONE',  ( 0.1999999999999788058, -2.097675824466502803, -0.7286991843995631601 ) ) ;
#36468 = PRODUCT_DEFINITION_FORMATION_WITH_SPECIFIED_SOURCE ( 'ANY', '', #14383, .NOT_KNOWN. ) ;
#36469 = CARTESIAN_POINT ( 'NONE',  ( 0.07641379623259875187, -0.9713282881620481923, 0.8144253132993416466 ) ) ;
#36470 = EDGE_CURVE ( 'NONE', #25200, #30050, #23958, .T. ) ;
#36471 = CARTESIAN_POINT ( 'NONE',  ( 0.3712243616927410894, -1.761250189250869180, -0.4316674211170486442 ) ) ;
#36473 = VERTEX_POINT ( 'NONE', #22708 ) ;
#36472 = DIRECTION ( 'NONE',  ( 0.8660512985181133550, 0.4999551463232371207, 0.000000000000000000 ) ) ;
#36474 = CARTESIAN_POINT ( 'NONE',  ( 0.3224711051296385578, -1.754080271473366093, 0.4780932018388675542 ) ) ;
#36475 = CONICAL_SURFACE ( 'NONE', #8218, 0.1400000000000005684, 1.047197551196600962 ) ;
#36476 = CARTESIAN_POINT ( 'NONE',  ( 0.5155751834530871713, -1.137973747986757544, 0.7479765829993398896 ) ) ;
#36478 = ORIENTED_EDGE ( 'NONE', *, *, #24046, .T. ) ;
#36477 = ORIENTED_EDGE ( 'NONE', *, *, #38086, .F. ) ;
#36479 = CARTESIAN_POINT ( 'NONE',  ( 0.09016133453268133924, -1.373701387894656900, -0.6687768065943457962 ) ) ;
#36480 = ORIENTED_EDGE ( 'NONE', *, *, #31387, .F. ) ;
#36481 = DIRECTION ( 'NONE',  ( 1.000000000000000000, 0.000000000000000000, 0.000000000000000000 ) ) ;
#36482 = CARTESIAN_POINT ( 'NONE',  ( 0.2948640431821396013, -1.208698857570559948, 0.4182417262808778013 ) ) ;
#36483 = DATE_TIME_ROLE ( 'classification_date' ) ;
#36484 = CARTESIAN_POINT ( 'NONE',  ( -0.2399999999999999079, -3.701811653776600597, -0.3192834175180689904 ) ) ;
#36485 = EDGE_LOOP ( 'NONE', ( #21064, #7829, #12341, #37745 ) ) ;
#36486 = DIRECTION ( 'NONE',  ( -0.8660512985181132439, -0.4999551463232374537, 0.000000000000000000 ) ) ;
#36487 = CARTESIAN_POINT ( 'NONE',  ( 0.1251483427054724540, -0.7782096407036064312, 0.4562269205239417591 ) ) ;
#36488 = CARTESIAN_POINT ( 'NONE',  ( 0.3154013571205182553, -1.680250829566968473, 0.8751360567703019289 ) ) ;
#36489 = CARTESIAN_POINT ( 'NONE',  ( 0.09985988637870266138, -0.5731286213205528668, 0.2623670383419783314 ) ) ;
#36491 = FACE_OUTER_BOUND ( 'NONE', #4177, .T. ) ;
#36490 = CARTESIAN_POINT ( 'NONE',  ( 0.1146734031460662356, -0.4828071762122547739, 0.01829575716233284438 ) ) ;
#36492 = CARTESIAN_POINT ( 'NONE',  ( 0.1659062591970449363, -1.250628541066444388, 0.6134509435559128976 ) ) ;
#36493 = ORIENTED_EDGE ( 'NONE', *, *, #25626, .F. ) ;
#36494 = VERTEX_POINT ( 'NONE', #1506 ) ;
#36495 = AXIS2_PLACEMENT_3D ( 'NONE', #7375, #26933, #4500 ) ;
#36496 = CARTESIAN_POINT ( 'NONE',  ( 0.3174184176267951796, -1.762933076790987874, 0.5319023928053561168 ) ) ;
#36497 = CARTESIAN_POINT ( 'NONE',  ( 0.3348785992456718708, -0.8147534913312738380, 0.7321433735801530229 ) ) ;
#36498 = VECTOR ( 'NONE', #2411, 39.37007874015748143 ) ;
#36499 = FACE_OUTER_BOUND ( 'NONE', #6512, .T. ) ;
#36500 = DIRECTION ( 'NONE',  ( 1.000000000000000000, 0.000000000000000000, 0.000000000000000000 ) ) ;
#36501 = APPLIED_SECURITY_CLASSIFICATION_ASSIGNMENT ( #25357, ( #39149 ) ) ;
#36502 = CARTESIAN_POINT ( 'NONE',  ( -0.05634490452572749747, -0.4379840114246532634, -0.1369850167785242601 ) ) ;
#36503 = EDGE_CURVE ( 'NONE', #9452, #14931, #1308, .T. ) ;
#36504 = DIRECTION ( 'NONE',  ( 1.912293595564980111E-14, 0.7743343091952541446, -0.6327767201810673425 ) ) ;
#36505 = CARTESIAN_POINT ( 'NONE',  ( 0.2498074192101490676, -1.572794153342251811, -0.7074376191508968681 ) ) ;
#36506 = AXIS2_PLACEMENT_3D ( 'NONE', #9481, #71, #15250 ) ;
#36507 = CARTESIAN_POINT ( 'NONE',  ( 0.3504057387187115014, -1.153664717295436404, 0.4422128889498893045 ) ) ;
#36508 = CARTESIAN_POINT ( 'NONE',  ( 0.4104166757648185504, -0.9945572768306742972, 0.7245767828144217271 ) ) ;
#36509 = DATE_TIME_ROLE ( 'classification_date' ) ;
#36510 = CARTESIAN_POINT ( 'NONE',  ( -0.1104192559602747703, -0.5043764815743673191, 0.1033498972402037835 ) ) ;
#36511 = LINE ( 'NONE', #8322, #9410 ) ;
#36512 = CARTESIAN_POINT ( 'NONE',  ( 0.3683934783552571535, -2.038992781902201124, -0.6813765817288593984 ) ) ;
#36513 = VERTEX_POINT ( 'NONE', #26596 ) ;
#36514 = DIRECTION ( 'NONE',  ( 1.000000000000000000, 0.000000000000000000, 1.138269997360110167E-15 ) ) ;
#36515 = SPHERICAL_SURFACE ( 'NONE', #21240, 0.01499999999999999944 ) ;
#36516 = CARTESIAN_POINT ( 'NONE',  ( -0.04947837552028281488, -0.3081459059633547826, -0.3644550506195411987 ) ) ;
#36517 = ORIENTED_EDGE ( 'NONE', *, *, #17922, .F. ) ;
#36518 = FACE_OUTER_BOUND ( 'NONE', #16690, .T. ) ;
#36519 = LINE ( 'NONE', #1788, #39689 ) ;
#36520 = CIRCLE ( 'NONE', #7590, 0.01000000000000002623 ) ;
#36521 = CIRCLE ( 'NONE', #12215, 0.01500000000000001159 ) ;
#36522 = CARTESIAN_POINT ( 'NONE',  ( 0.1620965704063034862, -1.205491034068324252, 0.7491300204058332080 ) ) ;
#36523 = EDGE_LOOP ( 'NONE', ( #23447, #25501, #26479, #11227, #31384, #38839, #21776, #6811, #4253 ) ) ;
#36524 = CARTESIAN_POINT ( 'NONE',  ( 0.01548846960707511190, -0.2306506793134066036, 0.4716198300880325434 ) ) ;
#36525 = CARTESIAN_POINT ( 'NONE',  ( -0.02000000000000000042, -2.144840178508589545, -0.3363606153560244616 ) ) ;
#36526 = ORGANIZATION ( 'NAUO-ORG5', 'UNSPECIFIED', 'UNSPECIFIED' ) ;
#36527 = CARTESIAN_POINT ( 'NONE',  ( 0.1613371997446969852, -1.389521869439662938, 0.4310088812813361869 ) ) ;
#36528 = DIRECTION ( 'NONE',  ( -1.000000000000000000, -0.000000000000000000, -0.000000000000000000 ) ) ;
#36529 = CARTESIAN_POINT ( 'NONE',  ( 0.4411176185871907296, -1.199366743384446377, 0.6758596692312155430 ) ) ;
#36531 = CARTESIAN_POINT ( 'NONE',  ( -0.02000000000000000042, -2.379949255320110257, -0.6346823614705312533 ) ) ;
#36530 = CARTESIAN_POINT ( 'NONE',  ( 0.05489899477340703243, 0.4472784955204376911, 0.1186631084353854670 ) ) ;
#36532 = PLANE ( 'NONE',  #34908 ) ;
#36533 = ORIENTED_EDGE ( 'NONE', *, *, #14668, .F. ) ;
#36534 = CIRCLE ( 'NONE', #18812, 0.01499999999999994567 ) ;
#36535 = CARTESIAN_POINT ( 'NONE',  ( 0.06979851145747001384, -1.326871333008951881, 0.5494227783323851755 ) ) ;
#36536 = ORIENTED_EDGE ( 'NONE', *, *, #23058, .T. ) ;
#36537 = DIRECTION ( 'NONE',  ( 0.8660512985181132439, 0.4999551463232376758, 0.000000000000000000 ) ) ;
#36538 = CARTESIAN_POINT ( 'NONE',  ( 0.4132723870208870331, -1.504063452548798807, 0.8015072579983955059 ) ) ;
#36540 = CARTESIAN_POINT ( 'NONE',  ( 0.1857430203655689172, -0.8056635886342105035, 0.2698372336795832882 ) ) ;
#36539 = CARTESIAN_POINT ( 'NONE',  ( 0.08803424184564076493, -0.6404506698634022666, 0.009295576138141414813 ) ) ;
#36541 = CARTESIAN_POINT ( 'NONE',  ( 0.4412551199097751176, -1.145691214381745038, 0.4235448160515665195 ) ) ;
#36542 = EDGE_LOOP ( 'NONE', ( #10771, #17964, #15025, #32863, #30196, #25933, #27639 ) ) ;
#36543 = VERTEX_POINT ( 'NONE', #7040 ) ;
#36544 = CARTESIAN_POINT ( 'NONE',  ( 0.1791084308631172295, -1.789643132935252234, -0.3232808063848631175 ) ) ;
#36545 = B_SPLINE_CURVE_WITH_KNOTS ( 'NONE', 3,
 ( #7611, #20795, #20985, #13981, #17490, #26553 ),
 .UNSPECIFIED., .F., .F.,
 ( 4, 2, 4 ),
 ( 0.005183784548773252843, 0.005807229420386499606, 0.006430674291999746370 ),
 .UNSPECIFIED. ) ;
#36546 = CARTESIAN_POINT ( 'NONE',  ( 0.5566350444588750168, -1.457454591888360573, 0.7347119787586107176 ) ) ;
#36547 = CARTESIAN_POINT ( 'NONE',  ( 0.05999999999999990757, 0.000000000000000000, 0.000000000000000000 ) ) ;
#36548 = CARTESIAN_POINT ( 'NONE',  ( 0.3999999999999786504, -2.120723258816476609, -0.4622723469118392714 ) ) ;
#36549 = CARTESIAN_POINT ( 'NONE',  ( 0.6009414993585495690, -1.584005022665416984, 0.4182417262808776903 ) ) ;
#36550 = CARTESIAN_POINT ( 'NONE',  ( 0.09165208117211873229, -1.314337288742353227, 0.4470340182402313123 ) ) ;
#36551 = CARTESIAN_POINT ( 'NONE',  ( 0.3957373257482387774, -1.750805605674629950, -0.5219666508750002709 ) ) ;
#36552 = CARTESIAN_POINT ( 'NONE',  ( 0.08911620379650853074, -0.6035282328652368244, 0.06395801244005373809 ) ) ;
#36553 = AXIS2_PLACEMENT_3D ( 'NONE', #32239, #16626, #1414 ) ;
#36554 = EDGE_CURVE ( 'NONE', #13751, #30110, #16378, .T. ) ;
#36555 = EDGE_CURVE ( 'NONE', #38935, #17501, #18132, .T. ) ;
#36556 = CARTESIAN_POINT ( 'NONE',  ( 0.1876258513389257310, -0.4649338269308297966, 0.1998821562507554217 ) ) ;
#36557 = EDGE_CURVE ( 'NONE', #23564, #30450, #1906, .T. ) ;
#36558 = CARTESIAN_POINT ( 'NONE',  ( 0.07296648554937049114, -1.326663526568331752, 0.4848661492846349508 ) ) ;
#36559 = DIRECTION ( 'NONE',  ( -0.4999551463232377313, 0.8660512985181132439, 0.000000000000000000 ) ) ;
#36560 = CARTESIAN_POINT ( 'NONE',  ( 0.1484974224218250372, -0.8518925887318784529, 0.5179931425135368972 ) ) ;
#36561 = ADVANCED_FACE ( 'NONE', ( #27410 ), #26689, .F. ) ;
#36562 = CARTESIAN_POINT ( 'NONE',  ( 0.6010837949887281040, -1.596314856062887921, -0.5078772351678970676 ) ) ;
#36563 = CARTESIAN_POINT ( 'NONE',  ( 0.4676588494100126780, -1.684644990138186804, -0.6179151535550295726 ) ) ;
#36564 = CARTESIAN_POINT ( 'NONE',  ( 0.01548846960707528191, 0.3772621329472709006, 0.3651003739303413931 ) ) ;
#36565 = EDGE_CURVE ( 'NONE', #29923, #19133, #17387, .T. ) ;
#36566 = FACE_BOUND ( 'NONE', #28344, .T. ) ;
#36567 = AXIS2_PLACEMENT_3D ( 'NONE', #27048, #11410, #1779 ) ;
#36568 = CARTESIAN_POINT ( 'NONE',  ( 0.4909801108973092520, -1.199306193601649362, -0.5155029497116575543 ) ) ;
#36569 = CARTESIAN_POINT ( 'NONE',  ( 0.2292082634166116850, -1.390808673668628259, 1.038138609612698327 ) ) ;
#36570 = CARTESIAN_POINT ( 'NONE',  ( 0.3625898815820082222, -1.763258591188420210, -0.5925135466911359838 ) ) ;
#36571 = DIRECTION ( 'NONE',  ( -1.000000000000000000, -0.000000000000000000, -0.000000000000000000 ) ) ;
#36572 = CARTESIAN_POINT ( 'NONE',  ( 0.4399541867944170570, -1.702001723531057165, 0.6019985635216079656 ) ) ;
#36573 = VERTEX_POINT ( 'NONE', #30257 ) ;
#36574 = CARTESIAN_POINT ( 'NONE',  ( 0.4672376269229551182, -1.092478783799717856, -0.6267157269568994771 ) ) ;
#36575 = EDGE_CURVE ( 'NONE', #14323, #33695, #39324, .T. ) ;
#36576 = CARTESIAN_POINT ( 'NONE',  ( 0.3558549970762978076, -1.139915900499853585, 0.6174992432461627878 ) ) ;
#36577 = CARTESIAN_POINT ( 'NONE',  ( -0.1157923916715204865, -0.5295015842444287246, 0.1380392329925466954 ) ) ;
#36578 = APPLIED_DATE_AND_TIME_ASSIGNMENT ( #18486, #34533, ( #33155 ) ) ;
#36579 = CARTESIAN_POINT ( 'NONE',  ( -0.05082303569918699554, 0.3162776479886636460, -0.3525632866555268863 ) ) ;
#36580 = CARTESIAN_POINT ( 'NONE',  ( 0.4911901511437292700, -1.279438450280085293, 0.6967407287098164037 ) ) ;
#36582 = VERTEX_POINT ( 'NONE', #11144 ) ;
#36581 = CARTESIAN_POINT ( 'NONE',  ( -0.1628171590788805023, 0.5058980335669727157, 0.1333422639292590750 ) ) ;
#36583 = CARTESIAN_POINT ( 'NONE',  ( 0.4989999315605664343, -1.099494619349625113, 0.6223919996226902063 ) ) ;
#36584 = AXIS2_PLACEMENT_3D ( 'NONE', #22308, #27865, #18600 ) ;
#36585 = ORIENTED_EDGE ( 'NONE', *, *, #22686, .T. ) ;
#36586 = CARTESIAN_POINT ( 'NONE',  ( 0.1699918782215477098, -0.4775673823552313291, 0.1457287000202342475 ) ) ;
#36587 = VERTEX_POINT ( 'NONE', #26980 ) ;
#36588 = CARTESIAN_POINT ( 'NONE',  ( 0.05999999999999990757, 0.7171888913565960255, -0.2325238883388469069 ) ) ;
#36589 = CARTESIAN_POINT ( 'NONE',  ( 0.3562689543733437159, -1.622445070342072304, 0.5759800519041369249 ) ) ;
#36591 = CARTESIAN_POINT ( 'NONE',  ( -0.01895884884825222924, -0.3622979475331346566, 0.3730907371368802350 ) ) ;
#36590 = CARTESIAN_POINT ( 'NONE',  ( 0.7027426662857245709, -1.495553731087327254, 0.5003482327437285271 ) ) ;
#36592 = CARTESIAN_POINT ( 'NONE',  ( 0.000000000000000000, -0.1960639381401260983, -0.03948331496955503200 ) ) ;
#36593 = ORGANIZATION ( 'NAUO-ORG14', 'UNSPECIFIED', 'UNSPECIFIED' ) ;
#36594 = ORIENTED_EDGE ( 'NONE', *, *, #31662, .F. ) ;
#36595 = ORIENTED_EDGE ( 'NONE', *, *, #10148, .T. ) ;
#36596 = ORIENTED_EDGE ( 'NONE', *, *, #29831, .T. ) ;
#36597 = CARTESIAN_POINT ( 'NONE',  ( 0.1826134026666660082, -1.261648033191451246, 0.4282186462236582392 ) ) ;
#36598 = CYLINDRICAL_SURFACE ( 'NONE', #7961, 0.1550424246542357609 ) ;
#36599 = CARTESIAN_POINT ( 'NONE',  ( 0.1041408025812746996, -0.8666933816795890921, 0.4735943452512007545 ) ) ;
#36600 = CARTESIAN_POINT ( 'NONE',  ( 0.03113248654051816583, -0.3165425539888620521, -0.4137570037148034507 ) ) ;
#36601 = LINE ( 'NONE', #39889, #25988 ) ;
#36602 = B_SPLINE_CURVE_WITH_KNOTS ( 'NONE', 3,
 ( #34971, #37867, #9684, #35573 ),
 .UNSPECIFIED., .F., .F.,
 ( 4, 4 ),
 ( 0.000000000000000000, 0.001336189563664358891 ),
 .UNSPECIFIED. ) ;
#36603 = CARTESIAN_POINT ( 'NONE',  ( 0.3092347844015437830, -1.045386296435460549, 0.6288420117150920197 ) ) ;
#36604 = ADVANCED_FACE ( 'NONE', ( #36445 ), #11464, .F. ) ;
#36605 = DIRECTION ( 'NONE',  ( 0.000000000000000000, 0.000000000000000000, 1.000000000000000000 ) ) ;
#36606 = FACE_OUTER_BOUND ( 'NONE', #7682, .T. ) ;
#36607 = CARTESIAN_POINT ( 'NONE',  ( 0.1852718761952666104, -0.8389489029336036907, 0.1457185345930598341 ) ) ;
#36608 = CARTESIAN_POINT ( 'NONE',  ( 0.05217694232180475344, -1.283001185023028068, 0.6381678350426021051 ) ) ;
#36609 = COORDINATED_UNIVERSAL_TIME_OFFSET ( 0, 0, .AHEAD. ) ;
#36610 = EDGE_CURVE ( 'NONE', #8445, #13751, #7561, .T. ) ;
#36611 = CARTESIAN_POINT ( 'NONE',  ( 0.4393690858571965285, -1.132650523124447473, 0.4426054485940990046 ) ) ;
#36612 = EDGE_CURVE ( 'NONE', #51, #40488, #18878, .T. ) ;
#36613 = CARTESIAN_POINT ( 'NONE',  ( 0.4669612913469819437, -1.236553095564864035, 0.6057417262809811076 ) ) ;
#36614 = CARTESIAN_POINT ( 'NONE',  ( -0.02000000000000000042, -1.598492537578166672, -0.1971380022280825872 ) ) ;
#36615 = EDGE_LOOP ( 'NONE', ( #37126, #34914, #35983, #2934 ) ) ;
#36616 = LOCAL_TIME ( 0, 53, 7.000000000000000000, #9249 ) ;
#36617 = CARTESIAN_POINT ( 'NONE',  ( 1.097344326769410557E-05, -0.5478823044768206252, -0.07510365260775653251 ) ) ;
#36618 = LINE ( 'NONE', #10918, #31107 ) ;
#36619 = CARTESIAN_POINT ( 'NONE',  ( 0.0008453517450213650667, -0.4570859405462899816, 0.2529032369821648807 ) ) ;
#36620 = CARTESIAN_POINT ( 'NONE',  ( 0.04229956186878634783, 0.008769846780144823287, -0.4686106502047103217 ) ) ;
#36621 = ORIENTED_EDGE ( 'NONE', *, *, #33838, .T. ) ;
#36622 = ORIENTED_EDGE ( 'NONE', *, *, #22893, .F. ) ;
#36623 = EDGE_CURVE ( 'NONE', #15439, #27736, #38468, .T. ) ;
#36624 = CARTESIAN_POINT ( 'NONE',  ( 0.1767564091517300762, -0.5260537877495167214, 0.08939343933192094027 ) ) ;
#36625 = ORIENTED_EDGE ( 'NONE', *, *, #15767, .F. ) ;
#36626 = CARTESIAN_POINT ( 'NONE',  ( 0.1849096901904443147, -1.549205955729533235, 0.5682417262808779901 ) ) ;
#36627 = ADVANCED_FACE ( 'NONE', ( #868 ), #20918, .T. ) ;
#36628 = CARTESIAN_POINT ( 'NONE',  ( -0.1103620673373586075, -0.5040504500050040360, 0.1035024533007080916 ) ) ;
#36630 = EDGE_LOOP ( 'NONE', ( #32157, #28919 ) ) ;
#36629 = CARTESIAN_POINT ( 'NONE',  ( 0.001056708435954382790, -0.5892904156828951967, 0.01971284387651792494 ) ) ;
#36631 = ORIENTED_EDGE ( 'NONE', *, *, #20793, .F. ) ;
#36632 = CARTESIAN_POINT ( 'NONE',  ( -0.01548846960707524721, 0.000000000000000000, 0.000000000000000000 ) ) ;
#36633 = EDGE_LOOP ( 'NONE', ( #12636, #28178, #25029, #16438 ) ) ;
#36634 = CARTESIAN_POINT ( 'NONE',  ( -0.0009405724334786376211, -0.5506602586161217783, 0.2523206823539573262 ) ) ;
#36636 = CARTESIAN_POINT ( 'NONE',  ( 0.1361711851722846311, -1.247893485105676215, 0.6057349558209625950 ) ) ;
#36635 = DIRECTION ( 'NONE',  ( 0.000000000000000000, 0.000000000000000000, -1.000000000000000000 ) ) ;
#36637 = CARTESIAN_POINT ( 'NONE',  ( -0.05464101615137795936, -1.546789565643408526, -0.06332195561662121164 ) ) ;
#36638 = CARTESIAN_POINT ( 'NONE',  ( -0.05464101615137770263, -2.274798198814180772, -0.3601501197397404264 ) ) ;
#36640 = EDGE_LOOP ( 'NONE', ( #31273, #19831, #27238, #8298 ) ) ;
#36639 = ORIENTED_EDGE ( 'NONE', *, *, #30767, .F. ) ;
#36641 = CARTESIAN_POINT ( 'NONE',  ( -0.08000000000000000167, -1.772778095317936620, -0.3120197613628934441 ) ) ;
#36642 = CARTESIAN_POINT ( 'NONE',  ( -0.02000000000000000042, -2.183180860297908144, -0.4937760292030871079 ) ) ;
#36643 = B_SPLINE_SURFACE_WITH_KNOTS ( 'NONE', 3, 3, ( 
 ( #32758, #1323, #23335, #1738, #7673, #13829, #13636 ),
 ( #10977, #32960, #14250, #20424, #38933, #26402, #36246 ),
 ( #26203, #10765, #4560, #29679, #29895, #1525, #26812 ),
 ( #14041, #23719, #26619, #39152, #19622, #3965, #36464 ) ),
 .UNSPECIFIED., .F., .F., .F.,
 ( 4, 4 ),
 ( 4, 3, 4 ),
 ( 0.01293109825612811029, 0.01296195159122108011 ),
 ( 0.000000000000000000, 0.5039009682608166507, 1.007801936521633301 ),
 .UNSPECIFIED. ) ;
#36644 = CARTESIAN_POINT ( 'NONE',  ( 0.09318787492968771957, -0.5716158580642060061, 0.2615376999529335778 ) ) ;
#36645 =( BOUNDED_SURFACE ( )  B_SPLINE_SURFACE ( 3, 2, ( 
 ( #30233, #39704, #5325 ),
 ( #15216, #26959, #2676 ),
 ( #2283, #2483, #27772 ),
 ( #21614, #39492, #18107 ),
 ( #11537, #24102, #36628 ),
 ( #8844, #40312, #33733 ),
 ( #8431, #5546, #12141 ),
 ( #20996, #21421, #33954 ),
 ( #30454, #18312, #40096 ),
 ( #14822, #11731, #27387 ) ),
 .UNSPECIFIED., .F., .F., .T. ) 
 B_SPLINE_SURFACE_WITH_KNOTS ( ( 4, 2, 2, 2, 4 ),
 ( 3, 3 ),
 ( 0.001500576079630530895, 0.001976458225352494859, 0.002452340371074459256, 0.002928222516796423220, 0.003404104662518387184 ),
 ( 0.000000000000000000, 1.000000000000000000 ),
 .UNSPECIFIED. ) 
 GEOMETRIC_REPRESENTATION_ITEM ( )  RATIONAL_B_SPLINE_SURFACE ( (
 ( 1.000000000000000000, 0.9128709291753008825, 1.000000000000000000),
 ( 1.000000000000000000, 0.9128711300565840459, 1.000000000000000000),
 ( 1.000000000000000000, 0.9128295461285025336, 1.000000000000000000),
 ( 1.000000000000000000, 0.9126769222979866925, 1.000000000000000000),
 ( 1.000000000000000000, 0.9125696619634834361, 1.000000000000000000),
 ( 1.000000000000000000, 0.9123247991096318232, 1.000000000000000000),
 ( 1.000000000000000000, 0.9121939566646036779, 1.000000000000000000),
 ( 1.000000000000000000, 0.9119567588130496061, 1.000000000000000000),
 ( 1.000000000000000000, 0.9118559517119447788, 1.000000000000000000),
 ( 1.000000000000000000, 0.9117915798251980952, 1.000000000000000000) ) ) 
 REPRESENTATION_ITEM ( '' )  SURFACE ( )  );
#36646 = CARTESIAN_POINT ( 'NONE',  ( 0.1869677562307399121, -0.7232448055034852441, 0.03223249978197218618 ) ) ;
#36647 = CARTESIAN_POINT ( 'NONE',  ( -2.119743302583864240E-14, -2.107936428766274073, -0.7005084057759867200 ) ) ;
#36648 = FACE_OUTER_BOUND ( 'NONE', #1473, .T. ) ;
#36649 = CARTESIAN_POINT ( 'NONE',  ( 0.01220592763406190724, -0.4286278507047505681, 0.1569170967635542535 ) ) ;
#36650 = CARTESIAN_POINT ( 'NONE',  ( 0.4011294921376035161, -1.722319301493235644, 0.4257442406416360736 ) ) ;
#36651 = FACE_OUTER_BOUND ( 'NONE', #20548, .T. ) ;
#36652 = CARTESIAN_POINT ( 'NONE',  ( 0.1995529058109188070, -2.050896138459942009, -0.3054326997595750992 ) ) ;
#36653 = CARTESIAN_POINT ( 'NONE',  ( 0.000000000000000000, -0.3829990175980249600, -0.3390339253215535198 ) ) ;
#36654 = CARTESIAN_POINT ( 'NONE',  ( 0.3607508412325427516, -1.620744409234910144, -0.4217444633269712417 ) ) ;
#36655 = DIRECTION ( 'NONE',  ( 1.000000000000000000, 0.000000000000000000, 0.000000000000000000 ) ) ;
#36656 = ADVANCED_FACE ( 'NONE', ( #22448 ), #16720, .T. ) ;
#36657 = CARTESIAN_POINT ( 'NONE',  ( 0.2059273467974228333, -1.283046334493783025, -0.7462941026102624109 ) ) ;
#36658 = CARTESIAN_POINT ( 'NONE',  ( 0.005948235723147832048, -0.6142029534155015735, 0.3540208382306603840 ) ) ;
#36659 = CARTESIAN_POINT ( 'NONE',  ( 0.4241296934850513067, -1.044958113096912777, 0.6349482895397999815 ) ) ;
#36660 = CARTESIAN_POINT ( 'NONE',  ( 0.02180608606761921808, -0.9117970258225919222, 0.5599240550155194507 ) ) ;
#36661 = APPROVAL_STATUS ( 'not_yet_approved' ) ;
#36662 = CARTESIAN_POINT ( 'NONE',  ( 0.1875000000000003608, -0.4593131964907914422, 0.1498534765393862711 ) ) ;
#36663 = DIRECTION ( 'NONE',  ( 0.000000000000000000, 0.000000000000000000, -1.000000000000000000 ) ) ;
#36664 = FACE_OUTER_BOUND ( 'NONE', #2296, .T. ) ;
#36665 = CARTESIAN_POINT ( 'NONE',  ( 0.3577318113308060599, -1.744272611056911781, -0.4663113921787143124 ) ) ;
#36666 = ORIENTED_EDGE ( 'NONE', *, *, #6399, .F. ) ;
#36667 = CARTESIAN_POINT ( 'NONE',  ( -0.001495529303326669120, -0.9079788901573263571, 0.1457185332388704069 ) ) ;
#36668 = CARTESIAN_POINT ( 'NONE',  ( 0.09137532172571469213, -1.015574661215327579, 0.8525896866749620440 ) ) ;
#36669 = EDGE_CURVE ( 'NONE', #27130, #4891, #4893, .T. ) ;
#36670 = APPROVAL ( #21665, 'UNKNOWN' ) ;
#36671 = CARTESIAN_POINT ( 'NONE',  ( 0.1282560915798944823, -0.5581765241255676191, 0.1980671242072916116 ) ) ;
#36672 = CARTESIAN_POINT ( 'NONE',  ( 0.3815368266015244925, -1.759003287083134692, -0.4522571440127258202 ) ) ;
#36674 = ORIENTED_EDGE ( 'NONE', *, *, #26115, .T. ) ;
#36673 = CARTESIAN_POINT ( 'NONE',  ( 0.1874578000378240850, -0.6893444085712847613, 0.06304793604024336307 ) ) ;
#36675 = EDGE_CURVE ( 'NONE', #27427, #3365, #2948, .T. ) ;
#36676 = AXIS2_PLACEMENT_3D ( 'NONE', #38149, #19450, #16552 ) ;
#36677 = CARTESIAN_POINT ( 'NONE',  ( 0.6169573538504090626, -1.299218888095586388, 0.5469722621913530869 ) ) ;
#36679 = ORIENTED_EDGE ( 'NONE', *, *, #34045, .T. ) ;
#36678 = ORIENTED_EDGE ( 'NONE', *, *, #13909, .F. ) ;
#36680 = CARTESIAN_POINT ( 'NONE',  ( 0.001006207230660943319, -1.919904431792509136, -0.6546587980846723109 ) ) ;
#36681 = ORIENTED_EDGE ( 'NONE', *, *, #15299, .F. ) ;
#36682 = CARTESIAN_POINT ( 'NONE',  ( 0.3649706973909825347, -1.747755802025040328, -0.5186209711425785462 ) ) ;
#36683 = CARTESIAN_POINT ( 'NONE',  ( -0.1304423469995333318, -0.5262799683630392522, 0.3599999999999987654 ) ) ;
#36684 = DATE_TIME_ROLE ( 'classification_date' ) ;
#36685 = CARTESIAN_POINT ( 'NONE',  ( 0.5247602972291017798, -1.202859872010444198, 0.6057417262809816627 ) ) ;
#36686 = ORIENTED_EDGE ( 'NONE', *, *, #24785, .T. ) ;
#36687 = CARTESIAN_POINT ( 'NONE',  ( 0.000000000000000000, 0.000000000000000000, 0.000000000000000000 ) ) ;
#36688 = CARTESIAN_POINT ( 'NONE',  ( 0.2783032227094284772, -0.9886002588855364870, 0.7058132634711740128 ) ) ;
#36689 = CARTESIAN_POINT ( 'NONE',  ( 0.3167411566867828210, -1.686693824585019152, 0.8658616982602641565 ) ) ;
#36690 = CARTESIAN_POINT ( 'NONE',  ( 0.4713817688654168281, -1.488542902949906876, 0.7707858769014730438 ) ) ;
#36692 = CARTESIAN_POINT ( 'NONE',  ( 0.0006870102372341157582, -0.6133945797756367169, -0.005209209353789174407 ) ) ;
#36691 = CARTESIAN_POINT ( 'NONE',  ( 0.5938580047360285663, -1.599883625798725673, 0.4301333326164196169 ) ) ;
#36693 = CARTESIAN_POINT ( 'NONE',  ( 0.001265705468310253205, -0.9563107042206788755, 0.3108407331560245068 ) ) ;
#36694 = ORIENTED_EDGE ( 'NONE', *, *, #2660, .T. ) ;
#36695 = ORIENTED_EDGE ( 'NONE', *, *, #24615, .T. ) ;
#36696 = CARTESIAN_POINT ( 'NONE',  ( 0.05561176441985712926, -0.4442366066780392142, -0.1229089882096667807 ) ) ;
#36697 = CARTESIAN_POINT ( 'NONE',  ( 0.5806152853151792526, -1.240580746683077606, 0.8162131908780063672 ) ) ;
#36698 = CARTESIAN_POINT ( 'NONE',  ( -0.2399999999999999079, -2.183180860297908144, -1.015296970111275510 ) ) ;
#36699 = DIRECTION ( 'NONE',  ( 1.445848444424219201E-15, -1.000000000000000000, -2.361472542561095431E-16 ) ) ;
#36700 = EDGE_CURVE ( 'NONE', #13571, #25255, #31607, .T. ) ;
#36701 = PLANE ( 'NONE',  #26673 ) ;
#36702 = CARTESIAN_POINT ( 'NONE',  ( 0.4351352655241935152, -1.693421934718205124, -0.5229744562079222669 ) ) ;
#36703 = CARTESIAN_POINT ( 'NONE',  ( 0.3175074107031659598, -1.172635205199522801, 0.4853316727370740047 ) ) ;
#36704 = CARTESIAN_POINT ( 'NONE',  ( 0.1912825281910040254, -0.6944471949468554728, 0.2480975638430023278 ) ) ;
#36705 = CALENDAR_DATE ( 2026, 13, 10 ) ;
#36706 = DIRECTION ( 'NONE',  ( 0.3181970600707391683, -0.9480245940703956320, -2.369716614345735130E-16 ) ) ;
#36707 = CARTESIAN_POINT ( 'NONE',  ( 0.3638603365242920051, -1.988569641414750233, -0.6726323697083436137 ) ) ;
#36708 = CARTESIAN_POINT ( 'NONE',  ( 0.4568312001397978883, -1.218398625660269907, 0.5976199984034119561 ) ) ;
#36709 = DIRECTION ( 'NONE',  ( -1.387778780781449225E-15, 6.616194359655655447E-16, -1.000000000000000000 ) ) ;
#36710 = CARTESIAN_POINT ( 'NONE',  ( 0.3174184176267951796, -1.762933076790987874, 0.5319023928053561168 ) ) ;
#36711 = VERTEX_POINT ( 'NONE', #6997 ) ;
#36712 = DIRECTION ( 'NONE',  ( 0.4999551463232373427, -0.8660512985181134660, 0.000000000000000000 ) ) ;
#36713 = DIRECTION ( 'NONE',  ( 0.8660512985181135770, 0.4999551463232370652, 1.983296656985675225E-15 ) ) ;
#36714 = CARTESIAN_POINT ( 'NONE',  ( -0.05268850283020068415, 0.004611971649429206892, -0.4686124025367036650 ) ) ;
#36715 = CARTESIAN_POINT ( 'NONE',  ( 0.2263037797473776980, -1.351310894833297693, 0.5682417262808749925 ) ) ;
#36716 = EDGE_LOOP ( 'NONE', ( #36727, #16942, #33846, #28793 ) ) ;
#36717 = CARTESIAN_POINT ( 'NONE',  ( -0.02231181081520748968, 0.2417894035777240214, 0.4519954025055022973 ) ) ;
#36718 = CARTESIAN_POINT ( 'NONE',  ( -0.02000000000000000042, -2.041899626011815183, -0.6359449730384926225 ) ) ;
#36719 = CARTESIAN_POINT ( 'NONE',  ( 0.04047043078436212554, -0.4536058588506475808, -0.2133299978720243073 ) ) ;
#36720 = FACE_OUTER_BOUND ( 'NONE', #8389, .T. ) ;
#36721 = CARTESIAN_POINT ( 'NONE',  ( 0.3837573706890263781, -1.128755630749517680, 0.7040211244557138537 ) ) ;
#36722 = EDGE_CURVE ( 'NONE', #28751, #24257, #39697, .T. ) ;
#36724 = CARTESIAN_POINT ( 'NONE',  ( 0.2164394655998746198, -1.357183666387900667, 0.5509909139819678670 ) ) ;
#36723 = CARTESIAN_POINT ( 'NONE',  ( 0.04308449196698531380, 0.4845747790795011944, 0.09763455429601687607 ) ) ;
#36725 = DIRECTION ( 'NONE',  ( 0.000000000000000000, 0.000000000000000000, 1.000000000000000000 ) ) ;
#36726 = VERTEX_POINT ( 'NONE', #16460 ) ;
#36727 = ORIENTED_EDGE ( 'NONE', *, *, #38809, .T. ) ;
#36728 = DIRECTION ( 'NONE',  ( 0.000000000000000000, 0.000000000000000000, -1.000000000000000000 ) ) ;
#36729 = ORIENTED_EDGE ( 'NONE', *, *, #247, .F. ) ;
#36730 = FACE_OUTER_BOUND ( 'NONE', #3135, .T. ) ;
#36731 = CARTESIAN_POINT ( 'NONE',  ( 0.06043370286545072384, -0.5384506411558260819, 0.1542169419559350219 ) ) ;
#36733 = CARTESIAN_POINT ( 'NONE',  ( 0.1934695683574406411, -0.7446624497515935692, 0.3188077537673400519 ) ) ;
#36732 = CARTESIAN_POINT ( 'NONE',  ( 0.3288726549063353266, -1.639147087365691036, -0.4090903646187450948 ) ) ;
#36734 = CARTESIAN_POINT ( 'NONE',  ( 0.4236478467173229179, -1.144025187649157393, 0.4241618933158771698 ) ) ;
#36735 = ORIENTED_EDGE ( 'NONE', *, *, #7947, .F. ) ;
#36736 = VERTEX_POINT ( 'NONE', #23051 ) ;
#36737 = CARTESIAN_POINT ( 'NONE',  ( 0.3990412541384849576, -2.061965117970526951, -0.4759812377563777397 ) ) ;
#36738 = CARTESIAN_POINT ( 'NONE',  ( 0.4766810985275751200, -1.336280447492598222, 0.8178516970329706703 ) ) ;
#36739 = CARTESIAN_POINT ( 'NONE',  ( -2.112273405726188513E-14, -2.097675824466503691, -0.6968677163258658602 ) ) ;
#36740 = DIRECTION ( 'NONE',  ( -1.000000000000000000, -7.857794173099924470E-32, -8.628166150854818811E-32 ) ) ;
#36741 = FACE_OUTER_BOUND ( 'NONE', #9193, .T. ) ;
#36742 = CARTESIAN_POINT ( 'NONE',  ( 0.4368279861777726314, -1.677667223885754622, 0.4182417262808776348 ) ) ;
#36743 = CARTESIAN_POINT ( 'NONE',  ( 0.6413879784614744395, -1.405912376546664122, -0.6250000000000000000 ) ) ;
#36744 = PLANE ( 'NONE',  #27318 ) ;
#36745 = CARTESIAN_POINT ( 'NONE',  ( 0.7205914100055046401, -1.471989004879187490, 0.6461535000039996257 ) ) ;
#36746 = CARTESIAN_POINT ( 'NONE',  ( 0.3867386822597077001, -1.692088203187593898, -0.6206395857499010793 ) ) ;
#36747 = CARTESIAN_POINT ( 'NONE',  ( 0.01771465363353170661, -0.9865948873696219756, 0.4717780899493672075 ) ) ;
#36748 = CARTESIAN_POINT ( 'NONE',  ( 0.5959760379479978054, -1.584574879541716941, -0.6027336449407405539 ) ) ;
#36749 = CARTESIAN_POINT ( 'NONE',  ( 0.03318190567315884576, -1.808085944443767579, -0.6722552504361505310 ) ) ;
#36750 = CARTESIAN_POINT ( 'NONE',  ( 0.5767056209452497972, -1.613046407156268014, 0.5861331466064494400 ) ) ;
#36751 = CARTESIAN_POINT ( 'NONE',  ( -0.3000000000000000999, -4.394818335734379744, -0.8816972205720928768 ) ) ;
#36752 = DIRECTION ( 'NONE',  ( 1.000000000000000000, 1.450080480853946466E-15, -8.881784197001242463E-16 ) ) ;
#36753 = EDGE_LOOP ( 'NONE', ( #8964, #38189, #37635, #26409, #5401, #33231, #38964, #37129, #36061, #32732, #14556, #16430, #32327, #10731, #14389 ) ) ;
#36754 = CARTESIAN_POINT ( 'NONE',  ( 0.1826873925087639794, -0.5091858565627841449, 0.09782563527837608019 ) ) ;
#36755 = CARTESIAN_POINT ( 'NONE',  ( 0.4046838182303809650, -1.753375371334861654, -0.5898849750082092447 ) ) ;
#36756 = FACE_OUTER_BOUND ( 'NONE', #17623, .T. ) ;
#36757 = CARTESIAN_POINT ( 'NONE',  ( -0.07216878364870250862, 0.05141091571461216952, 0.1249999999999993477 ) ) ;
#36758 = EDGE_LOOP ( 'NONE', ( #33514, #31980, #21143, #19770 ) ) ;
#36759 = LINE ( 'NONE', #29790, #7281 ) ;
#36760 = CARTESIAN_POINT ( 'NONE',  ( 0.3504971479267370293, -1.161911706188821780, 0.5926884422481595305 ) ) ;
#36761 = CARTESIAN_POINT ( 'NONE',  ( 0.3247288286498336007, -1.767622216147507919, 0.5120194545848663070 ) ) ;
#36762 = CARTESIAN_POINT ( 'NONE',  ( -0.05634307799789460558, 0.2780413953411688399, -0.3652007531760524950 ) ) ;
#36763 = CARTESIAN_POINT ( 'NONE',  ( 0.4865585680422996884, -1.272250160645541195, 0.7024912634709812309 ) ) ;
#36765 = ORIENTED_EDGE ( 'NONE', *, *, #23537, .T. ) ;
#36764 = CARTESIAN_POINT ( 'NONE',  ( 0.2914323826288400254, -1.233685883474753497, -0.5166151207188711680 ) ) ;
#36766 = CARTESIAN_POINT ( 'NONE',  ( 0.4638997371337593156, -1.067608878195758448, 0.6494661525283214054 ) ) ;
#36767 = ORIENTED_EDGE ( 'NONE', *, *, #26009, .F. ) ;
#36768 = EDGE_CURVE ( 'NONE', #1061, #2531, #16902, .T. ) ;
#36769 = CARTESIAN_POINT ( 'NONE',  ( 0.05332459779802017213, -1.470191566866195121, -0.3710607107473925526 ) ) ;
#36770 = ORIENTED_EDGE ( 'NONE', *, *, #25584, .F. ) ;
#36771 = CARTESIAN_POINT ( 'NONE',  ( -0.03662792686184437874, 0.3149733899719671104, -0.3635662525351499585 ) ) ;
#36772 = CARTESIAN_POINT ( 'NONE',  ( 0.3349041316666306889, -1.546677854842905653, 0.8259521700164116353 ) ) ;
#36774 = CARTESIAN_POINT ( 'NONE',  ( 0.1148406439744575763, -0.4693285123388637459, 0.04216440238363276805 ) ) ;
#36773 = FACE_OUTER_BOUND ( 'NONE', #14328, .T. ) ;
#36775 = FACE_OUTER_BOUND ( 'NONE', #6723, .T. ) ;
#36776 = EDGE_CURVE ( 'NONE', #17453, #23598, #25721, .T. ) ;
#36777 = EDGE_LOOP ( 'NONE', ( #34907, #30809 ) ) ;
#36778 = CARTESIAN_POINT ( 'NONE',  ( 0.4855685666384785826, -1.075955829526442864, 0.6081528487602839705 ) ) ;
#36779 = ADVANCED_FACE ( 'NONE', ( #14184 ), #14796, .T. ) ;
#36780 = VERTEX_POINT ( 'NONE', #17066 ) ;
#36781 = FACE_OUTER_BOUND ( 'NONE', #10825, .T. ) ;
#36782 = LINE ( 'NONE', #27956, #15102 ) ;
#36783 = AXIS2_PLACEMENT_3D ( 'NONE', #37317, #6253, #12843 ) ;
#36784 = CARTESIAN_POINT ( 'NONE',  ( 0.1370286797637513543, -0.9213833723744169202, 0.6131078865398249533 ) ) ;
#36785 = CARTESIAN_POINT ( 'NONE',  ( 0.6473787150721044270, -1.455279521797666176, -0.6250000000000000000 ) ) ;
#36786 = DIRECTION ( 'NONE',  ( 0.4999551463232372317, -0.8660512985181133550, 0.000000000000000000 ) ) ;
#36787 = PERSON ( 'NAUO-PER6', 'UNSPECIFIED', 'UNSPECIFIED', ('UNSPECIFIED'), ('UNSPECIFIED'), ('UNSPECIFIED') ) ;
#36788 = CARTESIAN_POINT ( 'NONE',  ( 0.1192809747888602806, -0.9331602493862439784, 0.2873266990398272158 ) ) ;
#36789 = FACE_OUTER_BOUND ( 'NONE', #6370, .T. ) ;
#36790 = CARTESIAN_POINT ( 'NONE',  ( 0.3620892796180312234, -1.158480933315200634, 0.4329786855189595718 ) ) ;
#36791 = ADVANCED_FACE ( 'NONE', ( #5299 ), #26542, .T. ) ;
#36792 = CARTESIAN_POINT ( 'NONE',  ( 0.6568168297909239284, -1.515518412183779917, 0.4182417262808776903 ) ) ;
#36793 = DIRECTION ( 'NONE',  ( 1.000000000000000000, 0.000000000000000000, 0.000000000000000000 ) ) ;
#36794 = PERSON_AND_ORGANIZATION ( #28500, #32463 ) ;
#36795 = ORIENTED_EDGE ( 'NONE', *, *, #34096, .F. ) ;
#36796 = APPLIED_PERSON_AND_ORGANIZATION_ASSIGNMENT ( #2102, #18143, ( #19425 ) ) ;
#36797 = CARTESIAN_POINT ( 'NONE',  ( 0.4782576142078460157, -1.116195606080568448, 0.5342808753144958622 ) ) ;
#36798 = CARTESIAN_POINT ( 'NONE',  ( 0.5536047524870395531, -1.186371981408798737, 0.6057417262809813296 ) ) ;
#36799 = CARTESIAN_POINT ( 'NONE',  ( 0.5651833292478160020, -1.583037129094509998, -0.5461299182969832078 ) ) ;
#36800 = CARTESIAN_POINT ( 'NONE',  ( 2.603767063935397472E-05, -0.4515708911803948955, 0.03326049213652611247 ) ) ;
#36801 = CARTESIAN_POINT ( 'NONE',  ( 0.1399999999999994582, 0.000000000000000000, 0.000000000000000000 ) ) ;
#36802 = CARTESIAN_POINT ( 'NONE',  ( 0.0004750592482352814579, -0.4386115460793976739, 0.1457185332388683252 ) ) ;
#36803 = AXIS2_PLACEMENT_3D ( 'NONE', #40255, #5487, #24653 ) ;
#36804 = CARTESIAN_POINT ( 'NONE',  ( 0.4909801108973092520, -1.199306193601649362, -0.5155029497116575543 ) ) ;
#36805 = EDGE_LOOP ( 'NONE', ( #19926, #31758, #34752, #33592 ) ) ;
#36806 = ORIENTED_EDGE ( 'NONE', *, *, #34821, .F. ) ;
#36807 = CARTESIAN_POINT ( 'NONE',  ( -0.1124521194441415461, -0.5140518175048249816, 0.1111873348898669150 ) ) ;
#36808 = EDGE_LOOP ( 'NONE', ( #35235, #30576, #29297, #39533 ) ) ;
#36809 = DIRECTION ( 'NONE',  ( 0.4999551463232382309, -0.8660512985181127998, 1.639108796198564242E-15 ) ) ;
#36810 = DIRECTION ( 'NONE',  ( -1.000000000000000000, -2.341930812374887555E-31, 1.664003471950578127E-31 ) ) ;
#36812 = ORIENTED_EDGE ( 'NONE', *, *, #15748, .F. ) ;
#36811 = CARTESIAN_POINT ( 'NONE',  ( 0.001165796508395512297, -0.5811892146192374486, 0.02646226458924476332 ) ) ;
#36813 = EDGE_LOOP ( 'NONE', ( #26208, #37807, #31382, #17850, #18927, #37078, #22417, #26030, #30525 ) ) ;
#36814 = DIRECTION ( 'NONE',  ( 0.000000000000000000, 0.7071067811865474617, 0.7071067811865474617 ) ) ;
#36815 = ADVANCED_FACE ( 'NONE', ( #29613 ), #4258, .T. ) ;
#36816 = ORIENTED_EDGE ( 'NONE', *, *, #33303, .F. ) ;
#36817 = CARTESIAN_POINT ( 'NONE',  ( 0.2756304489896920229, -1.560360415575528403, 0.8591560916848097751 ) ) ;
#36818 = CARTESIAN_POINT ( 'NONE',  ( 0.1561163534220291194, -1.247536721834538564, 0.6205000180267052912 ) ) ;
#36819 = CARTESIAN_POINT ( 'NONE',  ( 0.6055916563817613785, -1.479479184092913790, 0.5526975506195442867 ) ) ;
#36820 = APPROVAL_ROLE ( '' ) ;
#36821 = EDGE_CURVE ( 'NONE', #34712, #3822, #35769, .T. ) ;
#36822 = EDGE_CURVE ( 'NONE', #38602, #32180, #36601, .T. ) ;
#36823 = EDGE_CURVE ( 'NONE', #30066, #29582, #7048, .T. ) ;
#36824 = DIRECTION ( 'NONE',  ( -1.188678714063517635E-15, 1.000000000000000000, 0.000000000000000000 ) ) ;
#36826 = ORIENTED_EDGE ( 'NONE', *, *, #15742, .T. ) ;
#36825 = ORIENTED_EDGE ( 'NONE', *, *, #39112, .T. ) ;
#36827 = EDGE_CURVE ( 'NONE', #30658, #5941, #2044, .T. ) ;
#36828 = CARTESIAN_POINT ( 'NONE',  ( 0.3311676996542577411, -1.172455566505741009, 0.5902003772419670558 ) ) ;
#36829 = CARTESIAN_POINT ( 'NONE',  ( -0.04085667396267264606, -0.4547700361314969131, 0.1255037944140869888 ) ) ;
#36830 = CARTESIAN_POINT ( 'NONE',  ( 0.3883702057743975145, -1.127429566525099069, 0.8010219123841900712 ) ) ;
#36831 = CARTESIAN_POINT ( 'NONE',  ( 0.1863214475076807042, -0.7675427701765082933, 0.04791228833432090856 ) ) ;
#36832 = LINE ( 'NONE', #8043, #13931 ) ;
#36833 = DIRECTION ( 'NONE',  ( -0.3468893892380655042, -0.7396492646828789486, -0.5767033179097537099 ) ) ;
#36834 = CARTESIAN_POINT ( 'NONE',  ( 0.3878387718074795543, -1.722808031660705508, -0.4381220887401267583 ) ) ;
#36835 = DIRECTION ( 'NONE',  ( 0.5495291984759871351, 0.000000000000000000, 0.8354745118926962810 ) ) ;
#36836 = DIRECTION ( 'NONE',  ( 5.551115123125718607E-17, 3.263080277421931478E-16, -1.000000000000000000 ) ) ;
#36837 = FACE_BOUND ( 'NONE', #7822, .T. ) ;
#36838 = CIRCLE ( 'NONE', #7938, 0.01000000000000002276 ) ;
#36839 = CARTESIAN_POINT ( 'NONE',  ( 0.4793488899164102257, -1.661214906270700453, 0.4177417262808786336 ) ) ;
#36840 = CARTESIAN_POINT ( 'NONE',  ( 0.4626267559758963643, -1.110960807299395503, 0.5629296282522621153 ) ) ;
#36841 = EDGE_CURVE ( 'NONE', #38334, #20390, #15460, .T. ) ;
#36842 = CARTESIAN_POINT ( 'NONE',  ( 0.3545087897290576384, -1.628856737622770723, -0.3716332584104992676 ) ) ;
#36843 =( CONVERSION_BASED_UNIT ( 'INCH', #2704 ) LENGTH_UNIT ( ) NAMED_UNIT ( #32274 ) );
#36844 = AXIS2_PLACEMENT_3D ( 'NONE', #11976, #15265, #34390 ) ;
#36845 = B_SPLINE_CURVE_WITH_KNOTS ( 'NONE', 3,
 ( #26747, #23659, #17863, #17268, #30211, #27144, #1660, #2042, #30428, #14183, #11099, #9028, #6335, #18288, #27744, #40071, #12509, #21589, #31030, #18081, #37598, #9213, #5518, #30635, #34312, #18907 ),
 .UNSPECIFIED., .F., .F.,
 ( 4, 2, 2, 2, 2, 2, 2, 2, 2, 2, 2, 2, 4 ),
 ( 0.007586643537693086789, 0.008316112212441773011, 0.009045580887190457497, 0.009775049561939141984, 0.01050451823668782821, 0.01196345558618519891, 0.01342239293568256962, 0.01634026763467730931, 0.01925814233367205419, 0.02217601703266679214, 0.02509389173166153703, 0.02801176643065627497, 0.03092964112965101986 ),
 .UNSPECIFIED. ) ;
#36846 = CIRCLE ( 'NONE', #10565, 0.1020173459747799466 ) ;
#36847 = CARTESIAN_POINT ( 'NONE',  ( 0.03303737228521855251, -0.2303602220530255040, 0.4672390599430960578 ) ) ;
#36848 = CARTESIAN_POINT ( 'NONE',  ( 0.1576987512544144876, -1.257723164589890308, 0.9396174402501648038 ) ) ;
#36849 = CARTESIAN_POINT ( 'NONE',  ( 0.04606810292053332284, -1.053385927643326392, 0.7216629152402889158 ) ) ;
#36850 = APPROVAL_ROLE ( '' ) ;
#36851 = CARTESIAN_POINT ( 'NONE',  ( 0.2954936729740054724, -0.7648845942614268534, 0.6619870385404000857 ) ) ;
#36852 = CARTESIAN_POINT ( 'NONE',  ( 0.6901651924715963560, -1.541509145059895447, 0.6010274064238112501 ) ) ;
#36853 = CARTESIAN_POINT ( 'NONE',  ( 0.03674078017396287255, 0.04075419261117436964, -0.4790519037776406197 ) ) ;
#36854 = VERTEX_POINT ( 'NONE', #33101 ) ;
#36855 = CARTESIAN_POINT ( 'NONE',  ( 0.05999999999999990757, -0.3497707857934448938, -0.3763954645181781244 ) ) ;
#36856 = ORIENTED_EDGE ( 'NONE', *, *, #17783, .F. ) ;
#36857 = DIRECTION ( 'NONE',  ( 1.000000000000000000, 6.779273404243070203E-32, 4.314083075427408311E-32 ) ) ;
#36858 = CARTESIAN_POINT ( 'NONE',  ( 0.06485312910877945314, -0.9239547295439671792, 0.7816216479469996203 ) ) ;
#36859 = AXIS2_PLACEMENT_3D ( 'NONE', #10888, #36166, #36369 ) ;
#36860 = CARTESIAN_POINT ( 'NONE',  ( 0.5475335553363155361, -1.432897008145440632, 0.7595943864330529927 ) ) ;
#36862 = VERTEX_POINT ( 'NONE', #4909 ) ;
#36861 = DIRECTION ( 'NONE',  ( 0.8660512985181135770, 0.4999551463232370097, 0.000000000000000000 ) ) ;
#36863 = AXIS2_PLACEMENT_3D ( 'NONE', #3932, #32129, #2779 ) ;
#36864 = APPLICATION_CONTEXT ( 'configuration controlled 3d designs of mechanical parts and assemblies' ) ;
#36865 = CARTESIAN_POINT ( 'NONE',  ( 0.2413003582545148740, -0.7023676887333554220, 0.5126316699731913173 ) ) ;
#36867 = ORIENTED_EDGE ( 'NONE', *, *, #21530, .T. ) ;
#36866 = ORIENTED_EDGE ( 'NONE', *, *, #20623, .T. ) ;
#36868 = CARTESIAN_POINT ( 'NONE',  ( 0.2540134399983700608, -0.7317239470612214580, 0.5469083470500127886 ) ) ;
#36869 = EDGE_CURVE ( 'NONE', #29183, #2065, #26631, .T. ) ;
#36870 = CIRCLE ( 'NONE', #26378, 0.04749999999977558285 ) ;
#36871 =( BOUNDED_SURFACE ( )  B_SPLINE_SURFACE ( 3, 2, ( 
 ( #19229, #37946, #9757 ),
 ( #31771, #3588, #6865 ),
 ( #19441, #31978, #27181 ),
 ( #2072, #29857, #23900 ) ),
 .UNSPECIFIED., .F., .F., .T. ) 
 B_SPLINE_SURFACE_WITH_KNOTS ( ( 4, 4 ),
 ( 3, 3 ),
 ( 0.01585912860563366486, 0.01610830113874010469 ),
 ( 0.000000000000000000, 0.04973070668175570697 ),
 .UNSPECIFIED. ) 
 GEOMETRIC_REPRESENTATION_ITEM ( )  RATIONAL_B_SPLINE_SURFACE ( (
 ( 1.000000000000000000, 0.9852470504322862199, 0.9719614500798579027),
 ( 1.000000000000000000, 0.9852431442513369664, 0.9719540262322374780),
 ( 1.000000000000000000, 0.9852393448778324903, 0.9719468053762871929),
 ( 1.000000000000000000, 0.9852356417021994606, 0.9719397673481035005) ) ) 
 REPRESENTATION_ITEM ( '' )  SURFACE ( )  );
#36872 = CARTESIAN_POINT ( 'NONE',  ( 0.6533741625928966013, -1.451818462565194201, -0.4117423987689379228 ) ) ;
#36873 = AXIS2_PLACEMENT_3D ( 'NONE', #6442, #21692, #19015 ) ;
#36874 = CARTESIAN_POINT ( 'NONE',  ( -0.1530923209794372852, 0.4738745695581291772, 0.09813923389054934887 ) ) ;
#36875 = ITEM_DEFINED_TRANSFORMATION ( 'NONE', 'NONE', #3575,  #27819 ) ;
#36876 = AXIS2_PLACEMENT_3D ( 'NONE', #26168, #31716, #3744 ) ;
#36877 = EDGE_CURVE ( 'NONE', #19496, #37899, #27147, .T. ) ;
#36878 = CARTESIAN_POINT ( 'NONE',  ( -0.01896968469604467730, 0.4667670904252209652, -0.2292592343991369241 ) ) ;
#36879 = ORIENTED_EDGE ( 'NONE', *, *, #11903, .T. ) ;
#36880 = ADVANCED_FACE ( 'NONE', ( #11511 ), #12477, .T. ) ;
#36881 = CARTESIAN_POINT ( 'NONE',  ( 0.1667190806935081038, -0.8308575925635335313, 0.5680044787289236785 ) ) ;
#36882 = CARTESIAN_POINT ( 'NONE',  ( 0.3190986850306563594, -1.698610481730714161, 0.8469447252347735988 ) ) ;
#36883 = CARTESIAN_POINT ( 'NONE',  ( 0.3509249258713971198, -1.204199599461771797, 0.8461177908718215956 ) ) ;
#36885 = CARTESIAN_POINT ( 'NONE',  ( 0.001991186333074667497, -0.5252647267804683162, 0.1020407222978734763 ) ) ;
#36884 = CARTESIAN_POINT ( 'NONE',  ( 0.6984663268742642428, -1.558725849730709934, -0.5155029497116575543 ) ) ;
#36886 = CARTESIAN_POINT ( 'NONE',  ( 0.04680495427436304895, -1.248529868540707355, 0.6559205912289112206 ) ) ;
#36887 = ORIENTED_EDGE ( 'NONE', *, *, #4116, .F. ) ;
#36888 = VERTEX_POINT ( 'NONE', #18084 ) ;
#36889 = CARTESIAN_POINT ( 'NONE',  ( -0.1684323895664678050, 0.5231977504175356897, 0.1528658435937002014 ) ) ;
#36890 = CARTESIAN_POINT ( 'NONE',  ( 0.4526194128954861284, -1.133629661972199054, 0.8947919898580423137 ) ) ;
#36891 = CARTESIAN_POINT ( 'NONE',  ( 0.1834964085430285941, -1.226715333008844055, -0.5155029497116575543 ) ) ;
#36892 = EDGE_CURVE ( 'NONE', #3309, #5909, #2974, .T. ) ;
#36893 = DIRECTION ( 'NONE',  ( 1.000000000000000000, 1.138269997360109379E-15, 0.000000000000000000 ) ) ;
#36894 = EDGE_CURVE ( 'NONE', #17501, #34890, #40498, .T. ) ;
#36895 = AXIS2_PLACEMENT_3D ( 'NONE', #20711, #30158, #33243 ) ;
#36896 = CARTESIAN_POINT ( 'NONE',  ( 0.3725772820214828807, -1.154817030518550780, 0.4257997613619559085 ) ) ;
#36897 = EDGE_CURVE ( 'NONE', #9709, #17150, #23758, .T. ) ;
#36898 = CARTESIAN_POINT ( 'NONE',  ( -5.013849553589398218E-05, -2.025592738939852033, -0.6748736259139497262 ) ) ;
#36899 = CARTESIAN_POINT ( 'NONE',  ( 0.3233135765761497304, -1.169465760711457358, 0.5638487597746312252 ) ) ;
#36900 = CARTESIAN_POINT ( 'NONE',  ( 0.5240142186908230970, -1.141661684775556296, 0.6661746706671649587 ) ) ;
#36901 = PERSON_AND_ORGANIZATION_ROLE ( 'creator' ) ;
#36902 = CIRCLE ( 'NONE', #19180, 0.07499999999999977518 ) ;
#36903 = CIRCLE ( 'NONE', #4705, 0.1600000000000000588 ) ;
#36904 = CARTESIAN_POINT ( 'NONE',  ( 0.01548846960721238578, -0.4730347584884322942, -0.2341461249027902980 ) ) ;
#36905 = AXIS2_PLACEMENT_3D ( 'NONE', #26253, #19665, #10601 ) ;
#36906 = CARTESIAN_POINT ( 'NONE',  ( 0.3648744522289030789, -2.000369472598153564, -0.6742880656426406549 ) ) ;
#36907 = DIRECTION ( 'NONE',  ( -7.771561172376107616E-16, 7.170354002788761615E-17, -1.000000000000000000 ) ) ;
#36908 = CARTESIAN_POINT ( 'NONE',  ( -0.1167294259372886750, -0.5331983348239501819, 0.3032895567580813356 ) ) ;
#36909 = VERTEX_POINT ( 'NONE', #28158 ) ;
#36910 = CYLINDRICAL_SURFACE ( 'NONE', #11514, 0.1033070866141732880 ) ;
#36911 = CARTESIAN_POINT ( 'NONE',  ( -0.03674260963082343762, -0.2486114773148977442, 0.4115095709379189559 ) ) ;
#36912 = CARTESIAN_POINT ( 'NONE',  ( -2.112273405726188513E-14, -2.107936428766274073, -0.2870436526301869962 ) ) ;
#36913 = ORIENTED_EDGE ( 'NONE', *, *, #12809, .T. ) ;
#36914 = CARTESIAN_POINT ( 'NONE',  ( -0.03672309138969848119, 0.04080728438229311306, -0.4790859898006342710 ) ) ;
#36915 = CARTESIAN_POINT ( 'NONE',  ( 0.01992777578774528394, -0.8806741340087591574, 0.4717011239932006328 ) ) ;
#36917 = EDGE_LOOP ( 'NONE', ( #31727, #17045, #38768 ) ) ;
#36916 = VERTEX_POINT ( 'NONE', #28350 ) ;
#36918 = DIRECTION ( 'NONE',  ( 0.8660512985181127998, 0.4999551463232382309, 0.000000000000000000 ) ) ;
#36919 = CARTESIAN_POINT ( 'NONE',  ( 0.04946288932099964647, 0.03516002272508091803, 0.4760097007310892248 ) ) ;
#36920 = CARTESIAN_POINT ( 'NONE',  ( 0.7433653656267760201, -1.515745490836327924, 0.5775132586956883696 ) ) ;
#36921 = CARTESIAN_POINT ( 'NONE',  ( 0.1994776429548950347, -2.045397862102978248, -0.3070066531183754388 ) ) ;
#36922 = CARTESIAN_POINT ( 'NONE',  ( 0.4616341473221652336, -1.227275536790998878, 0.6274102885783789940 ) ) ;
#36923 = CIRCLE ( 'NONE', #20522, 0.1333070866141733701 ) ;
#36924 = EDGE_CURVE ( 'NONE', #4721, #9760, #31106, .T. ) ;
#36926 = DIRECTION ( 'NONE',  ( -0.4999551463232372317, 0.8660512985181134660, -0.000000000000000000 ) ) ;
#36925 = PLANE ( 'NONE',  #6847 ) ;
#36927 = DIRECTION ( 'NONE',  ( 1.167933802921251313E-16, 0.9396926207859072067, -0.3420201433256720991 ) ) ;
#36928 = VERTEX_POINT ( 'NONE', #15190 ) ;
#36929 = ORIENTED_EDGE ( 'NONE', *, *, #30297, .T. ) ;
#36930 = ADVANCED_FACE ( 'NONE', ( #12117 ), #5773, .T. ) ;
#36931 = CARTESIAN_POINT ( 'NONE',  ( -0.2399999999999999079, -3.285933380171606188, -0.6294744526254049122 ) ) ;
#36932 = ORIENTED_EDGE ( 'NONE', *, *, #18291, .F. ) ;
#36933 = VECTOR ( 'NONE', #17709, 39.37007874015748854 ) ;
#36934 = CARTESIAN_POINT ( 'NONE',  ( 0.09701883858600784949, -1.253543889448050175, -0.5155029497116575543 ) ) ;
#36935 = CARTESIAN_POINT ( 'NONE',  ( 0.4127843276619986290, -1.589234977166629648, 0.5609238619371352819 ) ) ;
#36937 = CARTESIAN_POINT ( 'NONE',  ( -0.05464101615137787610, -2.183180860297908144, -0.4937760292030871079 ) ) ;
#36936 = CARTESIAN_POINT ( 'NONE',  ( -0.05283102792148739596, -0.4560693389104596429, 0.1064538768721983303 ) ) ;
#36938 = CARTESIAN_POINT ( 'NONE',  ( -0.05464101615137762630, -1.851224977018630868, -0.7958870385335591324 ) ) ;
#36939 = ORIENTED_EDGE ( 'NONE', *, *, #23589, .T. ) ;
#36940 = CARTESIAN_POINT ( 'NONE',  ( 0.3999835757944618098, -1.598096088517039437, -0.3114834528418581883 ) ) ;
#36941 = ORIENTED_EDGE ( 'NONE', *, *, #4728, .F. ) ;
#36942 = CARTESIAN_POINT ( 'NONE',  ( 0.4122953444515879418, -1.719325576034882674, -0.5258118692306196218 ) ) ;
#36943 = CARTESIAN_POINT ( 'NONE',  ( 0.1228162980791566161, -0.5684618713961013814, 0.2359394659365706692 ) ) ;
#36944 = CARTESIAN_POINT ( 'NONE',  ( 0.4714374192161987498, -1.680212440471048563, 0.4684164612439499775 ) ) ;
#36945 = CARTESIAN_POINT ( 'NONE',  ( 2.084605582574230847E-16, 0.2900000000000004241, -0.06434668806854136613 ) ) ;
#36946 = DIRECTION ( 'NONE',  ( -0.4999999999999985567, 0.2711473017028560029, 0.8224835200654551093 ) ) ;
#36947 = CARTESIAN_POINT ( 'NONE',  ( -0.6247879186461520185, 0.2375666616292472499, 0.08499999999999936773 ) ) ;
#36948 = LINE ( 'NONE', #30782, #34477 ) ;
#36949 = DIRECTION ( 'NONE',  ( -4.930380657631322689E-32, -0.7472307839325097456, -0.6645646360916346307 ) ) ;
#36950 = CARTESIAN_POINT ( 'NONE',  ( 0.1905506861939139096, -0.5145941129025596306, 0.2257199139534598609 ) ) ;
#36951 = CARTESIAN_POINT ( 'NONE',  ( -0.05616044724337349026, 0.2782405634116475457, 0.3655497896892119791 ) ) ;
#36952 = DIRECTION ( 'NONE',  ( 0.8660512985181134660, 0.4999551463232371762, 0.000000000000000000 ) ) ;
#36953 = VECTOR ( 'NONE', #14850, 39.37007874015748143 ) ;
#36954 = CARTESIAN_POINT ( 'NONE',  ( 0.6260944913943206069, -1.518023479389316810, -0.3975690101215826333 ) ) ;
#36955 = CARTESIAN_POINT ( 'NONE',  ( 0.08978098643734198914, 0.000000000000000000, 0.000000000000000000 ) ) ;
#36956 = LINE ( 'NONE', #31596, #23458 ) ;
#36957 = CARTESIAN_POINT ( 'NONE',  ( 0.02869712619511934765, 0.3396447909410104660, -0.3648221446286666336 ) ) ;
#36958 = CARTESIAN_POINT ( 'NONE',  ( 0.6011193747858227798, -1.595581932925101976, 0.4276689662439276396 ) ) ;
#36959 = AXIS2_PLACEMENT_3D ( 'NONE', #23879, #14381, #5311 ) ;
#36960 = AXIS2_PLACEMENT_3D ( 'NONE', #35798, #39092, #10915 ) ;
#36961 = ORIENTED_EDGE ( 'NONE', *, *, #35119, .F. ) ;
#36962 = CARTESIAN_POINT ( 'NONE',  ( 0.3659586724855932727, -1.748074482237940375, -0.5029264115039194794 ) ) ;
#36963 = CARTESIAN_POINT ( 'NONE',  ( 0.5003942916249191075, -1.540239132408833589, 0.5630373515401332352 ) ) ;
#36964 = AXIS2_PLACEMENT_3D ( 'NONE', #35978, #13752, #26136 ) ;
#36965 = CARTESIAN_POINT ( 'NONE',  ( 0.4495244212156574437, -1.660272750698808863, -0.6367136028539922554 ) ) ;
#36967 = VERTEX_POINT ( 'NONE', #6734 ) ;
#36966 = B_SPLINE_SURFACE_WITH_KNOTS ( 'NONE', 3, 1, ( 
 ( #10300, #35382 ),
 ( #19739, #29208 ),
 ( #1070, #26145 ),
 ( #38659, #10479 ),
 ( #23045, #35571 ),
 ( #16872, #10681 ),
 ( #667, #30255 ),
 ( #2087, #33538 ),
 ( #32942, #10957 ),
 ( #17318, #7837 ) ),
 .UNSPECIFIED., .F., .F., .F.,
 ( 4, 2, 2, 2, 4 ),
 ( 2, 2 ),
 ( -0.1094769316984412211, 0.2500000000000000000, 0.5000000000000000000, 0.7500000000000000000, 0.9999999728204846949 ),
 ( 0.000000000000000000, 1.000000000000000000 ),
 .UNSPECIFIED. ) ;
#36968 = DIRECTION ( 'NONE',  ( 0.000000000000000000, 0.000000000000000000, -1.000000000000000000 ) ) ;
#36969 = CONICAL_SURFACE ( 'NONE', #16664, 0.1600000000000000588, 1.047197551196602738 ) ;
#36970 = DIRECTION ( 'NONE',  ( -1.000000000000000000, -0.000000000000000000, -0.000000000000000000 ) ) ;
#36971 = CYLINDRICAL_SURFACE ( 'NONE', #29625, 0.09249999999977555343 ) ;
#36972 = CARTESIAN_POINT ( 'NONE',  ( 0.03875523708677872797, 0.2524014508497897102, -0.4040490413287913807 ) ) ;
#36973 = CARTESIAN_POINT ( 'NONE',  ( 0.4639166846825588664, -1.238161140430742213, 0.7208849079774189983 ) ) ;
#36975 = VERTEX_POINT ( 'NONE', #38618 ) ;
#36974 = CARTESIAN_POINT ( 'NONE',  ( -0.02000000000000000042, -2.070343076906777213, -0.2454056712452573896 ) ) ;
#36976 = CARTESIAN_POINT ( 'NONE',  ( 0.4793721953524077151, -1.080656662118478328, 0.6419491832934718367 ) ) ;
#36977 = ORIENTED_EDGE ( 'NONE', *, *, #37400, .T. ) ;
#36978 = APPROVAL_DATE_TIME ( #40054, #30992 ) ;
#36979 = DIRECTION ( 'NONE',  ( -7.771561172376097755E-16, -7.170354002788760383E-17, 1.000000000000000000 ) ) ;
#36980 = ORIENTED_EDGE ( 'NONE', *, *, #12180, .T. ) ;
#36981 = CARTESIAN_POINT ( 'NONE',  ( 0.3544495675655560118, -1.747437704060168739, -0.5520337568983563203 ) ) ;
#36982 = ORIENTED_EDGE ( 'NONE', *, *, #8406, .T. ) ;
#36983 = CARTESIAN_POINT ( 'NONE',  ( 0.09209597571042482667, -0.8538668600629184535, 0.7123787990913729162 ) ) ;
#36985 = CARTESIAN_POINT ( 'NONE',  ( 0.1124264983556580860, -0.7955156797634613808, -0.06988970266567862133 ) ) ;
#36984 = LINE ( 'NONE', #15390, #26992 ) ;
#36986 = DIRECTION ( 'NONE',  ( -1.000000000000000000, 0.000000000000000000, 0.000000000000000000 ) ) ;
#36987 = AXIS2_PLACEMENT_3D ( 'NONE', #10254, #9829, #439 ) ;
#36988 = ORIENTED_EDGE ( 'NONE', *, *, #30750, .T. ) ;
#36989 = CARTESIAN_POINT ( 'NONE',  ( 0.5067133256571466626, -1.119665319208750676, 0.6842747717451090894 ) ) ;
#36990 = CARTESIAN_POINT ( 'NONE',  ( 0.2241138682733187781, -0.8936256700826709087, 0.7043492929034889105 ) ) ;
#36991 = ORIENTED_EDGE ( 'NONE', *, *, #12947, .T. ) ;
#36992 = DIRECTION ( 'NONE',  ( 0.8660512985181134660, 0.4999551463232372317, 0.000000000000000000 ) ) ;
#36993 = DIRECTION ( 'NONE',  ( 0.4999999999999979461, 0.7980870686147867321, 0.3362395439413078391 ) ) ;
#36994 = AXIS2_PLACEMENT_3D ( 'NONE', #21603, #33719, #2269 ) ;
#36995 = DIRECTION ( 'NONE',  ( 0.000000000000000000, 0.000000000000000000, 1.000000000000000000 ) ) ;
#36996 = CARTESIAN_POINT ( 'NONE',  ( -0.1154414454259510697, -0.5279056935456387656, 0.3241024189951586254 ) ) ;
#36997 = B_SPLINE_CURVE_WITH_KNOTS ( 'NONE', 3,
 ( #15442, #31476, #18516, #22241, #2891, #38049, #3283 ),
 .UNSPECIFIED., .F., .F.,
 ( 4, 3, 4 ),
 ( 0.0001163120317926839576, 0.002539995921006134392, 0.003592109058172289482 ),
 .UNSPECIFIED. ) ;
#36998 = AXIS2_PLACEMENT_3D ( 'NONE', #32952, #30085, #4554 ) ;
#36999 = CARTESIAN_POINT ( 'NONE',  ( 0.3992403239432529283, -1.683235622436187073, -0.6263438071736542323 ) ) ;
#37000 = CARTESIAN_POINT ( 'NONE',  ( 0.6588957223800396834, -1.564199738096486714, 0.5197417262808792238 ) ) ;
#37001 = DIRECTION ( 'NONE',  ( 1.000000000000000000, 2.280301054154495132E-31, -1.664003471950577689E-31 ) ) ;
#37002 = AXIS2_PLACEMENT_3D ( 'NONE', #968, #7271, #31399 ) ;
#37003 = CARTESIAN_POINT ( 'NONE',  ( -0.005726188848608329551, -1.958868650540482870, -0.6583431953115838065 ) ) ;
#37004 = CARTESIAN_POINT ( 'NONE',  ( 0.05992090360963521489, -1.332693131100006978, 0.5682417262808777680 ) ) ;
#37005 = COORDINATED_UNIVERSAL_TIME_OFFSET ( 0, 0, .AHEAD. ) ;
#37006 = CARTESIAN_POINT ( 'NONE',  ( 0.4573173800065648553, -1.135161403414604475, 0.4529988214013289660 ) ) ;
#37007 = CARTESIAN_POINT ( 'NONE',  ( 0.3911537912183811194, -1.142124775201903475, 0.5563430366993925569 ) ) ;
#37008 = FACE_OUTER_BOUND ( 'NONE', #36758, .T. ) ;
#37009 = CARTESIAN_POINT ( 'NONE',  ( 0.0004467655297966004256, -0.4383329269132242856, 0.1340609614503255331 ) ) ;
#37010 = CARTESIAN_POINT ( 'NONE',  ( 0.3410366399252441338, -1.752216166167418043, 0.4548429336037024817 ) ) ;
#37011 = CIRCLE ( 'NONE', #19929, 0.1033070866141734129 ) ;
#37012 = CARTESIAN_POINT ( 'NONE',  ( 0.2209260011871197471, -1.309027873449325918, -0.6184399470714002645 ) ) ;
#37013 = CARTESIAN_POINT ( 'NONE',  ( 0.4186432780919984720, -1.612034538517055360, -0.6668481824684697745 ) ) ;
#37014 = EDGE_LOOP ( 'NONE', ( #11206, #30752, #2830, #22479 ) ) ;
#37015 = AXIS2_PLACEMENT_3D ( 'NONE', #3413, #6298, #590 ) ;
#37016 = ORIENTED_EDGE ( 'NONE', *, *, #38938, .F. ) ;
#37017 = AXIS2_PLACEMENT_3D ( 'NONE', #3685, #2870, #15420 ) ;
#37018 = CARTESIAN_POINT ( 'NONE',  ( -0.1044460467970231704, -0.4741855622371820567, 0.3602693341844405150 ) ) ;
#37019 = ORIENTED_EDGE ( 'NONE', *, *, #19527, .F. ) ;
#37020 = DIRECTION ( 'NONE',  ( 0.000000000000000000, 0.000000000000000000, -1.000000000000000000 ) ) ;
#37021 = CARTESIAN_POINT ( 'NONE',  ( -0.1399999999999997358, -6.881499428057815777E-16, -0.2526340763130725531 ) ) ;
#37023 = ORIENTED_EDGE ( 'NONE', *, *, #36827, .T. ) ;
#37022 = CARTESIAN_POINT ( 'NONE',  ( 0.001435883076814227933, -0.5530114004245914039, 0.04489778311629699648 ) ) ;
#37024 = AXIS2_PLACEMENT_3D ( 'NONE', #5316, #3081, #21412 ) ;
#37025 = EDGE_LOOP ( 'NONE', ( #27403, #33573, #7482, #30902, #13611, #33205 ) ) ;
#37026 = CARTESIAN_POINT ( 'NONE',  ( 0.1499999999999993561, 0.000000000000000000, 0.000000000000000000 ) ) ;
#37027 = VERTEX_POINT ( 'NONE', #25482 ) ;
#37028 = CIRCLE ( 'NONE', #21309, 0.04999999999999994726 ) ;
#37029 = EDGE_CURVE ( 'NONE', #1394, #35264, #3128, .T. ) ;
#37030 = CARTESIAN_POINT ( 'NONE',  ( 0.1207393138600422744, -1.069125492563510971, 0.8673586701997172410 ) ) ;
#37032 = CARTESIAN_POINT ( 'NONE',  ( 0.1438553286746209747, -1.251795828929518128, 0.6227151430034421065 ) ) ;
#37031 = CARTESIAN_POINT ( 'NONE',  ( 0.4309855169775498873, -1.223829803323659426, 0.6254704992157742449 ) ) ;
#37033 = APPLIED_PERSON_AND_ORGANIZATION_ASSIGNMENT ( #40263, #2833, ( #5625 ) ) ;
#37034 = FACE_OUTER_BOUND ( 'NONE', #10161, .T. ) ;
#37035 = DATE_AND_TIME ( #8032, #31975 ) ;
#37036 = CARTESIAN_POINT ( 'NONE',  ( -0.1707627412572580439, 0.4977336986496906923, 0.3126474374754089625 ) ) ;
#37038 = ORIENTED_EDGE ( 'NONE', *, *, #8223, .F. ) ;
#37037 = ORIENTED_EDGE ( 'NONE', *, *, #12200, .T. ) ;
#37039 = CARTESIAN_POINT ( 'NONE',  ( 0.3381111732067393350, -1.163545670492880157, 0.6012525635317799155 ) ) ;
#37040 = LINE ( 'NONE', #6380, #26715 ) ;
#37041 = CARTESIAN_POINT ( 'NONE',  ( -0.05252359774140081400, -0.4432374118283890496, 0.1535299757497308182 ) ) ;
#37042 = CARTESIAN_POINT ( 'NONE',  ( 0.3202918194079290015, -1.024799612382053970, 0.7687582342706213989 ) ) ;
#37043 = CARTESIAN_POINT ( 'NONE',  ( -0.3000000000000000999, -3.838583118162426810, -0.3058907208964237734 ) ) ;
#37044 = CARTESIAN_POINT ( 'NONE',  ( 0.2644847879712617367, -1.601187613148850719, 0.8339127871527183267 ) ) ;
#37045 = AXIS2_PLACEMENT_3D ( 'NONE', #27224, #19129, #12343 ) ;
#37046 = CARTESIAN_POINT ( 'NONE',  ( 0.08970986014245081741, -0.8451374409715517455, 0.8410174406224033561 ) ) ;
#37047 = DIRECTION ( 'NONE',  ( -0.9713176644646462909, -0.03533109781499667312, -0.2351461422735486029 ) ) ;
#37048 = CARTESIAN_POINT ( 'NONE',  ( 0.3499983029951591051, -1.626951647584141680, -0.6024333599963986874 ) ) ;
#37049 = VECTOR ( 'NONE', #33227, 39.37007874015748854 ) ;
#37050 = DIRECTION ( 'NONE',  ( 0.9848077530122080203, -0.1736481776669303589, 4.095352323445923521E-18 ) ) ;
#37051 = CARTESIAN_POINT ( 'NONE',  ( 0.3927915226382389657, -1.715293516864650147, 0.5707417262808793801 ) ) ;
#37052 = AXIS2_PLACEMENT_3D ( 'NONE', #22497, #3769, #34420 ) ;
#37053 = CARTESIAN_POINT ( 'NONE',  ( 0.4427491432746096800, -1.107282895871583905, 0.5823651115457876282 ) ) ;
#37054 = DIRECTION ( 'NONE',  ( 0.4999551463232372317, -0.8660512985181135770, 0.000000000000000000 ) ) ;
#37055 = CARTESIAN_POINT ( 'NONE',  ( -2.070754768975505034, -0.09959325338431362917, 0.3382895567580804230 ) ) ;
#37056 = ADVANCED_FACE ( 'NONE', ( #35340 ), #22206, .T. ) ;
#37057 = CARTESIAN_POINT ( 'NONE',  ( 0.2510700677566410910, -1.656657411791499168, 0.6264822711378978948 ) ) ;
#37058 = CARTESIAN_POINT ( 'NONE',  ( 0.03787118657716118109, -1.016424498358915018, 0.6950631583489912391 ) ) ;
#37059 = EDGE_CURVE ( 'NONE', #22890, #799, #13487, .T. ) ;
#37060 = COORDINATED_UNIVERSAL_TIME_OFFSET ( 0, 0, .AHEAD. ) ;
#37061 = CARTESIAN_POINT ( 'NONE',  ( 0.4715326458378593655, -1.065703591122391103, 0.8369151567944118630 ) ) ;
#37062 = AXIS2_PLACEMENT_3D ( 'NONE', #40594, #12413, #34017 ) ;
#37063 = EDGE_CURVE ( 'NONE', #20753, #9404, #19309, .T. ) ;
#37064 = ADVANCED_FACE ( 'NONE', ( #19102 ), #19902, .T. ) ;
#37065 = LINE ( 'NONE', #31317, #8323 ) ;
#37066 = ADVANCED_FACE ( 'NONE', ( #32440 ), #36475, .F. ) ;
#37067 = CARTESIAN_POINT ( 'NONE',  ( 0.03647060353175951564, 0.08366884794402459913, -0.5049308971818783354 ) ) ;
#37068 = ORIENTED_EDGE ( 'NONE', *, *, #8646, .F. ) ;
#37069 = CARTESIAN_POINT ( 'NONE',  ( 0.3435345990243335312, -1.649434886652794363, -0.4420678747786416785 ) ) ;
#37070 = ORIENTED_EDGE ( 'NONE', *, *, #9500, .T. ) ;
#37071 = DIRECTION ( 'NONE',  ( 0.4999999999999974465, -0.7980870686147877313, -0.3362395439413060072 ) ) ;
#37072 = CARTESIAN_POINT ( 'NONE',  ( 0.2215769352394466596, -1.475921142408890496, 0.9227110526898859577 ) ) ;
#37073 = AXIS2_PLACEMENT_3D ( 'NONE', #2941, #15494, #37475 ) ;
#37074 = CARTESIAN_POINT ( 'NONE',  ( 0.5879633267048641754, -1.491232175459922038, 0.5739096314268175014 ) ) ;
#37075 = VERTEX_POINT ( 'NONE', #3665 ) ;
#37076 = AXIS2_PLACEMENT_3D ( 'NONE', #3249, #32039, #9630 ) ;
#37077 = CARTESIAN_POINT ( 'NONE',  ( 0.6182635900321699074, -1.298039841913932513, 0.5932631914600888789 ) ) ;
#37079 = ORIENTED_EDGE ( 'NONE', *, *, #38643, .T. ) ;
#37078 = ORIENTED_EDGE ( 'NONE', *, *, #34821, .T. ) ;
#37080 = DIRECTION ( 'NONE',  ( 0.8660512985181132439, 0.4999551463232376203, 0.000000000000000000 ) ) ;
#37081 = CIRCLE ( 'NONE', #1632, 0.1249999999999999584 ) ;
#37082 = VECTOR ( 'NONE', #3431, 39.37007874015748143 ) ;
#37083 = CARTESIAN_POINT ( 'NONE',  ( 0.01548846960707528191, 0.2306506793134000532, -0.4716198300880355410 ) ) ;
#37084 = ADVANCED_FACE ( 'NONE', ( #29161 ), #9519, .F. ) ;
#37085 = APPROVAL_PERSON_ORGANIZATION ( #31703, #8891, #3522 ) ;
#37086 = CARTESIAN_POINT ( 'NONE',  ( 0.1734973056165641514, -1.209394307038482497, -0.5155029497116575543 ) ) ;
#37087 = CALENDAR_DATE ( 2026, 13, 10 ) ;
#37088 = ORIENTED_EDGE ( 'NONE', *, *, #4697, .F. ) ;
#37089 = CARTESIAN_POINT ( 'NONE',  ( 0.1385871437811476981, -0.7804196182993179409, 0.5000907977187665221 ) ) ;
#37090 = AXIS2_PLACEMENT_3D ( 'NONE', #7268, #1348, #17159 ) ;
#37091 = CARTESIAN_POINT ( 'NONE',  ( -0.08000000000000000167, -2.196538720661423749, -0.6552417777791260667 ) ) ;
#37092 = CARTESIAN_POINT ( 'NONE',  ( 0.1074718422060760153, -0.5843318630099050282, 0.2896000563418689722 ) ) ;
#37094 = FACE_OUTER_BOUND ( 'NONE', #28484, .T. ) ;
#37093 = CARTESIAN_POINT ( 'NONE',  ( 0.03113248654051816583, -3.491513147198971704E-33, 0.4614999999999880864 ) ) ;
#37095 = CARTESIAN_POINT ( 'NONE',  ( 0.02732781149695911321, -1.123547693055224173, 0.6558377280348957061 ) ) ;
#37096 = ORIENTED_EDGE ( 'NONE', *, *, #35309, .F. ) ;
#37097 = ORIENTED_EDGE ( 'NONE', *, *, #18734, .T. ) ;
#37098 = FACE_OUTER_BOUND ( 'NONE', #2249, .T. ) ;
#37099 = CARTESIAN_POINT ( 'NONE',  ( 0.5000143371095003841, -1.114760706755517639, 0.8117732093188116949 ) ) ;
#37100 = EDGE_CURVE ( 'NONE', #38078, #19390, #34927, .T. ) ;
#37102 = ADVANCED_FACE ( 'NONE', ( #39425 ), #18751, .T. ) ;
#37101 = CARTESIAN_POINT ( 'NONE',  ( -0.1339136704200473149, -0.4685718226220191851, 0.3606502365330780946 ) ) ;
#37103 = CARTESIAN_POINT ( 'NONE',  ( -0.05464101615137770263, -1.659335422034822205, 0.2169804935274544377 ) ) ;
#37104 = VECTOR ( 'NONE', #33033, 39.37007874015748143 ) ;
#37105 = DIRECTION ( 'NONE',  ( 0.000000000000000000, 0.000000000000000000, -1.000000000000000000 ) ) ;
#37106 = VECTOR ( 'NONE', #30123, 39.37007874015748143 ) ;
#37107 = CARTESIAN_POINT ( 'NONE',  ( 0.05496475644004305411, -1.465908258127670338, -0.6471173864664848674 ) ) ;
#37108 = CARTESIAN_POINT ( 'NONE',  ( 0.3415936387057808554, -1.158750661784961444, 0.4480089712593383622 ) ) ;
#37109 = B_SPLINE_CURVE_WITH_KNOTS ( 'NONE', 3,
 ( #34521, #12708, #25890, #3662 ),
 .UNSPECIFIED., .F., .F.,
 ( 4, 4 ),
 ( 0.0005090742087139675347, 0.0009526417881629593246 ),
 .UNSPECIFIED. ) ;
#37110 = CARTESIAN_POINT ( 'NONE',  ( 0.5214254866212318928, -1.138125297403113523, 0.6686424646332703725 ) ) ;
#37111 = CIRCLE ( 'NONE', #6883, 0.1946589359789743512 ) ;
#37112 = EDGE_CURVE ( 'NONE', #26563, #38515, #14779, .T. ) ;
#37113 = PERSON_AND_ORGANIZATION ( #28500, #32463 ) ;
#37114 = DIRECTION ( 'NONE',  ( -1.000000000000000000, -2.280301054154495132E-31, 1.664003471950577689E-31 ) ) ;
#37115 = LOCAL_TIME ( 0, 53, 7.000000000000000000, #21900 ) ;
#37116 = EDGE_CURVE ( 'NONE', #13556, #13794, #18282, .T. ) ;
#37117 = CARTESIAN_POINT ( 'NONE',  ( 0.3612352339526118117, -1.954411822542491128, -0.4945793958471655927 ) ) ;
#37118 = DIRECTION ( 'NONE',  ( 1.000000000000000000, 0.000000000000000000, 0.000000000000000000 ) ) ;
#37119 = EDGE_CURVE ( 'NONE', #38511, #38598, #17818, .T. ) ;
#37120 = VECTOR ( 'NONE', #35947, 39.37007874015748854 ) ;
#37121 = CARTESIAN_POINT ( 'NONE',  ( -0.02872242845530483327, -0.07817994906156928991, 0.5268390348591148742 ) ) ;
#37122 =( BOUNDED_SURFACE ( )  B_SPLINE_SURFACE ( 3, 2, ( 
 ( #37302, #11618, #18183 ),
 ( #27856, #28065, #14898 ),
 ( #9115, #20886, #18591 ),
 ( #34016, #34210, #11801 ),
 ( #30320, #2963, #36896 ),
 ( #5818, #14689, #8707 ) ),
 .UNSPECIFIED., .F., .F., .F. ) 
 B_SPLINE_SURFACE_WITH_KNOTS ( ( 4, 2, 4 ),
 ( 3, 3 ),
 ( -1.019150042136374168E-17, 0.0004951616201126806446, 0.0009903232402253714806 ),
 ( 0.000000000000000000, 1.000000000000000000 ),
 .UNSPECIFIED. ) 
 GEOMETRIC_REPRESENTATION_ITEM ( )  RATIONAL_B_SPLINE_SURFACE ( (
 ( 1.000000000000000000, 0.8170441014560104742, 1.000000000000000000),
 ( 1.000000000000000000, 0.8306458315206579623, 1.000000000000000000),
 ( 1.000000000000000000, 0.8330947640617497596, 1.000000000000000000),
 ( 1.000000000000000000, 0.8126093788735454515, 1.000000000000000000),
 ( 1.000000000000000000, 0.7896249599902737115, 1.000000000000000000),
 ( 1.000000000000000000, 0.7525568848367778507, 1.000000000000000000) ) ) 
 REPRESENTATION_ITEM ( '' )  SURFACE ( )  );
#37123 = ORIENTED_EDGE ( 'NONE', *, *, #2962, .T. ) ;
#37124 = CARTESIAN_POINT ( 'NONE',  ( 0.4564781620595781408, -1.137377641396571937, 0.4472515671891064692 ) ) ;
#37125 = CARTESIAN_POINT ( 'NONE',  ( -0.02953079040095600225, -0.3810518745593856060, 0.3687679460475811744 ) ) ;
#37126 = ORIENTED_EDGE ( 'NONE', *, *, #33520, .T. ) ;
#37127 = CARTESIAN_POINT ( 'NONE',  ( -0.04760454375020840151, 0.04300716520882287563, -0.4803168140823134702 ) ) ;
#37128 = CARTESIAN_POINT ( 'NONE',  ( 0.05817917803143683037, -1.018161828248461021, 0.7083252315212340555 ) ) ;
#37130 = ORIENTED_EDGE ( 'NONE', *, *, #5528, .T. ) ;
#37129 = ORIENTED_EDGE ( 'NONE', *, *, #769, .T. ) ;
#37131 = CARTESIAN_POINT ( 'NONE',  ( -2.115421433687637455E-14, -2.104525754108412805, -0.6992670217217592521 ) ) ;
#37132 = CARTESIAN_POINT ( 'NONE',  ( 0.04575106512774732015, 0.06504741310981214386, 0.4827780559048400755 ) ) ;
#37133 = EDGE_CURVE ( 'NONE', #5846, #12135, #32555, .T. ) ;
#37134 = CARTESIAN_POINT ( 'NONE',  ( 0.02881195911414813696, -0.4517660987406161843, -0.2100205058914844103 ) ) ;
#37135 = CARTESIAN_POINT ( 'NONE',  ( 0.3619118515909163780, -1.781044822011065731, -0.5264419442840763130 ) ) ;
#37136 = CIRCLE ( 'NONE', #36495, 0.04330708661417327632 ) ;
#37137 = CARTESIAN_POINT ( 'NONE',  ( 0.05999999999999990757, 0.8492681979939306069, -0.2138253033704805295 ) ) ;
#37139 = CARTESIAN_POINT ( 'NONE',  ( 0.2059273467974226113, -1.283046334493782359, -0.7462941026102624109 ) ) ;
#37138 = CARTESIAN_POINT ( 'NONE',  ( 0.02872242845530460428, 0.5252126300208033172, 0.08844866507292861724 ) ) ;
#37140 = DIRECTION ( 'NONE',  ( 0.8660512985181134660, 0.4999551463232372317, 0.000000000000000000 ) ) ;
#37141 = ORIENTED_EDGE ( 'NONE', *, *, #14680, .F. ) ;
#37142 = EDGE_CURVE ( 'NONE', #21612, #24566, #24022, .T. ) ;
#37143 = VECTOR ( 'NONE', #32840, 39.37007874015748143 ) ;
#37144 = DIRECTION ( 'NONE',  ( 0.000000000000000000, -1.000000000000000000, 0.000000000000000000 ) ) ;
#37145 = ORIENTED_EDGE ( 'NONE', *, *, #14163, .T. ) ;
#37146 = DIRECTION ( 'NONE',  ( 0.4999551463232372317, -0.8660512985181135770, 0.000000000000000000 ) ) ;
#37147 = CARTESIAN_POINT ( 'NONE',  ( 0.06872051704080016366, -0.6086765721664342266, 0.3652306837808803053 ) ) ;
#37149 = CARTESIAN_POINT ( 'NONE',  ( 0.5717393591038858469, -1.612291461392513003, 0.4730418959724068673 ) ) ;
#37148 = CARTESIAN_POINT ( 'NONE',  ( -0.2399999999999999079, -3.941790907013290823, -0.4709369376873030477 ) ) ;
#37150 = DIRECTION ( 'NONE',  ( 1.188678714063518227E-15, -1.000000000000000000, -3.263080277421930985E-16 ) ) ;
#37151 = CARTESIAN_POINT ( 'NONE',  ( -0.3000000000000000999, -3.941790907013290823, -0.2762780017083287243 ) ) ;
#37152 = PRODUCT_DEFINITION_FORMATION_WITH_SPECIFIED_SOURCE ( 'ANY', '', #13386, .NOT_KNOWN. ) ;
#37153 = ORIENTED_EDGE ( 'NONE', *, *, #34844, .T. ) ;
#37154 = DIRECTION ( 'NONE',  ( -1.000000000000000000, -6.779273404243070203E-32, -4.314083075427408311E-32 ) ) ;
#37155 = CARTESIAN_POINT ( 'NONE',  ( 0.3895534942183391247, -1.799872921755753641, -0.3127170998378249189 ) ) ;
#37156 = CARTESIAN_POINT ( 'NONE',  ( 0.1901246552320745298, -0.7774690835213511342, 0.5910184091100809667 ) ) ;
#37157 = AXIS2_PLACEMENT_3D ( 'NONE', #28014, #25538, #12171 ) ;
#37158 = CARTESIAN_POINT ( 'NONE',  ( 0.4796114828161345267, -1.675628263522580763, 0.4877750351082724700 ) ) ;
#37159 = CARTESIAN_POINT ( 'NONE',  ( -0.1743922129835729085, -0.5166151207188712791, 0.3599999999999990430 ) ) ;
#37160 = LINE ( 'NONE', #21122, #38920 ) ;
#37161 = DIRECTION ( 'NONE',  ( 0.000000000000000000, 0.000000000000000000, -1.000000000000000000 ) ) ;
#37162 = CARTESIAN_POINT ( 'NONE',  ( 0.6215274601157204648, -1.354888019438377444, -0.6250000000000000000 ) ) ;
#37163 = DIRECTION ( 'NONE',  ( 1.000000000000000000, -3.624433060062967676E-13, 2.563064096159671966E-12 ) ) ;
#37164 = CARTESIAN_POINT ( 'NONE',  ( 0.3043431798205027405, -0.7811398438223191576, 0.6771279187310788039 ) ) ;
#37165 = CARTESIAN_POINT ( 'NONE',  ( -0.04575334816097949980, 0.3363904506959767282, 0.3523376320073900447 ) ) ;
#37166 = CARTESIAN_POINT ( 'NONE',  ( 0.01534025463952351682, -0.9720854558541353052, 0.4214751749065498987 ) ) ;
#37167 = EDGE_CURVE ( 'NONE', #37390, #2983, #39237, .T. ) ;
#37168 = CARTESIAN_POINT ( 'NONE',  ( 0.6359077707932225820, -1.518635804457564520, -0.4166810063141049847 ) ) ;
#37169 = AXIS2_PLACEMENT_3D ( 'NONE', #17164, #4210, #26234 ) ;
#37170 = CARTESIAN_POINT ( 'NONE',  ( 0.03301162916267962738, 0.2303793641368860612, 0.4673060013142916191 ) ) ;
#37171 = PLANE ( 'NONE',  #17529 ) ;
#37172 = CARTESIAN_POINT ( 'NONE',  ( 0.2645503737337568939, -1.676379442750866477, 0.5604219075278777940 ) ) ;
#37173 = CYLINDRICAL_SURFACE ( 'NONE', #2210, 0.08000000000000000167 ) ;
#37174 = LOCAL_TIME ( 0, 53, 7.000000000000000000, #15058 ) ;
#37175 = ORIENTED_EDGE ( 'NONE', *, *, #13037, .T. ) ;
#37176 = CARTESIAN_POINT ( 'NONE',  ( 0.3656711388830471421, -1.748838986500312442, -0.5108124120186164907 ) ) ;
#37177 = CARTESIAN_POINT ( 'NONE',  ( 0.4676789493019616883, -1.559177855287317005, 0.5735223705611400824 ) ) ;
#37178 = CARTESIAN_POINT ( 'NONE',  ( 0.6531517882810622400, -1.470370464788490317, 0.4182417262808778013 ) ) ;
#37179 = CARTESIAN_POINT ( 'NONE',  ( 0.4568194025597909769, -1.686975086019319559, -0.6191628275868227282 ) ) ;
#37180 = CIRCLE ( 'NONE', #34539, 0.1400000000000013456 ) ;
#37181 = ORIENTED_EDGE ( 'NONE', *, *, #29068, .T. ) ;
#37182 = CARTESIAN_POINT ( 'NONE',  ( 0.5383773389028485568, -1.668462205496939132, -0.5443657938344932390 ) ) ;
#37183 = FACE_OUTER_BOUND ( 'NONE', #16938, .T. ) ;
#37184 = CARTESIAN_POINT ( 'NONE',  ( 0.4076976354719484830, -1.154888438488558267, 0.4282417262808775882 ) ) ;
#37185 = EDGE_CURVE ( 'NONE', #27340, #14, #35985, .T. ) ;
#37186 = CARTESIAN_POINT ( 'NONE',  ( 0.05634402396114654432, 0.2780622203583519858, -0.3651830615696467497 ) ) ;
#37187 = CARTESIAN_POINT ( 'NONE',  ( 0.4942211817909919480, -1.285256733056542977, 0.7126200490527264675 ) ) ;
#37188 = APPLIED_PERSON_AND_ORGANIZATION_ASSIGNMENT ( #17699, #24115, ( #38548 ) ) ;
#37190 = ORIENTED_EDGE ( 'NONE', *, *, #30272, .T. ) ;
#37189 = CARTESIAN_POINT ( 'NONE',  ( -0.05464101615137796630, -1.750394882718339762, -0.1142373872069606250 ) ) ;
#37191 = CARTESIAN_POINT ( 'NONE',  ( 0.2179926414509053834, -0.8923039640295803432, 0.4033837261968737375 ) ) ;
#37192 = ORIENTED_EDGE ( 'NONE', *, *, #37336, .T. ) ;
#37193 = ADVANCED_FACE ( 'NONE', ( #29563 ), #40599, .F. ) ;
#37194 = PERSON_AND_ORGANIZATION ( #28500, #32463 ) ;
#37195 = CARTESIAN_POINT ( 'NONE',  ( 5.505329350751969413E-16, -0.2899999999999994249, -0.07500000000000062172 ) ) ;
#37196 = VERTEX_POINT ( 'NONE', #30175 ) ;
#37197 = CARTESIAN_POINT ( 'NONE',  ( 0.03719017515162942322, -0.5647721775443517167, 0.2719657506221234144 ) ) ;
#37199 = CARTESIAN_POINT ( 'NONE',  ( 0.1758095078217830343, -0.7034033841566151857, -0.08419028408879647429 ) ) ;
#37198 = CARTESIAN_POINT ( 'NONE',  ( 0.06444297064315794576, -0.8352831487901670737, 0.1457185332388703236 ) ) ;
#37200 = DIRECTION ( 'NONE',  ( 0.8660512985181135770, 0.4999551463232370652, 1.983296656985675225E-15 ) ) ;
#37201 = EDGE_LOOP ( 'NONE', ( #37232, #15180, #25472, #39800 ) ) ;
#37202 = CIRCLE ( 'NONE', #16184, 0.1033070866141732325 ) ;
#37203 = CARTESIAN_POINT ( 'NONE',  ( 0.2813884797296905549, -1.026807924004586647, 0.6132444993518527676 ) ) ;
#37204 = CARTESIAN_POINT ( 'NONE',  ( 0.5527745311540036566, -1.511132050481931222, 0.5694627077227574219 ) ) ;
#37205 = ORIENTED_EDGE ( 'NONE', *, *, #9719, .F. ) ;
#37206 = CARTESIAN_POINT ( 'NONE',  ( 0.2933751793910955863, -1.495278175259627362, -0.3326461521471292260 ) ) ;
#37207 = DIRECTION ( 'NONE',  ( 0.8660512985181129109, 0.4999551463232381199, 0.000000000000000000 ) ) ;
#37208 = LOCAL_TIME ( 0, 53, 7.000000000000000000, #14880 ) ;
#37209 = LINE ( 'NONE', #21393, #40206 ) ;
#37210 = CARTESIAN_POINT ( 'NONE',  ( 0.3534309663918363542, -1.740588291835677870, -0.3303540215336857044 ) ) ;
#37211 = B_SPLINE_CURVE_WITH_KNOTS ( 'NONE', 3,
 ( #30033, #26941, #17869, #1861, #14375, #30434, #36395, #27367, #20786, #2262, #5113, #14801, #25281, #9426, #15195, #3072, #9035, #37604 ),
 .UNSPECIFIED., .F., .F.,
 ( 4, 2, 2, 2, 2, 2, 2, 2, 4 ),
 ( -0.003133633995111165162, -0.002350221109836696590, -0.001566808224562228451, -0.0007833953392877598780, 1.754598670826099105E-08, 0.0007834304312611764000, 0.001566843316535645406, 0.002350256201810114413, 0.003133669087084581684 ),
 .UNSPECIFIED. ) ;
#37212 = CIRCLE ( 'NONE', #39185, 0.03000000000000029379 ) ;
#37213 = CARTESIAN_POINT ( 'NONE',  ( 0.4211285406421715893, -1.688829255868648405, 0.4182417262808776903 ) ) ;
#37214 = CARTESIAN_POINT ( 'NONE',  ( 0.4815360835401190087, -1.665003689908300277, 0.5707417262808793801 ) ) ;
#37215 = CARTESIAN_POINT ( 'NONE',  ( -0.2399999999999999079, -4.385325017590463226, -0.5985264029706663935 ) ) ;
#37216 = CARTESIAN_POINT ( 'NONE',  ( 0.1593091913372683688, -1.385766485008658622, -0.6742091435302814961 ) ) ;
#37217 = CARTESIAN_POINT ( 'NONE',  ( 0.02666925540767700956, -1.119321828221852888, 0.6528166539191706530 ) ) ;
#37218 = APPROVAL_ROLE ( '' ) ;
#37219 = B_SPLINE_CURVE_WITH_KNOTS ( 'NONE', 3,
 ( #28379, #5184, #45, #31059, #34551, #37846, #12536, #34341, #34745, #6362, #27982, #18932, #9660, #462, #22229, #40522, #245, #28180 ),
 .UNSPECIFIED., .F., .F.,
 ( 4, 2, 2, 2, 2, 2, 2, 2, 4 ),
 ( 0.000000000000000000, 0.0007746617437634281808, 0.001549323487526856362, 0.002323985231290284434, 0.003098646975053712723, 0.003873308718817141012, 0.004647970462580568868, 0.005422632206343997591, 0.006197293950107425446 ),
 .UNSPECIFIED. ) ;
#37220 = EDGE_CURVE ( 'NONE', #17181, #31057, #29765, .T. ) ;
#37221 = CARTESIAN_POINT ( 'NONE',  ( 0.4787236986780760151, -1.118179508398265742, 0.5519777869597309872 ) ) ;
#37222 = CARTESIAN_POINT ( 'NONE',  ( 0.5245687263101824760, -1.202970462303446952, 0.6057417262809816627 ) ) ;
#37223 = DIRECTION ( 'NONE',  ( 8.881784197001246407E-16, -2.361472542561082612E-16, 1.000000000000000000 ) ) ;
#37224 = CARTESIAN_POINT ( 'NONE',  ( 0.04935217837593552231, -1.087446678362770758, 0.7326706496891072229 ) ) ;
#37225 = CARTESIAN_POINT ( 'NONE',  ( 0.05999999999999990757, -0.3829990175980249600, -0.3390339253215535198 ) ) ;
#37226 = CARTESIAN_POINT ( 'NONE',  ( 0.3088664963667261398, -1.757905065063135597, 0.5295467280985148850 ) ) ;
#37227 = VECTOR ( 'NONE', #36907, 39.37007874015748143 ) ;
#37228 = CARTESIAN_POINT ( 'NONE',  ( 0.3434711319545313835, -1.169169302084733797, 0.4182417262808776903 ) ) ;
#37229 = ORIENTED_EDGE ( 'NONE', *, *, #25802, .F. ) ;
#37230 = EDGE_LOOP ( 'NONE', ( #19884, #40567, #20895, #36480 ) ) ;
#37231 = CARTESIAN_POINT ( 'NONE',  ( -0.1123123235486435112, -0.5135423695149557988, 0.1325268268875357536 ) ) ;
#37232 = ORIENTED_EDGE ( 'NONE', *, *, #35885, .T. ) ;
#37233 = LOCAL_TIME ( 0, 53, 7.000000000000000000, #8245 ) ;
#37234 = DIRECTION ( 'NONE',  ( 0.8150167559926640992, 0.5794373887239191445, -1.138269997360107406E-15 ) ) ;
#37235 = CARTESIAN_POINT ( 'NONE',  ( 0.1499999999999993561, 0.000000000000000000, 0.000000000000000000 ) ) ;
#37236 = LINE ( 'NONE', #20809, #34809 ) ;
#37238 = VERTEX_POINT ( 'NONE', #1609 ) ;
#37237 = DIRECTION ( 'NONE',  ( 0.4999551463232372317, -0.8660512985181134660, 0.000000000000000000 ) ) ;
#37239 = VERTEX_POINT ( 'NONE', #14134 ) ;
#37240 = B_SPLINE_CURVE_WITH_KNOTS ( 'NONE', 3,
 ( #36451, #14026, #33356, #36040 ),
 .UNSPECIFIED., .F., .F.,
 ( 4, 4 ),
 ( 4.336808689942042773E-19, 0.0002303018524726760570 ),
 .UNSPECIFIED. ) ;
#37241 = DIRECTION ( 'NONE',  ( 1.000000000000000000, 2.280301054154495132E-31, -1.664003471950577689E-31 ) ) ;
#37242 = ORIENTED_EDGE ( 'NONE', *, *, #33421, .T. ) ;
#37243 = CARTESIAN_POINT ( 'NONE',  ( 0.2696218657953411424, -1.674929051967658733, 0.6230054160990766698 ) ) ;
#37245 = CARTESIAN_POINT ( 'NONE',  ( 0.08514104884741639789, -1.317777977354982921, 0.5631554082348806389 ) ) ;
#37244 = CARTESIAN_POINT ( 'NONE',  ( 0.1810495352127157176, -0.9167129548756171031, 0.6179360156744274635 ) ) ;
#37246 = FACE_OUTER_BOUND ( 'NONE', #12307, .T. ) ;
#37247 = CARTESIAN_POINT ( 'NONE',  ( 0.4131084440300917815, -1.709575418134248626, -0.4213477687306632080 ) ) ;
#37249 = EDGE_LOOP ( 'NONE', ( #21066, #5694, #39709, #25661 ) ) ;
#37248 = ORIENTED_EDGE ( 'NONE', *, *, #22056, .T. ) ;
#37250 = CARTESIAN_POINT ( 'NONE',  ( -0.2399999999999999079, -3.417177400252447317, -1.296093996387527758 ) ) ;
#37251 = CARTESIAN_POINT ( 'NONE',  ( 0.3631141027881771288, -1.729552718906028685, 0.4270090698524765527 ) ) ;
#37252 = CARTESIAN_POINT ( 'NONE',  ( 0.4751248519516730884, -1.681100737592190031, 0.5628962907142390781 ) ) ;
#37253 = CARTESIAN_POINT ( 'NONE',  ( 0.5049385406414879096, -1.338700766536453202, 0.8051606239926210051 ) ) ;
#37254 = DIRECTION ( 'NONE',  ( 1.000000000000000000, 0.000000000000000000, 0.000000000000000000 ) ) ;
#37255 = CARTESIAN_POINT ( 'NONE',  ( 0.2481470555835709191, -1.538569375340287371, 0.8889987892862927232 ) ) ;
#37256 = CARTESIAN_POINT ( 'NONE',  ( 0.3157029859671476313, -1.681686951297227894, 0.8731147540620630698 ) ) ;
#37257 = CIRCLE ( 'NONE', #1809, 0.6115209409081865388 ) ;
#37258 = CARTESIAN_POINT ( 'NONE',  ( 0.1999999999999789724, -2.183180860297921466, -0.4437760292030870635 ) ) ;
#37259 = CARTESIAN_POINT ( 'NONE',  ( 0.3914506609052950670, -1.712970798409825690, 0.5197417262808792238 ) ) ;
#37260 = CARTESIAN_POINT ( 'NONE',  ( 0.3336325236675090067, -1.050835064020409160, 0.7593003920438236021 ) ) ;
#37261 = CARTESIAN_POINT ( 'NONE',  ( -0.2399999999999999079, -3.647187793141847045, -0.4766722536777797115 ) ) ;
#37262 =( NAMED_UNIT ( * ) SI_UNIT ( $, .STERADIAN. ) SOLID_ANGLE_UNIT ( ) );
#37263 = CARTESIAN_POINT ( 'NONE',  ( 0.5953197980378833742, -1.599064723402610300, 0.4311035055375501135 ) ) ;
#37264 = CARTESIAN_POINT ( 'NONE',  ( 0.003142067210302413628, -0.5716151664902620055, 0.1991251360516817781 ) ) ;
#37265 = CARTESIAN_POINT ( 'NONE',  ( 0.06216260169285257875, -1.138180230654762815, 0.7527527421364956783 ) ) ;
#37266 = APPROVAL_ROLE ( '' ) ;
#37267 = CARTESIAN_POINT ( 'NONE',  ( 0.2232487200984690223, -0.6189500806901601093, 0.4773341886849224447 ) ) ;
#37268 = CARTESIAN_POINT ( 'NONE',  ( 0.05082303569918614206, -0.2375724430107425122, 0.4097459652473660063 ) ) ;
#37269 = CARTESIAN_POINT ( 'NONE',  ( 0.3460971044594531865, -1.678560363434771663, -0.4565776378744553221 ) ) ;
#37270 = ORIENTED_EDGE ( 'NONE', *, *, #19973, .T. ) ;
#37271 = DIRECTION ( 'NONE',  ( 0.4999999999999991118, 0.5755298573121168104, -0.6471208413753148925 ) ) ;
#37272 = CARTESIAN_POINT ( 'NONE',  ( 0.2601188121435625278, -1.607439648646116215, 0.8467017527915076114 ) ) ;
#37273 = CARTESIAN_POINT ( 'NONE',  ( 0.1286200154133211038, -0.5674997884473316212, 0.2294314527738028076 ) ) ;
#37275 = EDGE_LOOP ( 'NONE', ( #21375, #19988, #29947, #1241, #18387 ) ) ;
#37274 = DIRECTION ( 'NONE',  ( -0.4999551463232372317, 0.8660512985181135770, -0.000000000000000000 ) ) ;
#37276 = CARTESIAN_POINT ( 'NONE',  ( 0.5392338747517343434, -1.163405467613477295, 0.6464276897500325081 ) ) ;
#37278 = ORIENTED_EDGE ( 'NONE', *, *, #12521, .F. ) ;
#37277 = VERTEX_POINT ( 'NONE', #15563 ) ;
#37279 = CARTESIAN_POINT ( 'NONE',  ( 0.6498155928403246406, -1.464591312738813267, 0.4182417262808778013 ) ) ;
#37280 = CARTESIAN_POINT ( 'NONE',  ( 0.3707239397989903207, -1.673993377350394329, -0.6037758272379700752 ) ) ;
#37281 = CARTESIAN_POINT ( 'NONE',  ( -0.1552051794442721455, 0.4812910476514246083, 0.09878871670238423275 ) ) ;
#37282 = CYLINDRICAL_SURFACE ( 'NONE', #17201, 0.1033070866141732880 ) ;
#37283 = VERTEX_POINT ( 'NONE', #30981 ) ;
#37284 = EDGE_CURVE ( 'NONE', #652, #30726, #25639, .T. ) ;
#37285 = ADVANCED_FACE ( 'NONE', ( #8974 ), #21546, .F. ) ;
#37286 = CARTESIAN_POINT ( 'NONE',  ( 0.08735497562171311292, -0.7263075606618498714, 0.2000283160256591530 ) ) ;
#37287 = CIRCLE ( 'NONE', #551, 0.1033070866141734129 ) ;
#37288 = EDGE_CURVE ( 'NONE', #19496, #28467, #5464, .T. ) ;
#37289 = CARTESIAN_POINT ( 'NONE',  ( 0.3083686665179578568, -1.758089317276438024, 0.6134063284622075507 ) ) ;
#37290 = CARTESIAN_POINT ( 'NONE',  ( 0.5247960161509089838, -1.526737019399793116, 0.5659639212617542103 ) ) ;
#37292 = CARTESIAN_POINT ( 'NONE',  ( 0.06953952643797545186, -1.315567610428153511, 0.5260635157698690945 ) ) ;
#37291 = CARTESIAN_POINT ( 'NONE',  ( 0.3454273455000012594, -1.756874669286808466, 0.4564301676634069937 ) ) ;
#37293 = CARTESIAN_POINT ( 'NONE',  ( 0.08520462220341532000, -1.252311161969172026, 0.6441909309935092143 ) ) ;
#37294 = ORIENTED_EDGE ( 'NONE', *, *, #26093, .T. ) ;
#37295 = EDGE_CURVE ( 'NONE', #8335, #35903, #21378, .T. ) ;
#37296 = CARTESIAN_POINT ( 'NONE',  ( 0.4601907590469310194, -1.690464365935532731, 0.5857309660096694515 ) ) ;
#37297 = CARTESIAN_POINT ( 'NONE',  ( 0.5662013050271856862, -1.332134377766191147, 0.8879307549162257507 ) ) ;
#37298 = EDGE_CURVE ( 'NONE', #33631, #31055, #37765, .T. ) ;
#37299 = CARTESIAN_POINT ( 'NONE',  ( 0.01548846960712797240, 0.5203207976466739382, 0.08861466064782476393 ) ) ;
#37300 = CARTESIAN_POINT ( 'NONE',  ( -0.08408070219615466911, -0.09959325338431376795, 0.3600000000000005418 ) ) ;
#37301 = CYLINDRICAL_SURFACE ( 'NONE', #24538, 0.5400000000000017009 ) ;
#37302 = CARTESIAN_POINT ( 'NONE',  ( 0.4076976354719481499, -1.154888438488558711, 0.4182417262808778013 ) ) ;
#37303 = CARTESIAN_POINT ( 'NONE',  ( 0.01041184051585970598, -1.726097746008397493, -0.6357288279791224461 ) ) ;
#37304 = CARTESIAN_POINT ( 'NONE',  ( 0.3116101662948007611, -1.187661518757025192, 0.5454230041139144225 ) ) ;
#37305 = CARTESIAN_POINT ( 'NONE',  ( 0.4504611332311936889, -1.053473412190887304, 0.6915920958210214353 ) ) ;
#37306 = ADVANCED_BREP_SHAPE_REPRESENTATION ( '', ( #32173, #27819 ), #25262 ) ;
#37307 = CALENDAR_DATE ( 2026, 13, 10 ) ;
#37308 = CARTESIAN_POINT ( 'NONE',  ( 0.3560594290983791210, -1.794060577071256768, -0.5186890730419171369 ) ) ;
#37309 = ADVANCED_FACE ( 'NONE', ( #27700, #15351 ), #21341, .F. ) ;
#37310 = APPLIED_DATE_AND_TIME_ASSIGNMENT ( #29569, #35743, ( #11166 ) ) ;
#37311 = CARTESIAN_POINT ( 'NONE',  ( 0.3691383134885193318, -1.740927459917368303, -0.6793060835705189149 ) ) ;
#37312 = CARTESIAN_POINT ( 'NONE',  ( 0.5611986379937768943, -1.505946779369399025, 0.5603673003229301397 ) ) ;
#37313 = AXIS2_PLACEMENT_3D ( 'NONE', #5853, #30573, #8749 ) ;
#37314 = CARTESIAN_POINT ( 'NONE',  ( -1.019575837292305831, -0.04310840302198155199, 0.3750000000000002220 ) ) ;
#37315 = ORIENTED_EDGE ( 'NONE', *, *, #6864, .F. ) ;
#37316 = DIRECTION ( 'NONE',  ( -7.771561172376107616E-16, 7.170354002788761615E-17, -1.000000000000000000 ) ) ;
#37317 = CARTESIAN_POINT ( 'NONE',  ( 0.03113248654051816583, 0.000000000000000000, 0.000000000000000000 ) ) ;
#37318 = CARTESIAN_POINT ( 'NONE',  ( 0.1022213135577672433, -0.8207663499021961018, 0.3585070046201188076 ) ) ;
#37319 = VERTEX_POINT ( 'NONE', #5866 ) ;
#37320 = CARTESIAN_POINT ( 'NONE',  ( -0.05279185365593419554, 0.03990109708163099012, -0.4667311364329210233 ) ) ;
#37321 = CARTESIAN_POINT ( 'NONE',  ( 0.02220665151295753842, -1.035819085711241039, 0.7188228406368177836 ) ) ;
#37323 = ORIENTED_EDGE ( 'NONE', *, *, #18964, .T. ) ;
#37322 = ORIENTED_EDGE ( 'NONE', *, *, #10988, .T. ) ;
#37324 = SPHERICAL_SURFACE ( 'NONE', #13935, 0.01499999999999999944 ) ;
#37325 = ORIENTED_EDGE ( 'NONE', *, *, #4995, .T. ) ;
#37326 = CARTESIAN_POINT ( 'NONE',  ( 0.05999999999999990757, 9.785038312124675210E-34, 0.1499999999999990785 ) ) ;
#37327 = CARTESIAN_POINT ( 'NONE',  ( 0.7346172259536333238, -1.494169854247700657, 0.6985599367358283907 ) ) ;
#37328 = CARTESIAN_POINT ( 'NONE',  ( 0.1825460907816478517, -1.756676529110209994, -0.3560404930609161744 ) ) ;
#37329 = CARTESIAN_POINT ( 'NONE',  ( -0.2746410161513770931, -3.253611865733782693, -0.3464478357516359575 ) ) ;
#37331 = CARTESIAN_POINT ( 'NONE',  ( 0.2284780739230824753, -1.350302979228993117, 0.5370935808337153894 ) ) ;
#37330 = CARTESIAN_POINT ( 'NONE',  ( 0.05543910610525055321, 0.4446004295725627387, 0.1230574251923951118 ) ) ;
#37332 = CARTESIAN_POINT ( 'NONE',  ( -0.04293317454820666512, -0.3457449726441630400, -0.3536934093827145964 ) ) ;
#37333 = ORIENTED_EDGE ( 'NONE', *, *, #8277, .F. ) ;
#37334 = CARTESIAN_POINT ( 'NONE',  ( 0.1191520103465610603, -0.6496890496031613171, 0.4527207694524171822 ) ) ;
#37335 = VERTEX_POINT ( 'NONE', #2599 ) ;
#37336 = EDGE_CURVE ( 'NONE', #40066, #31681, #33186, .T. ) ;
#37337 = LINE ( 'NONE', #12639, #10861 ) ;
#37338 = CARTESIAN_POINT ( 'NONE',  ( 0.09827287832808975776, -0.6772034054173794448, 0.4837373503272690001 ) ) ;
#37340 = CARTESIAN_POINT ( 'NONE',  ( 0.5618478858959879974, -1.618700185366941824, 0.5182094704982558309 ) ) ;
#37339 = CARTESIAN_POINT ( 'NONE',  ( -0.04582889109739119587, -0.4389390569944067177, 0.2108010426992260600 ) ) ;
#37341 = CARTESIAN_POINT ( 'NONE',  ( -0.1157263453858490138, -0.4799749855354071837, 0.1178658435936994486 ) ) ;
#37342 = CARTESIAN_POINT ( 'NONE',  ( -0.2399999999999999079, -3.931184305295492898, -0.4815435394051006956 ) ) ;
#37343 = EDGE_CURVE ( 'NONE', #9543, #394, #1676, .T. ) ;
#37344 = DIRECTION ( 'NONE',  ( 1.000000000000000000, 1.517693329813468127E-15, -1.517693329813468127E-15 ) ) ;
#37345 = CARTESIAN_POINT ( 'NONE',  ( 0.3880982458546209934, -1.816572098790980805, -0.3121909403687748719 ) ) ;
#37346 = ADVANCED_FACE ( 'NONE', ( #8553 ), #2410, .T. ) ;
#37347 = CARTESIAN_POINT ( 'NONE',  ( 0.4273369639566782507, -1.239477052644316624, 0.8278212302127097022 ) ) ;
#37348 = CARTESIAN_POINT ( 'NONE',  ( 0.4875656111780362068, -1.659925035319771203, 0.5079328609705456854 ) ) ;
#37349 = FACE_OUTER_BOUND ( 'NONE', #20588, .T. ) ;
#37350 = EDGE_LOOP ( 'NONE', ( #34514, #5274, #5034, #33959 ) ) ;
#37351 = CYLINDRICAL_SURFACE ( 'NONE', #15291, 0.01500000000000001159 ) ;
#37352 = DIRECTION ( 'NONE',  ( 1.000000000000000000, 2.403560570595279103E-31, -1.725633230170969455E-31 ) ) ;
#37353 = DIRECTION ( 'NONE',  ( 0.000000000000000000, -0.9510565162951504226, 0.3090169943749569437 ) ) ;
#37354 = CARTESIAN_POINT ( 'NONE',  ( 0.2079659131559265517, -1.247001267129989710, 0.4467898267690011416 ) ) ;
#37355 = CARTESIAN_POINT ( 'NONE',  ( 0.5877184641988779656, -1.252861897328551022, 0.8491679911058225283 ) ) ;
#37356 =( BOUNDED_SURFACE ( )  B_SPLINE_SURFACE ( 3, 2, ( 
 ( #32543, #29466, #13816 ),
 ( #26387, #35842, #38914 ),
 ( #10745, #17116, #1508 ),
 ( #14023, #10961, #23522 ) ),
 .UNSPECIFIED., .F., .F., .F. ) 
 B_SPLINE_SURFACE_WITH_KNOTS ( ( 4, 4 ),
 ( 3, 3 ),
 ( 1.516581998872723602E-15, 0.0009752704012298402374 ),
 ( 0.000000000000000000, 1.000000000000000000 ),
 .UNSPECIFIED. ) 
 GEOMETRIC_REPRESENTATION_ITEM ( )  RATIONAL_B_SPLINE_SURFACE ( (
 ( 1.000000000000000000, 0.7101913118074566489, 1.000000000000000000),
 ( 1.000000000000000000, 0.7878845071931158683, 1.000000000000000000),
 ( 1.000000000000000000, 0.8401241550276493664, 1.000000000000000000),
 ( 1.000000000000000000, 0.8671479162383957107, 1.000000000000000000) ) ) 
 REPRESENTATION_ITEM ( '' )  SURFACE ( )  );
#37357 = CARTESIAN_POINT ( 'NONE',  ( -0.05076541221973871615, 0.2374623881706967587, 0.4099867295868513950 ) ) ;
#37358 = EDGE_CURVE ( 'NONE', #5090, #3536, #22747, .T. ) ;
#37359 = CARTESIAN_POINT ( 'NONE',  ( 0.01207181549175943662, -0.9514910684014844522, 0.2846013046921853640 ) ) ;
#37360 = CARTESIAN_POINT ( 'NONE',  ( -0.3000000000000000999, -3.941790907013290823, 0.1405840032208834911 ) ) ;
#37361 = CARTESIAN_POINT ( 'NONE',  ( 0.03025322876596520452, -1.914130172580563061, -0.6840549778904242428 ) ) ;
#37362 = CARTESIAN_POINT ( 'NONE',  ( 0.09705974031108312305, -0.8384972796398091344, 0.3241563970570177089 ) ) ;
#37363 = CARTESIAN_POINT ( 'NONE',  ( 0.2616322387702281205, -1.678013124025769187, 0.5382687897764735219 ) ) ;
#37364 = FACE_OUTER_BOUND ( 'NONE', #7690, .T. ) ;
#37365 = ORIENTED_EDGE ( 'NONE', *, *, #12510, .F. ) ;
#37366 = DIRECTION ( 'NONE',  ( 0.4908277074234744797, -0.8712566565745227809, 0.000000000000000000 ) ) ;
#37367 = CARTESIAN_POINT ( 'NONE',  ( 0.3864683547122780283, -1.712498712252804589, -0.5952922913290529250 ) ) ;
#37368 = CARTESIAN_POINT ( 'NONE',  ( 0.6542814889465385919, -1.462066692984673288, 0.4182417262808777458 ) ) ;
#37369 = DIRECTION ( 'NONE',  ( -1.000000000000000000, -1.119941574063613413E-31, 7.771561172376109588E-16 ) ) ;
#37370 = DIRECTION ( 'NONE',  ( 1.000000000000000000, 0.000000000000000000, 0.000000000000000000 ) ) ;
#37371 = ORIENTED_EDGE ( 'NONE', *, *, #7490, .T. ) ;
#37372 = DIRECTION ( 'NONE',  ( -8.881784197001246407E-16, 2.361472542561082612E-16, -1.000000000000000000 ) ) ;
#37373 = CARTESIAN_POINT ( 'NONE',  ( 0.3782063182305618887, -1.143311561251338260, 0.6049062659591731839 ) ) ;
#37374 = DIRECTION ( 'NONE',  ( -0.5000000000000012212, -0.7066258520834619583, -0.5006794435238177687 ) ) ;
#37375 = CARTESIAN_POINT ( 'NONE',  ( 0.03647060353175536618, 0.3644804546768194431, -0.3593183619073302415 ) ) ;
#37376 = CARTESIAN_POINT ( 'NONE',  ( 0.3862339994230782336, -1.129766223146394299, 0.7432368964524667110 ) ) ;
#37378 = ORIENTED_EDGE ( 'NONE', *, *, #8982, .F. ) ;
#37377 = DIRECTION ( 'NONE',  ( 2.532366176626897310E-12, -0.8090169943749517811, -0.5877852522924670309 ) ) ;
#37379 = CARTESIAN_POINT ( 'NONE',  ( 0.2007793764868952557, -0.8804627652107338553, 0.3298308470297674488 ) ) ;
#37380 = VERTEX_POINT ( 'NONE', #18641 ) ;
#37381 = APPROVAL_DATE_TIME ( #27728, #35281 ) ;
#37382 = CARTESIAN_POINT ( 'NONE',  ( 0.1014787326204109191, -1.381130074647918482, 0.6548904690729412392 ) ) ;
#37383 = ORIENTED_EDGE ( 'NONE', *, *, #23810, .T. ) ;
#37384 = ADVANCED_FACE ( 'NONE', ( #21126, #12458 ), #25012, .T. ) ;
#37385 = ORIENTED_EDGE ( 'NONE', *, *, #32069, .F. ) ;
#37386 = CARTESIAN_POINT ( 'NONE',  ( 0.04318205873092141600, -0.6066656042371337820, 0.3720294104896150755 ) ) ;
#37388 = CARTESIAN_POINT ( 'NONE',  ( 0.1849751083739534507, -0.8214528691028653018, 0.04641342327598888678 ) ) ;
#37387 = FACE_OUTER_BOUND ( 'NONE', #26842, .T. ) ;
#37389 = FACE_OUTER_BOUND ( 'NONE', #29552, .T. ) ;
#37390 = VERTEX_POINT ( 'NONE', #3202 ) ;
#37391 = EDGE_CURVE ( 'NONE', #4809, #22283, #40345, .T. ) ;
#37392 = ORIENTED_EDGE ( 'NONE', *, *, #32958, .T. ) ;
#37393 = ORIENTED_EDGE ( 'NONE', *, *, #2091, .F. ) ;
#37394 = CARTESIAN_POINT ( 'NONE',  ( 0.4724925770889458754, -1.066128429548910628, 0.6254527518579948708 ) ) ;
#37395 = CARTESIAN_POINT ( 'NONE',  ( 0.1549538013712574436, -0.7259076401328894423, 0.5372629092130595252 ) ) ;
#37396 = ORIENTED_EDGE ( 'NONE', *, *, #9894, .F. ) ;
#37397 = CARTESIAN_POINT ( 'NONE',  ( 0.2127719091618048841, -1.748736742968465485, -0.3547752604823448119 ) ) ;
#37398 = CARTESIAN_POINT ( 'NONE',  ( 0.6922159527011226832, -1.545014083134421901, -0.6250000000000000000 ) ) ;
#37399 = DIRECTION ( 'NONE',  ( 0.4379975771764363368, 0.000000000000000000, 0.8989761522907998570 ) ) ;
#37400 = EDGE_CURVE ( 'NONE', #26563, #3365, #36948, .T. ) ;
#37401 = CARTESIAN_POINT ( 'NONE',  ( -0.1068374249684430066, -0.4867512985519860114, 0.3606502370888305387 ) ) ;
#37402 = CARTESIAN_POINT ( 'NONE',  ( 0.4173132459375147874, -1.699444977922919042, 0.4182417262808778013 ) ) ;
#37403 = CARTESIAN_POINT ( 'NONE',  ( 0.3990191109500385025, -2.061617765760503485, -0.5133078562858378602 ) ) ;
#37404 = DIRECTION ( 'NONE',  ( -0.4887635750372997245, -0.8724162812079783169, 4.149599771362008055E-15 ) ) ;
#37405 = EDGE_CURVE ( 'NONE', #39909, #38544, #19405, .T. ) ;
#37406 = CARTESIAN_POINT ( 'NONE',  ( 0.07836034245246617513, -1.898373411144233192, -0.6535496771068961541 ) ) ;
#37407 = CARTESIAN_POINT ( 'NONE',  ( 1.365923996832131609E-16, -0.9481888444201345134, 0.1139263443108001761 ) ) ;
#37408 = COORDINATED_UNIVERSAL_TIME_OFFSET ( 0, 0, .AHEAD. ) ;
#37409 = EDGE_CURVE ( 'NONE', #27730, #12740, #28121, .T. ) ;
#37410 = CARTESIAN_POINT ( 'NONE',  ( 0.1916709472725509622, -0.9174159909098704713, 0.2459055916410233245 ) ) ;
#37411 = ADVANCED_FACE ( 'NONE', ( #26605 ), #40404, .T. ) ;
#37412 = CARTESIAN_POINT ( 'NONE',  ( 0.4690336016591764023, -1.116275788733601004, 0.5587719650776661329 ) ) ;
#37413 = DIRECTION ( 'NONE',  ( 0.8660512985181134660, 0.4999551463232372317, 0.000000000000000000 ) ) ;
#37414 = DIRECTION ( 'NONE',  ( -1.000000000000000000, 8.195543980992782950E-15, 0.000000000000000000 ) ) ;
#37415 = CARTESIAN_POINT ( 'NONE',  ( 0.1235390412447300995, -1.439500955437662766, 0.5982358349985300583 ) ) ;
#37416 = DIRECTION ( 'NONE',  ( 0.000000000000000000, 0.000000000000000000, -1.000000000000000000 ) ) ;
#37417 = CARTESIAN_POINT ( 'NONE',  ( 0.1989976604547370465, -2.047409678865564686, -0.7132172901365274598 ) ) ;
#37418 = CARTESIAN_POINT ( 'NONE',  ( 0.3980973275624947738, -1.734594076868668067, -0.5940246208459699639 ) ) ;
#37419 = ORIENTED_EDGE ( 'NONE', *, *, #9986, .F. ) ;
#37420 = ORIENTED_EDGE ( 'NONE', *, *, #36315, .F. ) ;
#37421 = DIRECTION ( 'NONE',  ( -7.771561172376107616E-16, 7.170354002788761615E-17, -1.000000000000000000 ) ) ;
#37422 = ORIENTED_EDGE ( 'NONE', *, *, #36610, .T. ) ;
#37423 = FACE_OUTER_BOUND ( 'NONE', #24756, .T. ) ;
#37424 = FACE_OUTER_BOUND ( 'NONE', #12956, .T. ) ;
#37425 = CARTESIAN_POINT ( 'NONE',  ( 0.5547482201398101775, -1.386539788442228582, 0.7573865583411005797 ) ) ;
#37428 = ORIENTED_EDGE ( 'NONE', *, *, #11878, .F. ) ;
#37427 = B_SPLINE_CURVE_WITH_KNOTS ( 'NONE', 3,
 ( #39009, #26882, #39227, #23199, #29362, #13525, #1595, #19892, #23804, #7535, #4446, #7742, #10845, #39414, #36121, #10426, #11232, #17008 ),
 .UNSPECIFIED., .F., .F.,
 ( 4, 2, 2, 2, 2, 2, 2, 2, 4 ),
 ( 5.275955480050202716E-18, 0.0003722442517452602536, 0.0007444885034905153031, 0.001116732755235770244, 0.001488977006981025185, 0.001861221258726280126, 0.002233465510471535284, 0.002605709762216790008, 0.002977954013962045166 ),
 .UNSPECIFIED. ) ;
#37426 = CARTESIAN_POINT ( 'NONE',  ( 0.3624061103390691096, -1.968824918581854932, -0.4968426515055719972 ) ) ;
#37429 = EDGE_LOOP ( 'NONE', ( #3803, #32354, #22644, #5678 ) ) ;
#37430 = CARTESIAN_POINT ( 'NONE',  ( 0.02869942827333582178, 0.4519168387192257219, -0.2102852866807453092 ) ) ;
#37431 = EDGE_LOOP ( 'NONE', ( #1791, #25875 ) ) ;
#37432 = CARTESIAN_POINT ( 'NONE',  ( 0.2484999103478700566, -1.477039049371299040, 0.9074785348539847751 ) ) ;
#37434 = CARTESIAN_POINT ( 'NONE',  ( 0.1089099196686046794, -1.297471296687298326, 0.5942357276382801423 ) ) ;
#37433 = CARTESIAN_POINT ( 'NONE',  ( 0.5025602611599372382, -1.689138731673214489, -0.4231169579026368144 ) ) ;
#37435 = CARTESIAN_POINT ( 'NONE',  ( 0.3840418824211426774, -1.145968873474952909, 0.4818701983608400519 ) ) ;
#37436 = SECURITY_CLASSIFICATION_LEVEL ( 'unclassified' ) ;
#37437 = ADVANCED_FACE ( 'NONE', ( #17121 ), #25301, .T. ) ;
#37438 = CARTESIAN_POINT ( 'NONE',  ( 0.4042633028792979033, -1.711240744073928122, 0.4220515681607882597 ) ) ;
#37440 = VERTEX_POINT ( 'NONE', #11152 ) ;
#37439 = ORIENTED_EDGE ( 'NONE', *, *, #23986, .F. ) ;
#37441 = EDGE_CURVE ( 'NONE', #528, #40154, #9968, .T. ) ;
#37442 = CARTESIAN_POINT ( 'NONE',  ( -0.2399999999999999079, -2.004945370031237850, -0.3367537423720109446 ) ) ;
#37443 = CARTESIAN_POINT ( 'NONE',  ( 0.3453377680719366127, -1.749458763706788433, 0.4498113177181519151 ) ) ;
#37444 = CARTESIAN_POINT ( 'NONE',  ( -0.04211812644076767115, -0.4433543613217511004, 0.1530385388104371636 ) ) ;
#37445 = CARTESIAN_POINT ( 'NONE',  ( 0.3891419541809565952, -1.130175006036680641, 0.7851655795637670909 ) ) ;
#37446 = CARTESIAN_POINT ( 'NONE',  ( 0.6985364634159124675, -1.438850461896725275, 0.5682400285031795617 ) ) ;
#37447 = DIRECTION ( 'NONE',  ( 0.000000000000000000, 0.000000000000000000, 1.000000000000000000 ) ) ;
#37448 = CARTESIAN_POINT ( 'NONE',  ( 0.01327203635574252319, -0.4607175675008980398, 0.2958762723741367728 ) ) ;
#37449 = DIRECTION ( 'NONE',  ( 0.000000000000000000, 0.000000000000000000, 1.000000000000000000 ) ) ;
#37450 = CARTESIAN_POINT ( 'NONE',  ( 0.7472913949145145729, -1.513305546476923613, 0.4177417262808786336 ) ) ;
#37451 = CARTESIAN_POINT ( 'NONE',  ( 2.174026239640920213E-15, -0.2949999999999994293, 0.06434668806853986733 ) ) ;
#37452 = CARTESIAN_POINT ( 'NONE',  ( 0.3695052819757340123, -1.758428263776099287, -0.4278193900811940176 ) ) ;
#37453 = DIRECTION ( 'NONE',  ( 0.7423354687179488653, 0.4285363217154147808, 0.5150676391057058545 ) ) ;
#37454 = TOROIDAL_SURFACE ( 'NONE', #32867, 0.5250000000000000222, 0.01499999999999999944 ) ;
#37455 = CARTESIAN_POINT ( 'NONE',  ( 0.04285640132274435438, -0.2295067898340903967, 0.4383690285535427056 ) ) ;
#37456 = CARTESIAN_POINT ( 'NONE',  ( 0.000000000000000000, -0.4262518876079541830, 0.1457185332388682419 ) ) ;
#37457 = CARTESIAN_POINT ( 'NONE',  ( 0.09217733281014239832, -1.307048935866454098, 0.7302822141201406048 ) ) ;
#37458 = CALENDAR_DATE ( 2026, 13, 10 ) ;
#37459 = CARTESIAN_POINT ( 'NONE',  ( 0.3679852976493193095, -0.8933044249262621639, 0.7616870389678419562 ) ) ;
#37460 = LINE ( 'NONE', #9277, #12669 ) ;
#37461 = DIRECTION ( 'NONE',  ( -0.4999999999999962252, -0.8615295495183339369, -0.08812965055383011059 ) ) ;
#37462 = CARTESIAN_POINT ( 'NONE',  ( 0.3453377680719361131, -1.749458763706787545, 0.4498113177181523037 ) ) ;
#37463 = CARTESIAN_POINT ( 'NONE',  ( -0.1873388932668317575, 0.5325605939836577374, 0.3749999999999990008 ) ) ;
#37464 = ORIENTED_EDGE ( 'NONE', *, *, #23807, .F. ) ;
#37465 = CARTESIAN_POINT ( 'NONE',  ( 0.4752104778612297187, -1.162234221663497546, -0.6186948529734399571 ) ) ;
#37466 = CARTESIAN_POINT ( 'NONE',  ( 0.2629916659223787145, -1.620021443655322857, 0.8311813128113193505 ) ) ;
#37467 = CARTESIAN_POINT ( 'NONE',  ( 0.5949976145935880201, -1.487201548628922954, 0.5742703033084610720 ) ) ;
#37469 = ORIENTED_EDGE ( 'NONE', *, *, #10016, .T. ) ;
#37468 = CARTESIAN_POINT ( 'NONE',  ( 0.03113248654051816583, 0.8492681979939306069, -0.2138253033704803907 ) ) ;
#37470 = CARTESIAN_POINT ( 'NONE',  ( 0.1874999999999996669, -0.6872203660140437931, 0.1457185332388695742 ) ) ;
#37472 = ORIENTED_EDGE ( 'NONE', *, *, #7614, .T. ) ;
#37471 = ORIENTED_EDGE ( 'NONE', *, *, #7554, .T. ) ;
#37473 = CARTESIAN_POINT ( 'NONE',  ( -0.02953079040095700838, 0.000000000000000000, 0.000000000000000000 ) ) ;
#37474 = CARTESIAN_POINT ( 'NONE',  ( 0.3425232517505406027, -1.682473151710080606, -0.5664509581880096123 ) ) ;
#37475 = DIRECTION ( 'NONE',  ( 1.000000000000000000, 0.000000000000000000, 0.000000000000000000 ) ) ;
#37476 = ITEM_DEFINED_TRANSFORMATION ( 'NONE', 'NONE', #18026,  #27819 ) ;
#37477 = AXIS2_PLACEMENT_3D ( 'NONE', #12432, #18832, #24984 ) ;
#37478 = CARTESIAN_POINT ( 'NONE',  ( -0.3000000000000000999, -3.667123564397057667, -0.3682398926280779361 ) ) ;
#37479 = VERTEX_POINT ( 'NONE', #11570 ) ;
#37480 = CARTESIAN_POINT ( 'NONE',  ( 0.1145648225167921752, -0.8006048646630788967, 0.4136033892511831733 ) ) ;
#37481 = CARTESIAN_POINT ( 'NONE',  ( 0.3779802290120621855, -1.643891170928071910, -0.3923847609905750655 ) ) ;
#37482 = TOROIDAL_SURFACE ( 'NONE', #13204, 0.5250000000000000222, 0.01499999999999999944 ) ;
#37483 = CARTESIAN_POINT ( 'NONE',  ( 0.4182384646632246183, -1.335901635285643207, 0.8423281896759605702 ) ) ;
#37484 = CARTESIAN_POINT ( 'NONE',  ( 0.6315454839751819538, -1.614677985460544640, -0.5441907603680019578 ) ) ;
#37485 = CARTESIAN_POINT ( 'NONE',  ( -0.04293317454820668594, -0.2295413494973332635, 0.4381202835071946189 ) ) ;
#37486 = ORIENTED_EDGE ( 'NONE', *, *, #16737, .T. ) ;
#37487 = CIRCLE ( 'NONE', #38806, 0.1033070866141732325 ) ;
#37488 = DIRECTION ( 'NONE',  ( -0.8660512985181132439, -0.4999551463232377313, 0.000000000000000000 ) ) ;
#37489 = CARTESIAN_POINT ( 'NONE',  ( 0.7441752718225284058, -1.515794030150653837, 0.5954587793138176322 ) ) ;
#37490 = CARTESIAN_POINT ( 'NONE',  ( 0.1135262681040088983, -1.415870350120112864, 0.5684114953092351818 ) ) ;
#37491 = CARTESIAN_POINT ( 'NONE',  ( -0.1608542991165662073, 0.4995867522469580324, 0.3503927954982321569 ) ) ;
#37492 = CARTESIAN_POINT ( 'NONE',  ( 0.2318589737339854795, -1.232498520698479982, 0.5197417262808780025 ) ) ;
#37493 = B_SPLINE_CURVE_WITH_KNOTS ( 'NONE', 3,
 ( #24810, #5657, #24603, #15542, #11829, #40006 ),
 .UNSPECIFIED., .F., .F.,
 ( 4, 2, 4 ),
 ( 0.000000000000000000, 0.5000000000000000000, 1.000000000000000000 ),
 .UNSPECIFIED. ) ;
#37494 = CARTESIAN_POINT ( 'NONE',  ( -0.02000000000000000042, -1.845925619402022155, -0.3444148183989317880 ) ) ;
#37495 = CARTESIAN_POINT ( 'NONE',  ( 0.08096179802327445330, -1.367098532309424685, 0.5880770290185818316 ) ) ;
#37496 = CARTESIAN_POINT ( 'NONE',  ( 0.5265921910155209051, -1.145228776028037521, 0.6635139613180396356 ) ) ;
#37497 = PRODUCT_CONTEXT ( 'NONE', #28459, 'mechanical' ) ;
#37498 = CARTESIAN_POINT ( 'NONE',  ( 0.3590472838652598031, -1.925292734864337829, -0.5030625321385080451 ) ) ;
#37499 = CIRCLE ( 'NONE', #31614, 0.01500000000000002894 ) ;
#37500 = CARTESIAN_POINT ( 'NONE',  ( 0.3920817863706622663, -1.709816463946002063, 0.4185791750296219416 ) ) ;
#37501 = CARTESIAN_POINT ( 'NONE',  ( -0.05186792262757373290, -0.01796889665935117592, 0.4704835727131218004 ) ) ;
#37502 = CIRCLE ( 'NONE', #5287, 0.02999999999999997113 ) ;
#37503 = ORIENTED_EDGE ( 'NONE', *, *, #30529, .T. ) ;
#37504 = CARTESIAN_POINT ( 'NONE',  ( 0.4159916692016358830, -1.069406866067976081, -0.5155029497116575543 ) ) ;
#37505 = DIRECTION ( 'NONE',  ( 1.000000000000000000, 2.280301054154495132E-31, -1.664003471950577689E-31 ) ) ;
#37507 = B_SPLINE_CURVE_WITH_KNOTS ( 'NONE', 3,
 ( #21958, #15970, #16372, #393, #18870, #12891, #6692, #19472, #35300, #31809, #37979, #22777, #19269, #777, #9789, #3624, #13084, #25640, #38171, #29119 ),
 .UNSPECIFIED., .F., .F.,
 ( 4, 2, 2, 2, 2, 2, 2, 2, 2, 4 ),
 ( 0.000000000000000000, 0.0006479730685966644116, 0.001295946137193328823, 0.002591892274386650707, 0.003239865342983302109, 0.003563851877281627809, 0.003887838411579953943, 0.004211824945878279644, 0.004535811480176605778, 0.005183784548773252843 ),
 .UNSPECIFIED. ) ;
#37506 = CIRCLE ( 'NONE', #25703, 0.01000000000000002970 ) ;
#37508 = CARTESIAN_POINT ( 'NONE',  ( 0.2413666260127980967, -0.9305387420463091530, 0.6820401963294040470 ) ) ;
#37509 = ORIENTED_EDGE ( 'NONE', *, *, #5436, .T. ) ;
#37510 = CARTESIAN_POINT ( 'NONE',  ( -0.03642997641688962979, 0.08373618209168329218, -0.5050295872266733488 ) ) ;
#37511 = CARTESIAN_POINT ( 'NONE',  ( -0.001101659507716951656, -0.9212496868719332044, 0.5732851652631911765 ) ) ;
#37513 = ORIENTED_EDGE ( 'NONE', *, *, #28045, .F. ) ;
#37512 = VERTEX_POINT ( 'NONE', #11759 ) ;
#37514 = CARTESIAN_POINT ( 'NONE',  ( -0.1669433606228600819, 0.5138636982738132852, 0.1528658435937002569 ) ) ;
#37515 = ORIENTED_EDGE ( 'NONE', *, *, #3407, .T. ) ;
#37516 = CARTESIAN_POINT ( 'NONE',  ( 0.1392976812637733430, -1.285713247446159890, 0.4252422542015512064 ) ) ;
#37517 = CARTESIAN_POINT ( 'NONE',  ( 0.1805592728925153601, -1.816701042908541508, -0.3505378111635870098 ) ) ;
#37518 = CARTESIAN_POINT ( 'NONE',  ( -0.2399999999999999079, -3.807157481699992907, -0.4735579732456337565 ) ) ;
#37520 = CARTESIAN_POINT ( 'NONE',  ( 0.4842604987045637799, -1.673939032089394097, 0.5259745941821198922 ) ) ;
#37519 = CARTESIAN_POINT ( 'NONE',  ( -0.2399999999999999079, -3.723902497147952406, 0.1004495357399106253 ) ) ;
#37521 = CARTESIAN_POINT ( 'NONE',  ( 0.03171861681798098659, -0.2437378752574246299, -0.4645579091361444757 ) ) ;
#37522 = EDGE_LOOP ( 'NONE', ( #15631, #17093, #7159, #39992 ) ) ;
#37523 = CONICAL_SURFACE ( 'NONE', #19802, 0.1946589359789743512, 1.047197551196599186 ) ;
#37524 = CARTESIAN_POINT ( 'NONE',  ( 0.09435491736042275757, -0.5840496667413408449, 0.2789874680385455163 ) ) ;
#37525 = ORIENTED_EDGE ( 'NONE', *, *, #3938, .F. ) ;
#37526 = CARTESIAN_POINT ( 'NONE',  ( 0.6902793494311211253, -1.541375760405424566, 0.6008920144000082786 ) ) ;
#37527 = CARTESIAN_POINT ( 'NONE',  ( 0.07437268989541760689, -0.5655675014591935446, 0.2541927867883168601 ) ) ;
#37528 = EDGE_CURVE ( 'NONE', #19589, #11583, #2095, .T. ) ;
#37530 = CARTESIAN_POINT ( 'NONE',  ( 0.5593818882502148426, -1.619251521524634363, 0.4799587450026789326 ) ) ;
#37529 = CARTESIAN_POINT ( 'NONE',  ( 0.3485603902089104977, -1.632100916239925148, -0.6568559003424170317 ) ) ;
#37531 = CARTESIAN_POINT ( 'NONE',  ( 0.4243666725459964151, -1.591076223527387423, -0.4156371400837810537 ) ) ;
#37532 = CARTESIAN_POINT ( 'NONE',  ( 0.1718750000000002776, -0.9178826446108662163, 0.1609973318550534105 ) ) ;
#37533 = APPLIED_DATE_AND_TIME_ASSIGNMENT ( #12374, #30490, ( #6386 ) ) ;
#37534 = EDGE_LOOP ( 'NONE', ( #4019, #27434, #18680, #26135 ) ) ;
#37535 = CARTESIAN_POINT ( 'NONE',  ( 0.1169788285577439829, -1.415237608940837388, 0.5049415650359101448 ) ) ;
#37536 = CARTESIAN_POINT ( 'NONE',  ( 0.1887412855916273668, -0.4595320686313604241, 0.1365881794216594058 ) ) ;
#37537 = CARTESIAN_POINT ( 'NONE',  ( 0.5809272469664140681, -1.495261656052034871, 0.5735391159125613481 ) ) ;
#37538 = CARTESIAN_POINT ( 'NONE',  ( 0.4259795917038463609, -1.695922107943511836, 0.4200542363796885836 ) ) ;
#37539 = CARTESIAN_POINT ( 'NONE',  ( -0.03672309138970014653, 0.3146134659443282633, -0.3636027875696382083 ) ) ;
#37540 = AXIS2_PLACEMENT_3D ( 'NONE', #26078, #38597, #33029 ) ;
#37541 = CIRCLE ( 'NONE', #19815, 0.1500000000000011324 ) ;
#37542 = DIRECTION ( 'NONE',  ( 1.000000000000000000, 0.000000000000000000, 0.000000000000000000 ) ) ;
#37543 = CARTESIAN_POINT ( 'NONE',  ( 0.2257694031136883717, -1.236620430762222167, 0.5267521799253104264 ) ) ;
#37544 = VECTOR ( 'NONE', #23074, 39.37007874015748143 ) ;
#37545 = CARTESIAN_POINT ( 'NONE',  ( 0.1499999999999993561, 0.000000000000000000, 0.000000000000000000 ) ) ;
#37546 = CARTESIAN_POINT ( 'NONE',  ( 0.2321516500765777036, -1.232946919155727183, 0.5425383027153066751 ) ) ;
#37547 = CARTESIAN_POINT ( 'NONE',  ( 0.5091714098097919194, -1.126742604313814677, 0.8493738626068785269 ) ) ;
#37548 = CARTESIAN_POINT ( 'NONE',  ( -0.01896968469603047686, 0.3622774521524885771, 0.3730768833943122753 ) ) ;
#37549 = CARTESIAN_POINT ( 'NONE',  ( 0.06547945893112464000, -1.297457944248764594, 0.6222148637417063144 ) ) ;
#37550 = CARTESIAN_POINT ( 'NONE',  ( 0.6480134723046564460, -1.557673986349219941, -0.4212882653819030598 ) ) ;
#37551 = DIRECTION ( 'NONE',  ( -0.8660512985181133550, -0.4999551463232372872, 0.000000000000000000 ) ) ;
#37552 = CARTESIAN_POINT ( 'NONE',  ( 0.1737315473343117589, -0.8901614270947242336, 0.5692762810378355631 ) ) ;
#37553 = CARTESIAN_POINT ( 'NONE',  ( 0.2660108306589821781, -1.675569572048062561, 0.5682491886492555544 ) ) ;
#37554 = CARTESIAN_POINT ( 'NONE',  ( -0.02000000000000000042, -1.910390638264138685, -0.8820407338378629669 ) ) ;
#37555 = EDGE_CURVE ( 'NONE', #18554, #7023, #33165, .T. ) ;
#37556 = VERTEX_POINT ( 'NONE', #18138 ) ;
#37557 = DIRECTION ( 'NONE',  ( 0.000000000000000000, -3.885780586188049371E-16, -1.000000000000000000 ) ) ;
#37558 = CARTESIAN_POINT ( 'NONE',  ( 0.4282286496180897628, -1.188361668518445713, 0.7944891104112847824 ) ) ;
#37559 = ADVANCED_FACE ( 'NONE', ( #17717 ), #35080, .F. ) ;
#37560 = CARTESIAN_POINT ( 'NONE',  ( 0.6665678333534084121, -1.510259890604198407, 0.4229811308471109754 ) ) ;
#37561 = AXIS2_PLACEMENT_3D ( 'NONE', #12116, #15799, #12712 ) ;
#37562 = CARTESIAN_POINT ( 'NONE',  ( 0.4100456123093286775, -1.725225710419908243, -0.4268450903248972028 ) ) ;
#37563 = CARTESIAN_POINT ( 'NONE',  ( 0.3982365725197472561, -1.726079210701410460, 0.6107553134230500058 ) ) ;
#37564 = EDGE_CURVE ( 'NONE', #5039, #17175, #12166, .T. ) ;
#37565 = ORIENTED_EDGE ( 'NONE', *, *, #17691, .F. ) ;
#37566 = CARTESIAN_POINT ( 'NONE',  ( 0.5488242727466704496, -1.662431386828975288, -0.5397256741273313008 ) ) ;
#37567 = AXIS2_PLACEMENT_3D ( 'NONE', #24761, #15683, #18571 ) ;
#37568 = AXIS2_PLACEMENT_3D ( 'NONE', #29008, #35793, #35994 ) ;
#37569 = FACE_BOUND ( 'NONE', #39603, .T. ) ;
#37570 = CARTESIAN_POINT ( 'NONE',  ( -0.07216878364870250862, 0.000000000000000000, 0.1249999999999993477 ) ) ;
#37571 = CARTESIAN_POINT ( 'NONE',  ( 0.05078310099560659485, 0.3164655623698883202, -0.3525377550954976180 ) ) ;
#37572 = CIRCLE ( 'NONE', #19853, 0.1620173459747806799 ) ;
#37573 = CARTESIAN_POINT ( 'NONE',  ( 0.4540194299641387987, -1.222353591583736687, 0.7124676942563946680 ) ) ;
#37575 = DIRECTION ( 'NONE',  ( -1.000000000000000000, -0.000000000000000000, -0.000000000000000000 ) ) ;
#37574 = DIRECTION ( 'NONE',  ( 0.4999551463232372317, -0.8660512985181134660, 0.000000000000000000 ) ) ;
#37576 = CARTESIAN_POINT ( 'NONE',  ( 0.1863616350354748430, -0.8703638341540448353, 0.1952903930469164218 ) ) ;
#37577 = ORIENTED_EDGE ( 'NONE', *, *, #510, .T. ) ;
#37578 = DATE_AND_TIME ( #31012, #18119 ) ;
#37579 = PLANE ( 'NONE',  #21758 ) ;
#37580 = ORIENTED_EDGE ( 'NONE', *, *, #27106, .F. ) ;
#37581 = ORIENTED_EDGE ( 'NONE', *, *, #22686, .F. ) ;
#37582 = CARTESIAN_POINT ( 'NONE',  ( 0.3849909235177108591, -1.605527633581090852, 0.5705237664168376632 ) ) ;
#37583 = ADVANCED_FACE ( 'NONE', ( #21229 ), #8657, .F. ) ;
#37585 = CARTESIAN_POINT ( 'NONE',  ( 0.1748516657612844138, -0.8884282797386773289, 0.03374897621379178286 ) ) ;
#37584 = LINE ( 'NONE', #9406, #18432 ) ;
#37586 = DIRECTION ( 'NONE',  ( 5.551115123125783935E-17, 0.000000000000000000, -1.000000000000000000 ) ) ;
#37587 = APPLIED_DATE_AND_TIME_ASSIGNMENT ( #30645, #2657, ( #25296 ) ) ;
#37588 = EDGE_LOOP ( 'NONE', ( #36203, #17346, #39809, #17137 ) ) ;
#37589 = ORIENTED_EDGE ( 'NONE', *, *, #36823, .F. ) ;
#37590 = ORIENTED_EDGE ( 'NONE', *, *, #26993, .F. ) ;
#37591 = ORIENTED_EDGE ( 'NONE', *, *, #36503, .T. ) ;
#37592 = CARTESIAN_POINT ( 'NONE',  ( 0.4347216870940026623, -1.031328747192698625, 0.7169922827082580996 ) ) ;
#37593 = CARTESIAN_POINT ( 'NONE',  ( 0.1528991923064401126, -0.7010905126288613509, 0.5001151810244065521 ) ) ;
#37594 = ORIENTED_EDGE ( 'NONE', *, *, #13500, .T. ) ;
#37595 = CARTESIAN_POINT ( 'NONE',  ( 0.1871790664487952560, -0.7087350574275718129, 0.03072952741108740324 ) ) ;
#37596 = PLANE ( 'NONE',  #16073 ) ;
#37597 = CARTESIAN_POINT ( 'NONE',  ( 0.6107611075265444445, -1.468610687554505745, -0.6249999999999998890 ) ) ;
#37598 = CARTESIAN_POINT ( 'NONE',  ( 0.003621456447956619175, -1.840971628676655980, -0.3528920961991032224 ) ) ;
#37599 = CARTESIAN_POINT ( 'NONE',  ( -0.1157923916715207918, -0.5295015842444125154, 0.3181161673586298533 ) ) ;
#37600 = CARTESIAN_POINT ( 'NONE',  ( -0.02418142828330810401, 0.06026811487149385388, 0.1249999999999993616 ) ) ;
#37601 = CIRCLE ( 'NONE', #11971, 0.06250000000000001388 ) ;
#37602 = CARTESIAN_POINT ( 'NONE',  ( -0.1157923916715206114, -0.5295015842444287246, 0.1000000000000000194 ) ) ;
#37603 = CIRCLE ( 'NONE', #36278, 0.06000000000000045575 ) ;
#37604 = CARTESIAN_POINT ( 'NONE',  ( 0.02953079040095700838, 0.3810518745593862167, -0.3687679460475775106 ) ) ;
#37605 = CARTESIAN_POINT ( 'NONE',  ( 0.1589950187058418174, -2.053370087202771810, -0.6806478816540684207 ) ) ;
#37606 = FACE_OUTER_BOUND ( 'NONE', #31563, .T. ) ;
#37607 = PERSON_AND_ORGANIZATION ( #28500, #32463 ) ;
#37608 = CIRCLE ( 'NONE', #867, 0.08000000000000000167 ) ;
#37609 = CARTESIAN_POINT ( 'NONE',  ( 0.4878597496520711285, -1.079924603896147195, 0.5970707234729024648 ) ) ;
#37610 = CARTESIAN_POINT ( 'NONE',  ( 0.3121297305841956859, -1.175746190035780403, 0.5106052970165252392 ) ) ;
#37611 = CARTESIAN_POINT ( 'NONE',  ( 0.5623208420996907986, -1.181176875011435756, 0.6057417262809816627 ) ) ;
#37612 = B_SPLINE_CURVE_WITH_KNOTS ( 'NONE', 3,
 ( #17705, #2081, #33533, #14619, #2300, #27189 ),
 .UNSPECIFIED., .F., .F.,
 ( 4, 2, 4 ),
 ( 0.000000000000000000, 0.0005939623046373305147, 0.001187924609274661029 ),
 .UNSPECIFIED. ) ;
#37613 = DIRECTION ( 'NONE',  ( 0.000000000000000000, -0.6595282642760672553, -0.7516797646744243222 ) ) ;
#37614 = EDGE_CURVE ( 'NONE', #4836, #18572, #20724, .T. ) ;
#37615 = AXIS2_PLACEMENT_3D ( 'NONE', #36947, #5680, #2598 ) ;
#37616 = CARTESIAN_POINT ( 'NONE',  ( 0.1120276941441372132, -1.367097346105948130, 0.7195291715619951400 ) ) ;
#37617 = LINE ( 'NONE', #40087, #39638 ) ;
#37618 = ADVANCED_FACE ( 'NONE', ( #31306 ), #3517, .T. ) ;
#37619 = CARTESIAN_POINT ( 'NONE',  ( 0.6747199749832551996, -1.439515243308204795, 0.4672089648579093590 ) ) ;
#37620 = CARTESIAN_POINT ( 'NONE',  ( 0.3242889740156271738, -1.641829081526549716, 0.4952036213288416588 ) ) ;
#37621 = ADVANCED_FACE ( 'NONE', ( #12778 ), #22059, .F. ) ;
#37622 = VERTEX_POINT ( 'NONE', #22063 ) ;
#37623 = VERTEX_POINT ( 'NONE', #5975 ) ;
#37624 = CARTESIAN_POINT ( 'NONE',  ( -0.2746410161513776482, -3.758594918004649621, -0.06617323996463192470 ) ) ;
#37625 = ORIENTED_EDGE ( 'NONE', *, *, #28513, .T. ) ;
#37626 = CARTESIAN_POINT ( 'NONE',  ( -2.567390744445674500E-16, -0.02999999999999982889, -0.1849999999999994982 ) ) ;
#37627 = CARTESIAN_POINT ( 'NONE',  ( 0.03664605387828134830, 0.2484618661253114036, 0.4118464167359231487 ) ) ;
#37628 = CIRCLE ( 'NONE', #15316, 0.009999999999999981126 ) ;
#37629 = CARTESIAN_POINT ( 'NONE',  ( 0.5749443205740174534, -1.420905134751040855, 0.6314223347319325441 ) ) ;
#37631 = ORIENTED_EDGE ( 'NONE', *, *, #36877, .F. ) ;
#37630 = FACE_OUTER_BOUND ( 'NONE', #29553, .T. ) ;
#37632 = B_SPLINE_CURVE_WITH_KNOTS ( 'NONE', 3,
 ( #34086, #39863, #34499, #9003 ),
 .UNSPECIFIED., .F., .F.,
 ( 4, 4 ),
 ( 0.000000000000000000, 0.001593837860110619521 ),
 .UNSPECIFIED. ) ;
#37633 = ORIENTED_EDGE ( 'NONE', *, *, #6627, .F. ) ;
#37634 = DIRECTION ( 'NONE',  ( -0.2067069058495556444, -0.1193280138680804653, -0.9710989033977962537 ) ) ;
#37635 = ORIENTED_EDGE ( 'NONE', *, *, #4666, .T. ) ;
#37636 = AXIS2_PLACEMENT_3D ( 'NONE', #27919, #15968, #28515 ) ;
#37637 = EDGE_CURVE ( 'NONE', #24607, #356, #34371, .T. ) ;
#37638 = CARTESIAN_POINT ( 'NONE',  ( 0.01343172348619905282, -0.5732673182617886720, 0.3074519330991232757 ) ) ;
#37639 = EDGE_CURVE ( 'NONE', #34948, #33422, #27806, .T. ) ;
#37641 = CARTESIAN_POINT ( 'NONE',  ( 0.1049266666186983721, -1.284188116108003097, 0.6131522485820786184 ) ) ;
#37640 = CARTESIAN_POINT ( 'NONE',  ( 0.5153600767897008605, -1.667753545667869153, -0.4356355497465531634 ) ) ;
#37642 = B_SPLINE_CURVE_WITH_KNOTS ( 'NONE', 3,
 ( #18517, #21433, #9062, #36819 ),
 .UNSPECIFIED., .F., .F.,
 ( 4, 4 ),
 ( -0.0003965198687675489109, 0.0004429401854243748132 ),
 .UNSPECIFIED. ) ;
#37643 = CARTESIAN_POINT ( 'NONE',  ( 0.01205285774706865709, -0.4630597876925141021, 0.01601191316080295690 ) ) ;
#37644 = ADVANCED_FACE ( 'NONE', ( #40342 ), #37878, .F. ) ;
#37645 = TOROIDAL_SURFACE ( 'NONE', #13897, 0.04999999999999998196, 0.2000000000000000111 ) ;
#37646 = DIRECTION ( 'NONE',  ( -7.000205099780314469E-17, -1.000000000000000000, 6.590151126658399604E-16 ) ) ;
#37648 = ORIENTED_EDGE ( 'NONE', *, *, #2962, .F. ) ;
#37647 = EDGE_LOOP ( 'NONE', ( #89, #22467, #1286, #35514 ) ) ;
#37649 = EDGE_CURVE ( 'NONE', #15269, #19872, #14151, .T. ) ;
#37650 = CARTESIAN_POINT ( 'NONE',  ( 0.4761091661982407297, -1.093057945753640459, -0.4172484957075230927 ) ) ;
#37651 = DIRECTION ( 'NONE',  ( 0.000000000000000000, 0.000000000000000000, -1.000000000000000000 ) ) ;
#37652 = CIRCLE ( 'NONE', #19915, 0.01500000000000004628 ) ;
#37653 = CARTESIAN_POINT ( 'NONE',  ( -0.01899468245561876031, -0.5123206680798518819, 0.08888613072388566738 ) ) ;
#37654 = CARTESIAN_POINT ( 'NONE',  ( 0.5515293582047056109, -1.419488402371683833, 0.7635374488037771634 ) ) ;
#37655 = ADVANCED_FACE ( 'NONE', ( #15657 ), #7569, .T. ) ;
#37656 = CARTESIAN_POINT ( 'NONE',  ( -2.112273405726188513E-14, -2.183180860297921466, -0.4937760292030871079 ) ) ;
#37657 = CARTESIAN_POINT ( 'NONE',  ( 0.4974659133798483013, -1.692079602952080819, -0.4360564763722065140 ) ) ;
#37658 = CARTESIAN_POINT ( 'NONE',  ( 0.2177940209044571529, -1.312915603899528438, 1.030959333779153164 ) ) ;
#37659 = APPLICATION_CONTEXT ( 'configuration controlled 3d designs of mechanical parts and assemblies' ) ;
#37660 = DIRECTION ( 'NONE',  ( 0.000000000000000000, 0.000000000000000000, -1.000000000000000000 ) ) ;
#37661 = DIRECTION ( 'NONE',  ( -7.000205099780314469E-17, -1.000000000000000000, 6.590151126658399604E-16 ) ) ;
#37662 = DIRECTION ( 'NONE',  ( 0.000000000000000000, 0.5781348229923761739, -0.8159412518334723252 ) ) ;
#37663 = CARTESIAN_POINT ( 'NONE',  ( -0.3000000000000000999, -4.320736256378554963, -0.8145269479932405465 ) ) ;
#37664 = AXIS2_PLACEMENT_3D ( 'NONE', #14294, #23385, #13868 ) ;
#37665 = DIRECTION ( 'NONE',  ( -1.000000000000000000, -7.857794173099924470E-32, -8.628166150854818811E-32 ) ) ;
#37666 = CARTESIAN_POINT ( 'NONE',  ( 0.2646723247128293655, -1.687375416948911244, 0.5682417262808783232 ) ) ;
#37667 = CARTESIAN_POINT ( 'NONE',  ( 0.05311564377218584709, -1.038294028734484620, 0.7210077450460690152 ) ) ;
#37668 = CALENDAR_DATE ( 2026, 13, 10 ) ;
#37669 = AXIS2_PLACEMENT_3D ( 'NONE', #19526, #18920, #38029 ) ;
#37670 = AXIS2_PLACEMENT_3D ( 'NONE', #831, #38824, #16632 ) ;
#37671 = EDGE_CURVE ( 'NONE', #33435, #27442, #18757, .T. ) ;
#37672 = CARTESIAN_POINT ( 'NONE',  ( 0.3338244128917602915, -1.760037155675280518, 0.5632158866801645347 ) ) ;
#37673 = CARTESIAN_POINT ( 'NONE',  ( 0.6926962928713769063, -1.550933885067852902, 0.5932296416423278318 ) ) ;
#37674 = EDGE_CURVE ( 'NONE', #38708, #591, #8896, .T. ) ;
#37675 = CARTESIAN_POINT ( 'NONE',  ( -2.915087563824520450E-32, 7.160938508832261116E-17, 0.2149999999999999967 ) ) ;
#37676 = AXIS2_PLACEMENT_3D ( 'NONE', #14481, #8108, #17592 ) ;
#37677 = TOROIDAL_SURFACE ( 'NONE', #9427, 0.1333070866141734256, 0.02999999999999999889 ) ;
#37678 = CARTESIAN_POINT ( 'NONE',  ( 0.3408697296860659920, -1.678829344471958862, -0.4023362845575238489 ) ) ;
#37679 = EDGE_LOOP ( 'NONE', ( #316, #10458, #33325, #24105, #13873 ) ) ;
#37680 = CARTESIAN_POINT ( 'NONE',  ( 0.4475189022780061698, -1.144336077227306347, -0.3898466471268308697 ) ) ;
#37681 = CARTESIAN_POINT ( 'NONE',  ( 0.2673801512343003117, -1.641609933369855501, 0.7978219346028294634 ) ) ;
#37682 = CARTESIAN_POINT ( 'NONE',  ( 0.1316567728380550195, -0.5516482450355230105, 0.1613228570193817046 ) ) ;
#37684 = ORIENTED_EDGE ( 'NONE', *, *, #28854, .T. ) ;
#37683 = DIRECTION ( 'NONE',  ( 0.9998941247116546194, -0.01455087607600989881, 0.0001066420868425327849 ) ) ;
#37685 = CARTESIAN_POINT ( 'NONE',  ( 0.2322244407957205770, -0.7584751632699872070, 0.4677412183550399005 ) ) ;
#37687 = ORIENTED_EDGE ( 'NONE', *, *, #1714, .T. ) ;
#37686 = ORIENTED_EDGE ( 'NONE', *, *, #4989, .T. ) ;
#37688 = CARTESIAN_POINT ( 'NONE',  ( 0.6104464726719969203, -1.287892560030390099, 0.8054571804883312591 ) ) ;
#37689 = DIRECTION ( 'NONE',  ( 0.000000000000000000, 0.000000000000000000, -1.000000000000000000 ) ) ;
#37690 = CYLINDRICAL_SURFACE ( 'NONE', #27899, 0.1000000000000000194 ) ;
#37691 = DATE_AND_TIME ( #25153, #39845 ) ;
#37692 = FACE_OUTER_BOUND ( 'NONE', #11120, .T. ) ;
#37693 = ORIENTED_EDGE ( 'NONE', *, *, #19187, .T. ) ;
#37694 = EDGE_CURVE ( 'NONE', #1152, #23493, #25125, .T. ) ;
#37695 = CARTESIAN_POINT ( 'NONE',  ( 0.08617281636341815598, -0.7679981000224859189, 0.1929316491008059298 ) ) ;
#37696 = CARTESIAN_POINT ( 'NONE',  ( 0.3138383792994305921, -1.724913923476310895, 0.8094178256982638153 ) ) ;
#37697 = CIRCLE ( 'NONE', #21951, 0.1000000000000008521 ) ;
#37698 = CARTESIAN_POINT ( 'NONE',  ( 0.5246584051016858208, -1.526692330542510856, 0.5635048083496201343 ) ) ;
#37699 = CARTESIAN_POINT ( 'NONE',  ( 0.5988768534318814618, -1.579658039218154286, -0.6073675125623819726 ) ) ;
#37700 = CARTESIAN_POINT ( 'NONE',  ( -0.1621871387067669035, 0.5037941088976310988, 0.1094562450723023384 ) ) ;
#37701 = EDGE_LOOP ( 'NONE', ( #36961, #18324, #38463, #28042 ) ) ;
#37702 = CARTESIAN_POINT ( 'NONE',  ( 0.4347228130698158610, -1.693624708453924876, 0.6021643700774704788 ) ) ;
#37703 = CARTESIAN_POINT ( 'NONE',  ( 0.6993589672832161153, -1.438438989639379439, 0.5922646702261220586 ) ) ;
#37704 = AXIS2_PLACEMENT_3D ( 'NONE', #30774, #31574, #6474 ) ;
#37705 = CARTESIAN_POINT ( 'NONE',  ( 0.5766624839413022618, -1.620837096128123989, 0.5630430456491227753 ) ) ;
#37706 = CARTESIAN_POINT ( 'NONE',  ( 0.6090910762621168928, -1.479036187308539807, 0.5740727581542524049 ) ) ;
#37707 = AXIS2_PLACEMENT_3D ( 'NONE', #6626, #13033, #38112 ) ;
#37708 = CARTESIAN_POINT ( 'NONE',  ( 0.03309057659885075720, -0.5154121718708735145, 0.07470590733143715745 ) ) ;
#37709 = CARTESIAN_POINT ( 'NONE',  ( 0.4092450614235220163, -1.131740385117829817, 0.4687417262808780127 ) ) ;
#37710 = FACE_OUTER_BOUND ( 'NONE', #6597, .T. ) ;
#37711 = CARTESIAN_POINT ( 'NONE',  ( -0.2399999999999999079, -4.120026397279962005, -0.6279592245183788224 ) ) ;
#37712 = CARTESIAN_POINT ( 'NONE',  ( 0.5127940875192875669, -1.116701596374397587, 0.5863938561526392812 ) ) ;
#37713 = CALENDAR_DATE ( 2026, 13, 10 ) ;
#37714 =( BOUNDED_SURFACE ( )  B_SPLINE_SURFACE ( 3, 2, ( 
 ( #22208, #37402, #19105 ),
 ( #37213, #30831, #12512 ),
 ( #11900, #15613, #21786 ),
 ( #27551, #2651, #28159 ) ),
 .UNSPECIFIED., .F., .F., .F. ) 
 B_SPLINE_SURFACE_WITH_KNOTS ( ( 4, 4 ),
 ( 3, 3 ),
 ( 1.314703554355922677E-15, 0.0007336933749180589437 ),
 ( 0.000000000000000000, 1.000000000000000000 ),
 .UNSPECIFIED. ) 
 GEOMETRIC_REPRESENTATION_ITEM ( )  RATIONAL_B_SPLINE_SURFACE ( (
 ( 1.000000000000000000, 0.8624897507812552266, 1.000000000000000000),
 ( 1.000000000000000000, 0.8280948711062059431, 1.000000000000000000),
 ( 1.000000000000000000, 0.7730114043998153051, 1.000000000000000000),
 ( 1.000000000000000000, 0.7004196158429182306, 1.000000000000000000) ) ) 
 REPRESENTATION_ITEM ( '' )  SURFACE ( )  );
#37715 = DIRECTION ( 'NONE',  ( 0.000000000000000000, 0.000000000000000000, -1.000000000000000000 ) ) ;
#37716 = VECTOR ( 'NONE', #7066, 39.37007874015748143 ) ;
#37717 = EDGE_CURVE ( 'NONE', #28606, #12681, #28618, .T. ) ;
#37718 = ORIENTED_EDGE ( 'NONE', *, *, #22567, .T. ) ;
#37719 = EDGE_CURVE ( 'NONE', #24860, #37622, #8251, .T. ) ;
#37720 = CARTESIAN_POINT ( 'NONE',  ( 0.4667682742968850551, -1.559724797038235300, 0.5741068050677242685 ) ) ;
#37721 = CARTESIAN_POINT ( 'NONE',  ( -0.04760454375020965745, -0.04300716520882088417, 0.4803168140823217969 ) ) ;
#37722 = AXIS2_PLACEMENT_3D ( 'NONE', #35864, #32967, #33182 ) ;
#37723 = AXIS2_PLACEMENT_3D ( 'NONE', #38186, #25655, #4026 ) ;
#37724 = ORIENTED_EDGE ( 'NONE', *, *, #35417, .F. ) ;
#37725 = CARTESIAN_POINT ( 'NONE',  ( 0.4863315821689714880, -1.129918813781339404, 0.4934822903636956193 ) ) ;
#37726 =( GEOMETRIC_REPRESENTATION_CONTEXT ( 3 ) GLOBAL_UNCERTAINTY_ASSIGNED_CONTEXT ( ( #3007 ) ) GLOBAL_UNIT_ASSIGNED_CONTEXT ( ( #7004, #28015, #28411 ) ) REPRESENTATION_CONTEXT ( 'NONE', 'WORKASPACE' ) );
#37727 = CARTESIAN_POINT ( 'NONE',  ( 0.07318992162220727682, -1.313491455601902613, 0.4675735672926750741 ) ) ;
#37728 = LINE ( 'NONE', #733, #33112 ) ;
#37729 = EDGE_LOOP ( 'NONE', ( #1291, #7420, #5699 ) ) ;
#37730 = CARTESIAN_POINT ( 'NONE',  ( 0.1434010736994648927, -1.283284918233685623, 0.5707417262808780478 ) ) ;
#37731 = AXIS2_PLACEMENT_3D ( 'NONE', #4359, #29050, #29464 ) ;
#37732 = CARTESIAN_POINT ( 'NONE',  ( 0.09645609262235674275, -1.159589713166229608, 0.7612075701997731425 ) ) ;
#37734 = VERTEX_POINT ( 'NONE', #18536 ) ;
#37733 = ORIENTED_EDGE ( 'NONE', *, *, #36152, .F. ) ;
#37735 = DIRECTION ( 'NONE',  ( 0.000000000000000000, 0.000000000000000000, -1.000000000000000000 ) ) ;
#37736 = CIRCLE ( 'NONE', #15400, 0.6114999999999938263 ) ;
#37737 = CARTESIAN_POINT ( 'NONE',  ( 0.1185427538159745248, -1.297446678095303563, 0.4322093719855905625 ) ) ;
#37738 = CARTESIAN_POINT ( 'NONE',  ( 0.3682921722882570026, -2.034650425189704848, -0.3093546411653611550 ) ) ;
#37740 = CARTESIAN_POINT ( 'NONE',  ( -0.02000000000000000042, -2.183180860297908144, -0.4937760292030871079 ) ) ;
#37739 = DIRECTION ( 'NONE',  ( 1.702140497302368679E-12, -0.9510565162951529761, 0.3090169943749491166 ) ) ;
#37741 = CARTESIAN_POINT ( 'NONE',  ( 0.03674078017396031209, -0.2486088097086599225, -0.4115158447297234123 ) ) ;
#37742 = ORIENTED_EDGE ( 'NONE', *, *, #28868, .T. ) ;
#37743 = CARTESIAN_POINT ( 'NONE',  ( -0.04154009738085503306, 0.2902754972779528764, -0.3700679770908116284 ) ) ;
#37744 = CARTESIAN_POINT ( 'NONE',  ( 0.09349442991740078424, -0.6180904650601271033, 0.2586776949927410141 ) ) ;
#37745 = ORIENTED_EDGE ( 'NONE', *, *, #36145, .F. ) ;
#37746 = ORIENTED_EDGE ( 'NONE', *, *, #21732, .T. ) ;
#37747 = CARTESIAN_POINT ( 'NONE',  ( 0.05561170715395061942, 0.02038383341412389541, 0.4604752114371306604 ) ) ;
#37748 = CARTESIAN_POINT ( 'NONE',  ( 0.07513757318104685723, -0.5719538737171597775, 0.2718397121403446914 ) ) ;
#37750 = PLANE ( 'NONE',  #17622 ) ;
#37749 = CARTESIAN_POINT ( 'NONE',  ( 0.5324218574196054599, -1.599714249701870372, -0.4411601419016027981 ) ) ;
#37751 = DIRECTION ( 'NONE',  ( 1.000000000000000000, 2.276539994720212446E-15, -1.138269997360106223E-15 ) ) ;
#37752 = CARTESIAN_POINT ( 'NONE',  ( 0.1932155651835060495, -0.9182634696541240871, 0.2611848007271776462 ) ) ;
#37753 = AXIS2_PLACEMENT_3D ( 'NONE', #5391, #24159, #21474 ) ;
#37754 = EDGE_CURVE ( 'NONE', #39055, #34829, #18778, .T. ) ;
#37755 = PLANE ( 'NONE',  #29841 ) ;
#37756 = CARTESIAN_POINT ( 'NONE',  ( 0.3917177981610598936, -1.718486023052998135, -0.3060476212702296084 ) ) ;
#37757 = AXIS2_PLACEMENT_3D ( 'NONE', #25062, #31247, #33488 ) ;
#37758 = CARTESIAN_POINT ( 'NONE',  ( 0.1256422341217116601, -0.5670699205730641568, 0.2299123196654525580 ) ) ;
#37759 = CARTESIAN_POINT ( 'NONE',  ( -0.05268850283020189845, 0.2791746226943783160, -0.3764045485075417363 ) ) ;
#37760 = CIRCLE ( 'NONE', #8177, 0.07999999999999996003 ) ;
#37761 = AXIS2_PLACEMENT_3D ( 'NONE', #15724, #22327, #9560 ) ;
#37762 = LOCAL_TIME ( 0, 53, 7.000000000000000000, #20891 ) ;
#37763 = DIRECTION ( 'NONE',  ( 1.000000000000000000, -0.000000000000000000, -0.000000000000000000 ) ) ;
#37764 = DIRECTION ( 'NONE',  ( 0.000000000000000000, 0.000000000000000000, -1.000000000000000000 ) ) ;
#37765 = CIRCLE ( 'NONE', #23987, 0.06250000000000000000 ) ;
#37766 = CARTESIAN_POINT ( 'NONE',  ( 0.3938123320717736853, -0.9371650893754340794, 0.7866333354397343491 ) ) ;
#37767 = CARTESIAN_POINT ( 'NONE',  ( -0.05268850283020295316, 0.2717122958104549735, 0.3818262463465875722 ) ) ;
#37768 = CARTESIAN_POINT ( 'NONE',  ( 0.03667004059205163091, -1.157784549275130859, 0.6760954598802072502 ) ) ;
#37769 = CARTESIAN_POINT ( 'NONE',  ( 0.6399061864322146409, -1.581153798985416747, -0.4326948249935556046 ) ) ;
#37770 = LINE ( 'NONE', #389, #6800 ) ;
#37771 = CARTESIAN_POINT ( 'NONE',  ( 0.1047100132654907034, -0.8222625085212694751, 0.3700008871823666778 ) ) ;
#37772 = DIRECTION ( 'NONE',  ( -3.406373435249024214E-19, -1.000000000000000000, -7.170354002788761615E-17 ) ) ;
#37773 = DIRECTION ( 'NONE',  ( 0.000000000000000000, 1.000000000000000000, 1.566396143878659165E-12 ) ) ;
#37774 = ORIENTED_EDGE ( 'NONE', *, *, #34613, .T. ) ;
#37775 = DIRECTION ( 'NONE',  ( -2.563099466555626504E-12, -0.5877852522924708056, 0.8090169943749491166 ) ) ;
#37776 = CARTESIAN_POINT ( 'NONE',  ( 0.3683998553492333072, -1.620410879730887599, -0.3666241388582308636 ) ) ;
#37777 = AXIS2_PLACEMENT_3D ( 'NONE', #11132, #17100, #29859 ) ;
#37778 = FACE_OUTER_BOUND ( 'NONE', #22388, .T. ) ;
#37779 = CARTESIAN_POINT ( 'NONE',  ( 0.5223466852174000197, -1.671872836107813232, -0.4402217964095243574 ) ) ;
#37780 = CARTESIAN_POINT ( 'NONE',  ( -0.04293694706340306366, -0.07181688488226570244, 0.4893579783149998308 ) ) ;
#37781 = VECTOR ( 'NONE', #13858, 39.37007874015748143 ) ;
#37782 = CIRCLE ( 'NONE', #29247, 0.5302738246768099462 ) ;
#37783 = EDGE_LOOP ( 'NONE', ( #9252, #27889, #29699, #22392 ) ) ;
#37784 = CARTESIAN_POINT ( 'NONE',  ( 0.4942245234460003744, -1.693950796473111975, -0.6125153944540959738 ) ) ;
#37785 = CARTESIAN_POINT ( 'NONE',  ( 0.2592691511196472121, -1.332774616786658761, 0.4676817362816936274 ) ) ;
#37786 = LOCAL_TIME ( 0, 53, 7.000000000000000000, #4376 ) ;
#37787 = DIRECTION ( 'NONE',  ( 1.000000000000000000, 0.000000000000000000, 0.000000000000000000 ) ) ;
#37788 = CARTESIAN_POINT ( 'NONE',  ( 0.05279905671745029061, 0.3065870127358052422, -0.3541429396892920578 ) ) ;
#37789 = CARTESIAN_POINT ( 'NONE',  ( 0.3484262649563198422, -1.078417651898806895, 0.7434214752059845610 ) ) ;
#37791 = CYLINDRICAL_SURFACE ( 'NONE', #20124, 0.03000000000000008910 ) ;
#37790 = CARTESIAN_POINT ( 'NONE',  ( 0.000000000000000000, -0.01499999999999997689, 0.000000000000000000 ) ) ;
#37792 = B_SPLINE_CURVE_WITH_KNOTS ( 'NONE', 3,
 ( #40201, #37131, #21308, #34650 ),
 .UNSPECIFIED., .F., .F.,
 ( 4, 4 ),
 ( 0.000000000000000000, 0.0002765727889952716173 ),
 .UNSPECIFIED. ) ;
#37793 = CARTESIAN_POINT ( 'NONE',  ( 0.4613690144166702201, -1.065390048215762997, 0.6270275320092995042 ) ) ;
#37794 = VERTEX_POINT ( 'NONE', #24925 ) ;
#37795 = COORDINATED_UNIVERSAL_TIME_OFFSET ( 0, 0, .AHEAD. ) ;
#37796 = AXIS2_PLACEMENT_3D ( 'NONE', #3910, #23267, #39086 ) ;
#37797 = LINE ( 'NONE', #28930, #28321 ) ;
#37798 = ORIENTED_EDGE ( 'NONE', *, *, #39859, .T. ) ;
#37799 = ORIENTED_EDGE ( 'NONE', *, *, #879, .T. ) ;
#37800 = CARTESIAN_POINT ( 'NONE',  ( 0.08048400592800619702, -0.7604391007274543535, 0.6087342011644325535 ) ) ;
#37802 = CARTESIAN_POINT ( 'NONE',  ( 0.1756540496027305942, -0.7486115422362458194, -0.07645544523215128119 ) ) ;
#37801 = CARTESIAN_POINT ( 'NONE',  ( 0.06534793968408428300, -0.7997581921860751342, 0.04923965712713711251 ) ) ;
#37803 = CARTESIAN_POINT ( 'NONE',  ( 0.1994181777622906770, -2.041053584879497063, -0.3082502591624063371 ) ) ;
#37804 = B_SPLINE_CURVE_WITH_KNOTS ( 'NONE', 3,
 ( #31444, #28348, #217, #36785 ),
 .UNSPECIFIED., .F., .F.,
 ( 4, 4 ),
 ( 0.000000000000000000, 0.0005209419993945884871 ),
 .UNSPECIFIED. ) ;
#37805 = ORIENTED_EDGE ( 'NONE', *, *, #18046, .F. ) ;
#37806 = ORIENTED_EDGE ( 'NONE', *, *, #4116, .T. ) ;
#37807 = ORIENTED_EDGE ( 'NONE', *, *, #33893, .T. ) ;
#37808 = DIRECTION ( 'NONE',  ( 0.4999551463232372317, -0.8660512985181135770, 0.000000000000000000 ) ) ;
#37809 = CARTESIAN_POINT ( 'NONE',  ( 0.5678201344545344975, -1.503056767399954863, 0.5929916762886003889 ) ) ;
#37810 = ORIENTED_EDGE ( 'NONE', *, *, #5765, .F. ) ;
#37811 = CARTESIAN_POINT ( 'NONE',  ( 0.1874213080127691833, -0.6920270397579918464, 0.03916149223782419003 ) ) ;
#37812 = CARTESIAN_POINT ( 'NONE',  ( -0.2746410161513770931, -3.156018320128275878, -0.4841849112664152743 ) ) ;
#37813 = EDGE_CURVE ( 'NONE', #858, #9058, #3555, .T. ) ;
#37814 = DIRECTION ( 'NONE',  ( 0.000000000000000000, -0.9246857012436752177, 0.3807313408632029827 ) ) ;
#37815 = CARTESIAN_POINT ( 'NONE',  ( 0.1862096482451259249, -0.7741715863355521643, 0.1916105915568836193 ) ) ;
#37816 = VERTEX_POINT ( 'NONE', #19752 ) ;
#37817 = DIRECTION ( 'NONE',  ( 0.8660512985181133550, 0.4999551463232372317, 0.000000000000000000 ) ) ;
#37818 = EDGE_CURVE ( 'NONE', #16911, #38708, #40444, .T. ) ;
#37819 = CARTESIAN_POINT ( 'NONE',  ( -0.1148620258665538491, -0.5252635219644070652, 0.3299751171063294297 ) ) ;
#37820 = CARTESIAN_POINT ( 'NONE',  ( 0.03113248654051816583, 0.09520121321898405986, -0.1758883992810029440 ) ) ;
#37821 = VECTOR ( 'NONE', #30176, 39.37007874015748143 ) ;
#37822 = EDGE_CURVE ( 'NONE', #35420, #17096, #6283, .T. ) ;
#37823 = FACE_OUTER_BOUND ( 'NONE', #15789, .T. ) ;
#37824 = CARTESIAN_POINT ( 'NONE',  ( 0.3999999999999783173, -2.047156491238096176, -0.7141923294504540776 ) ) ;
#37825 = CARTESIAN_POINT ( 'NONE',  ( 0.2135559776035426960, -1.241076878514266513, 0.5839068764539582235 ) ) ;
#37826 = CARTESIAN_POINT ( 'NONE',  ( 0.08522533823544217735, -1.743361703470160728, -0.6409892287915732734 ) ) ;
#37827 = CARTESIAN_POINT ( 'NONE',  ( 0.1070962762476720537, -1.392980070899417111, 0.6530324985320268283 ) ) ;
#37828 = SHAPE_DEFINITION_REPRESENTATION ( #2158, #35919 ) ;
#37829 = ORGANIZATION ( 'NAUO-ORG2', 'UNSPECIFIED', 'UNSPECIFIED' ) ;
#37830 = CARTESIAN_POINT ( 'NONE',  ( 0.2296032268162506162, -0.9382281285954664485, 0.4302797228108481420 ) ) ;
#37831 = DIRECTION ( 'NONE',  ( 0.000000000000000000, 0.5365213554527469286, -0.8438867430782091006 ) ) ;
#37832 = CARTESIAN_POINT ( 'NONE',  ( 0.5535339714453306748, -1.186249370383523294, 0.6057417262809816627 ) ) ;
#37833 = AXIS2_PLACEMENT_3D ( 'NONE', #38622, #22615, #28954 ) ;
#37834 = CARTESIAN_POINT ( 'NONE',  ( 0.2640734557584212272, -1.686333136531013466, 0.5670960282305730349 ) ) ;
#37835 = EDGE_CURVE ( 'NONE', #12308, #13132, #5511, .T. ) ;
#37836 = PRODUCT_DEFINITION ( 'UNKNOWN', '', #26625, #12449 ) ;
#37837 = CARTESIAN_POINT ( 'NONE',  ( 0.04206944528682795420, -1.152159445897246393, 0.6964886360393780507 ) ) ;
#37838 = CARTESIAN_POINT ( 'NONE',  ( -0.0002424173180945032727, -0.8751502303707813235, -0.01887031899818753314 ) ) ;
#37839 = CYLINDRICAL_SURFACE ( 'NONE', #37017, 0.1000000000000000194 ) ;
#37840 = LINE ( 'NONE', #38033, #15205 ) ;
#37841 = ORIENTED_EDGE ( 'NONE', *, *, #11565, .F. ) ;
#37842 = ORIENTED_EDGE ( 'NONE', *, *, #31088, .T. ) ;
#37843 = FACE_OUTER_BOUND ( 'NONE', #17052, .T. ) ;
#37844 = EDGE_LOOP ( 'NONE', ( #32633, #14165, #15016, #29316 ) ) ;
#37845 = DIRECTION ( 'NONE',  ( 0.8150167559926670968, 0.5794373887239150367, 0.000000000000000000 ) ) ;
#37846 = CARTESIAN_POINT ( 'NONE',  ( -0.05082303569918675268, -0.4330427793496107181, -0.1918498709088775622 ) ) ;
#37847 = CARTESIAN_POINT ( 'NONE',  ( 0.4367679725710939542, -1.201179855909204397, 0.8157569126575382468 ) ) ;
#37849 = ORIENTED_EDGE ( 'NONE', *, *, #8472, .T. ) ;
#37848 = DIRECTION ( 'NONE',  ( -1.000000000000000000, -2.341930812374887555E-31, 1.664003471950578127E-31 ) ) ;
#37850 = CIRCLE ( 'NONE', #25349, 0.09249999999977555343 ) ;
#37851 = AXIS2_PLACEMENT_3D ( 'NONE', #39571, #14472, #1775 ) ;
#37852 = ORIENTED_EDGE ( 'NONE', *, *, #28999, .T. ) ;
#37853 = CARTESIAN_POINT ( 'NONE',  ( 0.1966708302945472664, -0.7872448539783969412, 0.3093500942271054099 ) ) ;
#37854 = ORIENTED_EDGE ( 'NONE', *, *, #3120, .T. ) ;
#37855 = CARTESIAN_POINT ( 'NONE',  ( 0.01624379798718045970, -0.5940688689955531121, 0.3554331757638558020 ) ) ;
#37857 = CARTESIAN_POINT ( 'NONE',  ( 0.6290530482886385055, -1.474716711548147874, 0.5182417262812423209 ) ) ;
#37856 = CARTESIAN_POINT ( 'NONE',  ( 0.1757454679492159444, -0.9123123364095576671, 0.6095604877834991386 ) ) ;
#37858 = FACE_OUTER_BOUND ( 'NONE', #19729, .T. ) ;
#37859 = APPLIED_SECURITY_CLASSIFICATION_ASSIGNMENT ( #14861, ( #40657 ) ) ;
#37860 = CARTESIAN_POINT ( 'NONE',  ( 0.1876953789110183679, -0.9196856789278203825, 0.1479976049341028554 ) ) ;
#37861 = CARTESIAN_POINT ( 'NONE',  ( -2.112273405726188513E-14, -1.835409001655643690, -0.3543101909453316156 ) ) ;
#37863 = VERTEX_POINT ( 'NONE', #13166 ) ;
#37862 = ORIENTED_EDGE ( 'NONE', *, *, #38123, .F. ) ;
#37864 = CARTESIAN_POINT ( 'NONE',  ( -0.01548846960707490547, 0.5198120922912040642, 0.07362328916749247276 ) ) ;
#37865 = AXIS2_PLACEMENT_3D ( 'NONE', #1562, #30134, #26853 ) ;
#37866 = CARTESIAN_POINT ( 'NONE',  ( 0.1642579856227123214, -0.9583868220818564376, 0.4613279698008625473 ) ) ;
#37867 = CARTESIAN_POINT ( 'NONE',  ( 0.1995969790795776300, -2.064390217781732595, -0.7176297154563284764 ) ) ;
#37868 = ADVANCED_FACE ( 'NONE', ( #32101 ), #4284, .F. ) ;
#37869 = CARTESIAN_POINT ( 'NONE',  ( 0.5816238657360307540, -1.478355207367950674, 0.6788288349111909481 ) ) ;
#37870 = DIRECTION ( 'NONE',  ( 9.244463733058726621E-33, 0.4685245517976878160, 0.8834504764630419782 ) ) ;
#37871 = CARTESIAN_POINT ( 'NONE',  ( 0.1805882081786515381, -1.310474468103578038, 0.9369546008279981963 ) ) ;
#37872 = EDGE_CURVE ( 'NONE', #29543, #3269, #32048, .T. ) ;
#37873 = CARTESIAN_POINT ( 'NONE',  ( 0.3080248481530759586, -1.647059832894722131, 0.9156036115443938472 ) ) ;
#37874 = ADVANCED_FACE ( 'NONE', ( #38674 ), #4107, .T. ) ;
#37875 = DIRECTION ( 'NONE',  ( 5.551115123125868984E-17, -5.531779426422974156E-16, -1.000000000000000000 ) ) ;
#37876 = FACE_OUTER_BOUND ( 'NONE', #36917, .T. ) ;
#37877 = LINE ( 'NONE', #6577, #8644 ) ;
#37878 = CYLINDRICAL_SURFACE ( 'NONE', #38477, 0.1000000000000000194 ) ;
#37879 = AXIS2_PLACEMENT_3D ( 'NONE', #10677, #1255, #13757 ) ;
#37880 = CARTESIAN_POINT ( 'NONE',  ( 0.03647060353175276409, -0.3644804546768179443, 0.3593183619073416768 ) ) ;
#37881 = CARTESIAN_POINT ( 'NONE',  ( 0.3122857990831161556, -1.766572940467653785, 0.5980579735034173838 ) ) ;
#37882 = CARTESIAN_POINT ( 'NONE',  ( 0.1758888584962763069, -1.756691831069698173, -0.6511160423431344713 ) ) ;
#37883 = APPROVAL_ROLE ( '' ) ;
#37884 = EDGE_CURVE ( 'NONE', #27710, #34692, #16466, .T. ) ;
#37885 = DIRECTION ( 'NONE',  ( 0.4017000971270622278, 0.2318939203356582823, -0.8859245124046789543 ) ) ;
#37886 = B_SPLINE_CURVE_WITH_KNOTS ( 'NONE', 3,
 ( #9045, #38, #9229, #24479 ),
 .UNSPECIFIED., .F., .F.,
 ( 4, 4 ),
 ( 0.000000000000000000, 0.0001096403195332056003 ),
 .UNSPECIFIED. ) ;
#37887 = CARTESIAN_POINT ( 'NONE',  ( -0.03674078017396703588, 0.4681991728402010167, 0.1092756390057632171 ) ) ;
#37888 = CARTESIAN_POINT ( 'NONE',  ( 0.7053833034112568789, -1.492524922043918734, 0.5185182801802852293 ) ) ;
#37889 = CIRCLE ( 'NONE', #20166, 0.04749999999977558285 ) ;
#37890 = VERTEX_POINT ( 'NONE', #13591 ) ;
#37891 = LINE ( 'NONE', #35600, #37544 ) ;
#37892 = ORIENTED_EDGE ( 'NONE', *, *, #14278, .T. ) ;
#37893 = CARTESIAN_POINT ( 'NONE',  ( 0.3591498995103406533, -1.737620376665804933, -0.5147966178037263196 ) ) ;
#37894 = CARTESIAN_POINT ( 'NONE',  ( 0.1854879680645313555, -1.345035247216854302, 0.9498699178978792235 ) ) ;
#37895 = CARTESIAN_POINT ( 'NONE',  ( 0.1327162649517526216, -0.5774347627937225225, 0.2565431035860060716 ) ) ;
#37897 = ORIENTED_EDGE ( 'NONE', *, *, #16494, .T. ) ;
#37896 = CARTESIAN_POINT ( 'NONE',  ( 0.3725959361440046025, -1.740293560479224011, 0.4320537422923894089 ) ) ;
#37899 = VERTEX_POINT ( 'NONE', #16277 ) ;
#37898 = ORIENTED_EDGE ( 'NONE', *, *, #26598, .F. ) ;
#37900 = CARTESIAN_POINT ( 'NONE',  ( -0.2399999999999999079, -3.196602950345407645, -0.1969487268370971322 ) ) ;
#37901 = VERTEX_POINT ( 'NONE', #29423 ) ;
#37902 = CARTESIAN_POINT ( 'NONE',  ( 0.6214629568584182362, -1.607011684701395993, -0.5680849726491742357 ) ) ;
#37903 = CALENDAR_DATE ( 2026, 13, 10 ) ;
#37904 = CARTESIAN_POINT ( 'NONE',  ( 0.3047942498816851864, -1.756876866921070146, 0.5683792054161904694 ) ) ;
#37905 = VERTEX_POINT ( 'NONE', #23055 ) ;
#37906 = CIRCLE ( 'NONE', #35937, 0.01500000000000004108 ) ;
#37907 = CARTESIAN_POINT ( 'NONE',  ( 0.08584567903155965185, -0.7460567843300380808, 0.1457185332388686860 ) ) ;
#37908 = EDGE_CURVE ( 'NONE', #591, #27450, #30582, .T. ) ;
#37909 = CARTESIAN_POINT ( 'NONE',  ( -0.3000000000000000999, -3.985676108854518507, -0.7623095129438225426 ) ) ;
#37910 = CARTESIAN_POINT ( 'NONE',  ( 0.5253282373615071332, -1.526886051446876280, 0.5751798715530015427 ) ) ;
#37911 = CARTESIAN_POINT ( 'NONE',  ( 0.6356291811816829895, -1.489535549261238767, -0.6355727712968906040 ) ) ;
#37912 = DIRECTION ( 'NONE',  ( 0.000000000000000000, 0.9510565162951442053, 0.3090169943749759840 ) ) ;
#37913 = ORIENTED_EDGE ( 'NONE', *, *, #30356, .F. ) ;
#37914 = EDGE_CURVE ( 'NONE', #11635, #18456, #32495, .T. ) ;
#37915 = B_SPLINE_CURVE_WITH_KNOTS ( 'NONE', 3,
 ( #9673, #34756, #6563, #19140 ),
 .UNSPECIFIED., .F., .F.,
 ( 4, 4 ),
 ( 3.150947443209742121E-16, 0.0008530918207275374129 ),
 .UNSPECIFIED. ) ;
#37916 = CARTESIAN_POINT ( 'NONE',  ( 0.4574846914228954953, -1.692033587742871381, 0.5885383685939118426 ) ) ;
#37917 = CARTESIAN_POINT ( 'NONE',  ( 0.6560342951817995649, -1.361138816048402145, 0.7673092742682359191 ) ) ;
#37918 = DIRECTION ( 'NONE',  ( -0.4999999999999948375, 0.7066258520834660661, 0.5006794435238187679 ) ) ;
#37919 = CARTESIAN_POINT ( 'NONE',  ( 0.6086752090503105839, -1.478944523047028392, 0.5656203117916941414 ) ) ;
#37920 = CARTESIAN_POINT ( 'NONE',  ( -0.3000000000000000999, -4.218511633990150500, -0.6415916474861803609 ) ) ;
#37921 = ADVANCED_FACE ( 'NONE', ( #22669 ), #2334, .F. ) ;
#37922 = CARTESIAN_POINT ( 'NONE',  ( 0.4093611158985690501, -1.131941421409890403, 0.5197417262808780025 ) ) ;
#37923 = CARTESIAN_POINT ( 'NONE',  ( 0.4654555503626408020, -1.098995021068088773, -0.3936018329855539566 ) ) ;
#37924 = CARTESIAN_POINT ( 'NONE',  ( 0.05889106705834949718, -1.326084810051836982, 0.5931655932887337501 ) ) ;
#37925 = CARTESIAN_POINT ( 'NONE',  ( 0.5055437690763310288, -1.106959495255247505, 0.6108412925465283028 ) ) ;
#37926 = PERSON_AND_ORGANIZATION ( #28500, #32463 ) ;
#37927 = DIRECTION ( 'NONE',  ( 0.000000000000000000, 0.000000000000000000, -1.000000000000000000 ) ) ;
#37928 = ADVANCED_FACE ( 'NONE', ( #1462 ), #19960, .T. ) ;
#37929 = APPROVAL ( #1701, 'UNKNOWN' ) ;
#37930 = ADVANCED_FACE ( 'NONE', ( #38481 ), #1270, .T. ) ;
#37931 = CARTESIAN_POINT ( 'NONE',  ( 0.5377610847061485844, -1.519774373043595972, 0.5731039079555608762 ) ) ;
#37932 = CARTESIAN_POINT ( 'NONE',  ( -0.05252049209742314095, -0.009108187116140229606, 0.4689942714594981243 ) ) ;
#37933 = ORIENTED_EDGE ( 'NONE', *, *, #1471, .F. ) ;
#37934 = CARTESIAN_POINT ( 'NONE',  ( 5.598961119911192370E-16, -0.2981948553318921058, -0.06819284191469447698 ) ) ;
#37935 = CARTESIAN_POINT ( 'NONE',  ( 0.06980746140711596714, 0.1750000000000001832, 0.000000000000000000 ) ) ;
#37936 = PLANE ( 'NONE',  #27229 ) ;
#37937 = VERTEX_POINT ( 'NONE', #19570 ) ;
#37938 = CARTESIAN_POINT ( 'NONE',  ( 0.3407574567498363183, -1.752395144162200546, 0.4551695278380876730 ) ) ;
#37939 = CARTESIAN_POINT ( 'NONE',  ( 0.0008401815153994757679, -0.9312571135744077688, 0.5924458961409151403 ) ) ;
#37941 = ORIENTED_EDGE ( 'NONE', *, *, #387, .T. ) ;
#37940 = ORIENTED_EDGE ( 'NONE', *, *, #4202, .F. ) ;
#37942 = FACE_OUTER_BOUND ( 'NONE', #19718, .T. ) ;
#37943 = ORIENTED_EDGE ( 'NONE', *, *, #34699, .T. ) ;
#37944 = DIRECTION ( 'NONE',  ( 0.000000000000000000, 0.000000000000000000, -1.000000000000000000 ) ) ;
#37945 = CARTESIAN_POINT ( 'NONE',  ( 0.3812837827729997908, -1.707230790293840172, -0.3372124425115716195 ) ) ;
#37947 = LINE ( 'NONE', #32727, #3785 ) ;
#37946 = CARTESIAN_POINT ( 'NONE',  ( 0.5997906010433834423, -1.596574738763893109, 0.4303942190982675831 ) ) ;
#37948 = CARTESIAN_POINT ( 'NONE',  ( -0.1743922129835736579, -0.5166151207188712791, 0.1000000000000000194 ) ) ;
#37949 = B_SPLINE_CURVE_WITH_KNOTS ( 'NONE', 3,
 ( #8748, #9353, #30572, #5852, #21933, #30768, #37529, #2397 ),
 .UNSPECIFIED., .F., .F.,
 ( 4, 2, 2, 4 ),
 ( 0.000000000000000000, 0.0002823184703889531472, 0.0005646369407779062944, 0.001129273881555797193 ),
 .UNSPECIFIED. ) ;
#37950 = ORIENTED_EDGE ( 'NONE', *, *, #12329, .T. ) ;
#37951 = CARTESIAN_POINT ( 'NONE',  ( 0.01025536129965940943, -0.5346927715679482551, 0.1046735957568519643 ) ) ;
#37952 = VERTEX_POINT ( 'NONE', #34981 ) ;
#37953 = CARTESIAN_POINT ( 'NONE',  ( 0.1000121428524311934, -0.6364596608959190993, 0.3289196408185624532 ) ) ;
#37954 = VERTEX_POINT ( 'NONE', #38865 ) ;
#37955 = CARTESIAN_POINT ( 'NONE',  ( 0.0004750028870838371897, -0.4386152171684600254, 0.1457185332388682975 ) ) ;
#37956 = CARTESIAN_POINT ( 'NONE',  ( 0.3607945552467097805, -1.331973876078468955, 0.8646488368460186758 ) ) ;
#37958 = CARTESIAN_POINT ( 'NONE',  ( -0.08000000000000000167, -2.023118915020511999, -0.4686803309516410221 ) ) ;
#37957 = CARTESIAN_POINT ( 'NONE',  ( 0.4356662251172992439, -1.610775558009423847, -0.3686272921855577867 ) ) ;
#37959 = CARTESIAN_POINT ( 'NONE',  ( 0.4924701362321921017, -1.025257283658408403, -0.5155029497116575543 ) ) ;
#37960 = DIRECTION ( 'NONE',  ( 0.000000000000000000, 0.000000000000000000, -1.000000000000000000 ) ) ;
#37961 = ADVANCED_FACE ( 'NONE', ( #10311 ), #10875, .T. ) ;
#37962 = DIRECTION ( 'NONE',  ( 0.000000000000000000, -3.885780586188049371E-16, -1.000000000000000000 ) ) ;
#37963 = CARTESIAN_POINT ( 'NONE',  ( 0.3967242239788378311, -1.726942646203573517, -0.3050504165543944657 ) ) ;
#37964 = ADVANCED_FACE ( 'NONE', ( #7183 ), #33497, .F. ) ;
#37965 = CARTESIAN_POINT ( 'NONE',  ( 0.3026669703120153376, -1.007674124269388294, 0.7664178669992703918 ) ) ;
#37966 = CARTESIAN_POINT ( 'NONE',  ( -0.05616044724337223432, 0.2616774468955962440, -0.3775835982344354358 ) ) ;
#37967 =( BOUNDED_SURFACE ( )  B_SPLINE_SURFACE ( 3, 2, ( 
 ( #32169, #26027, #16950 ),
 ( #10170, #32974, #29696 ),
 ( #32576, #36068, #3979 ),
 ( #29911, #23551, #32361 ),
 ( #1539, #23353, #14060 ),
 ( #29491, #38547, #16754 ),
 ( #10563, #14264, #22738 ),
 ( #16541, #35664, #29083 ) ),
 .UNSPECIFIED., .F., .F., .T. ) 
 B_SPLINE_SURFACE_WITH_KNOTS ( ( 4, 2, 2, 4 ),
 ( 3, 3 ),
 ( -1.735946658636840947E-05, 0.002957348748439985603, 0.004444702855953162543, 0.005932056963466339483 ),
 ( 0.000000000000000000, 1.000000000000000000 ),
 .UNSPECIFIED. ) 
 GEOMETRIC_REPRESENTATION_ITEM ( )  RATIONAL_B_SPLINE_SURFACE ( (
 ( 1.000000000000000000, 1.000000000000000000, 1.000000000000000000),
 ( 1.000000000000000000, 0.9999719623954188563, 1.000000000000000000),
 ( 1.000000000000000000, 0.9935697921326018811, 1.000000000000000000),
 ( 1.000000000000000000, 0.9839453963689780425, 1.000000000000000000),
 ( 1.000000000000000000, 0.9807074542717970633, 1.000000000000000000),
 ( 1.000000000000000000, 0.9760289094675052013, 1.000000000000000000),
 ( 1.000000000000000000, 0.9745874693094034313, 1.000000000000000000),
 ( 1.000000000000000000, 0.9750816781289051161, 1.000000000000000000) ) ) 
 REPRESENTATION_ITEM ( '' )  SURFACE ( )  );
#37968 = CARTESIAN_POINT ( 'NONE',  ( -0.02000000000000000042, -1.598492537578166672, -0.1971380022280825872 ) ) ;
#37969 = CARTESIAN_POINT ( 'NONE',  ( -0.04285534776242287680, -0.4433434382090528647, -0.2197501713291542813 ) ) ;
#37970 = CARTESIAN_POINT ( 'NONE',  ( 0.05999999999999990757, 0.000000000000000000, 0.000000000000000000 ) ) ;
#37971 = CARTESIAN_POINT ( 'NONE',  ( 0.5154728982652437841, -1.185177693224150008, 0.4436066727502508411 ) ) ;
#37972 = CARTESIAN_POINT ( 'NONE',  ( 0.5586414499496984432, -1.205790344466990627, 0.8068181458027993136 ) ) ;
#37973 = CARTESIAN_POINT ( 'NONE',  ( 0.5099280420869274355, -1.114989880839767578, 0.5367823920641713320 ) ) ;
#37974 = CARTESIAN_POINT ( 'NONE',  ( 0.05800524771820539383, -1.293462930650507214, 0.6434660951334953971 ) ) ;
#37975 = CARTESIAN_POINT ( 'NONE',  ( 0.05561375719525413902, 0.4316271021131491969, -0.1617018132803443586 ) ) ;
#37976 = CARTESIAN_POINT ( 'NONE',  ( 0.3999094372835061972, -2.086652961537767137, -0.4708658242691809992 ) ) ;
#37977 = CARTESIAN_POINT ( 'NONE',  ( 0.1939270537251513438, -0.9059543765946825866, 0.6046208699968631528 ) ) ;
#37978 = DIRECTION ( 'NONE',  ( 1.000000000000000000, -0.000000000000000000, -0.000000000000000000 ) ) ;
#37979 = CARTESIAN_POINT ( 'NONE',  ( 0.6862067491206771397, -1.510281502546922949, 0.4567439642065846406 ) ) ;
#37980 = ORIENTED_EDGE ( 'NONE', *, *, #34629, .T. ) ;
#37981 = DIRECTION ( 'NONE',  ( 0.000000000000000000, 0.000000000000000000, -1.000000000000000000 ) ) ;
#37982 = CARTESIAN_POINT ( 'NONE',  ( 0.1977209903153200055, -0.8506692363503495224, 0.6350317236410694122 ) ) ;
#37983 = CARTESIAN_POINT ( 'NONE',  ( 0.6584301049649089466, -1.489287037793245227, 0.4182417262808776903 ) ) ;
#37984 = CARTESIAN_POINT ( 'NONE',  ( 0.5320511322164590551, -1.669038612624452744, -0.4503538000400599262 ) ) ;
#37985 = ADVANCED_FACE ( 'NONE', ( #20577 ), #11304, .F. ) ;
#37986 = CARTESIAN_POINT ( 'NONE',  ( 0.3874608430265089609, -1.108326039081300785, 0.6051049422084413543 ) ) ;
#37987 = VERTEX_POINT ( 'NONE', #11518 ) ;
#37988 = CARTESIAN_POINT ( 'NONE',  ( 0.3959480418811466840, -1.613405948999770523, -0.6688934733077330774 ) ) ;
#37989 = CARTESIAN_POINT ( 'NONE',  ( 0.3315018707368336259, -1.291415966887107247, 0.5178325263893220898 ) ) ;
#37990 = DIRECTION ( 'NONE',  ( 1.000000000000000000, 0.000000000000000000, 0.000000000000000000 ) ) ;
#37991 = CYLINDRICAL_SURFACE ( 'NONE', #15378, 0.01500000000000004975 ) ;
#37992 = CARTESIAN_POINT ( 'NONE',  ( 0.4258910459772873858, -1.183759126590261168, 0.7367376598851150815 ) ) ;
#37994 = LINE ( 'NONE', #412, #24706 ) ;
#37993 = CARTESIAN_POINT ( 'NONE',  ( 0.4559719632891929830, -1.698713290701216350, -0.5155029497116575543 ) ) ;
#37995 = CARTESIAN_POINT ( 'NONE',  ( 0.4083208966368579995, -1.036284369767852764, 0.6331064141399478373 ) ) ;
#37996 = ORIENTED_EDGE ( 'NONE', *, *, #13768, .F. ) ;
#37997 = CALENDAR_DATE ( 2026, 13, 10 ) ;
#37998 = B_SPLINE_CURVE_WITH_KNOTS ( 'NONE', 3,
 ( #22212, #25685, #6535, #34933, #9429, #15809, #25072, #19703, #6948, #228 ),
 .UNSPECIFIED., .F., .F.,
 ( 4, 2, 2, 2, 4 ),
 ( 0.0008171848362502084993, 0.001788850595559428845, 0.002760516354868649408, 0.003732182114177869103, 0.004703847873487089666 ),
 .UNSPECIFIED. ) ;
#37999 = CARTESIAN_POINT ( 'NONE',  ( 0.09498762465003944555, -1.342648412413370407, 0.6966705301549200868 ) ) ;
#38000 = ORIENTED_EDGE ( 'NONE', *, *, #37639, .F. ) ;
#38001 = EDGE_LOOP ( 'NONE', ( #35320, #29042, #14733, #33613 ) ) ;
#38002 = CARTESIAN_POINT ( 'NONE',  ( 0.3036885249178302715, -1.390984769928044651, 0.8913742401028124096 ) ) ;
#38004 = CARTESIAN_POINT ( 'NONE',  ( 0.1996428621479708065, -0.6036337479795305105, 0.3287165209465360283 ) ) ;
#38003 = CARTESIAN_POINT ( 'NONE',  ( -0.2746410161513776482, -3.941790907013290823, -0.4709369376873030477 ) ) ;
#38005 = CARTESIAN_POINT ( 'NONE',  ( 0.6001884367015531963, -1.607799423540326567, 0.4311405334566375536 ) ) ;
#38006 = VERTEX_POINT ( 'NONE', #17870 ) ;
#38007 = VERTEX_POINT ( 'NONE', #5524 ) ;
#38008 = ORIENTED_EDGE ( 'NONE', *, *, #36565, .F. ) ;
#38009 = CARTESIAN_POINT ( 'NONE',  ( -0.2399999999999999079, -3.156018320128275878, -0.4841849112664152743 ) ) ;
#38010 = CARTESIAN_POINT ( 'NONE',  ( 0.1181822409742579877, -0.5775493957728874417, 0.2649829690098590707 ) ) ;
#38011 = ORIENTED_EDGE ( 'NONE', *, *, #35182, .T. ) ;
#38012 = CARTESIAN_POINT ( 'NONE',  ( 0.07556315841227323471, -1.331191507351497716, 0.4849083929475445087 ) ) ;
#38013 = CARTESIAN_POINT ( 'NONE',  ( 0.4732031336055909643, -1.076730694904952434, -0.6086252408385472989 ) ) ;
#38014 = FACE_BOUND ( 'NONE', #14988, .T. ) ;
#38015 = CARTESIAN_POINT ( 'NONE',  ( 0.4547563268321924701, -1.664835936145135031, -0.6217598108907549381 ) ) ;
#38016 = ORIENTED_EDGE ( 'NONE', *, *, #30034, .F. ) ;
#38017 = CARTESIAN_POINT ( 'NONE',  ( 0.02999999999997886302, -2.183180860297921466, -0.4937760292030871079 ) ) ;
#38018 = DIRECTION ( 'NONE',  ( 1.000000000000000000, -0.000000000000000000, -0.000000000000000000 ) ) ;
#38019 = CARTESIAN_POINT ( 'NONE',  ( 0.08750309474107365038, -0.6863091869244348775, 0.02122045413186614618 ) ) ;
#38020 = CARTESIAN_POINT ( 'NONE',  ( 0.7371735653322752935, -1.498976209023650696, 0.6847608182276055944 ) ) ;
#38021 = CARTESIAN_POINT ( 'NONE',  ( 0.1968880119611848278, -2.022044081434100971, -0.7071002453052855907 ) ) ;
#38022 = DIRECTION ( 'NONE',  ( 0.000000000000000000, 0.3090169943749439541, -0.9510565162951547524 ) ) ;
#38023 = CARTESIAN_POINT ( 'NONE',  ( -4.314083075427408721E-33, -0.03575622569115821658, -0.1978615321325044307 ) ) ;
#38024 = CARTESIAN_POINT ( 'NONE',  ( 0.1117854919768572763, -1.404504638728010679, 0.6272293575327468895 ) ) ;
#38025 = APPROVAL_STATUS ( 'not_yet_approved' ) ;
#38026 = DIRECTION ( 'NONE',  ( 0.4999551463232372317, -0.8660512985181134660, -0.000000000000000000 ) ) ;
#38027 = DIRECTION ( 'NONE',  ( -0.9378410757839567014, 0.1072489841977716934, 0.3300784330442341763 ) ) ;
#38028 = FACE_OUTER_BOUND ( 'NONE', #14783, .T. ) ;
#38029 = DIRECTION ( 'NONE',  ( 0.000000000000000000, 0.000000000000000000, -1.000000000000000000 ) ) ;
#38030 = CARTESIAN_POINT ( 'NONE',  ( 0.03762609415277568675, -1.032875954121303508, 0.6996461994120862782 ) ) ;
#38031 = CARTESIAN_POINT ( 'NONE',  ( 0.0003774071935349580386, -0.4512940697347599950, 0.06537198606400290712 ) ) ;
#38032 = CARTESIAN_POINT ( 'NONE',  ( 0.4356662251172990774, -1.610775558009424735, -0.3686272921855577867 ) ) ;
#38033 = CARTESIAN_POINT ( 'NONE',  ( -0.2746410161513776482, -3.753843787845913216, -0.2458487048530572650 ) ) ;
#38034 = VERTEX_POINT ( 'NONE', #11712 ) ;
#38035 = ORIENTED_EDGE ( 'NONE', *, *, #3230, .F. ) ;
#38036 = CARTESIAN_POINT ( 'NONE',  ( 2.185478394931410575E-15, -0.2949999999999994293, -9.902948977032954413E-16 ) ) ;
#38037 = ORIENTED_EDGE ( 'NONE', *, *, #13558, .F. ) ;
#38038 = CARTESIAN_POINT ( 'NONE',  ( -0.2399999999999999079, -1.730153431576819001, -0.08301574631829765349 ) ) ;
#38039 = DIRECTION ( 'NONE',  ( 0.000000000000000000, 0.000000000000000000, -1.000000000000000000 ) ) ;
#38040 = CARTESIAN_POINT ( 'NONE',  ( 0.6252342874366797476, -1.468101632537779366, 0.5255929057819803685 ) ) ;
#38042 = VERTEX_POINT ( 'NONE', #39473 ) ;
#38041 = CARTESIAN_POINT ( 'NONE',  ( 0.000000000000000000, -0.02999999999999995379, 0.000000000000000000 ) ) ;
#38043 = EDGE_CURVE ( 'NONE', #16451, #4940, #39393, .T. ) ;
#38044 = ORIENTED_EDGE ( 'NONE', *, *, #15699, .T. ) ;
#38045 = CARTESIAN_POINT ( 'NONE',  ( 0.5574173260714455624, -1.620431899042181545, 0.4862486760544370568 ) ) ;
#38046 = ORIENTED_EDGE ( 'NONE', *, *, #11295, .T. ) ;
#38047 = CARTESIAN_POINT ( 'NONE',  ( 0.04452036461275030166, -0.7338017871114075330, 0.5870408077749112996 ) ) ;
#38049 = CARTESIAN_POINT ( 'NONE',  ( 0.2158254279709804768, -1.357966257267858134, 0.4182417262808779679 ) ) ;
#38048 = DIRECTION ( 'NONE',  ( 0.000000000000000000, -0.6595282642760673664, -0.7516797646744242112 ) ) ;
#38050 = CARTESIAN_POINT ( 'NONE',  ( 0.01180287247555067420, -0.6200342144150551293, -0.1048702747917058531 ) ) ;
#38051 = CARTESIAN_POINT ( 'NONE',  ( 5.388056259091479659E-16, -0.2899999999999993694, 0.04249999999999923284 ) ) ;
#38053 = ORIENTED_EDGE ( 'NONE', *, *, #29496, .T. ) ;
#38052 = ORIENTED_EDGE ( 'NONE', *, *, #20230, .F. ) ;
#38054 = DIRECTION ( 'NONE',  ( 0.8660512985181132439, 0.4999551463232376758, 0.000000000000000000 ) ) ;
#38055 = CARTESIAN_POINT ( 'NONE',  ( 0.2165169723861147255, -0.9316405093292169370, 0.3921959536928056322 ) ) ;
#38056 = FACE_OUTER_BOUND ( 'NONE', #8200, .T. ) ;
#38057 = CARTESIAN_POINT ( 'NONE',  ( -2.112273405726188513E-14, -2.104523474114237125, -0.2882858665344287807 ) ) ;
#38058 = EDGE_CURVE ( 'NONE', #7985, #30726, #27152, .T. ) ;
#38059 = LINE ( 'NONE', #22053, #6702 ) ;
#38060 = DIRECTION ( 'NONE',  ( 1.000000000000000000, 1.445897915516965072E-15, -8.881784197001242463E-16 ) ) ;
#38061 = APPLIED_DATE_AND_TIME_ASSIGNMENT ( #9739, #19007, ( #26657 ) ) ;
#38062 = CARTESIAN_POINT ( 'NONE',  ( 0.4768212070748857889, -1.161171340586348411, 0.4226408848665243467 ) ) ;
#38063 = CARTESIAN_POINT ( 'NONE',  ( -0.1167294259372886056, -0.5331983348239501819, 0.3749999999999996669 ) ) ;
#38064 = LINE ( 'NONE', #12775, #1580 ) ;
#38065 = DIRECTION ( 'NONE',  ( -0.9117016142544763779, -0.4108529743908177490, -1.183049357217560165E-13 ) ) ;
#38066 = CARTESIAN_POINT ( 'NONE',  ( 0.01548846960706677829, -0.4638115001431235562, -0.2459753896937935114 ) ) ;
#38067 = DIRECTION ( 'NONE',  ( 1.000000000000000000, 0.000000000000000000, 0.000000000000000000 ) ) ;
#38068 = CARTESIAN_POINT ( 'NONE',  ( 0.02872242845529797070, -0.3729171224323792888, 0.3802687114177617511 ) ) ;
#38069 = CARTESIAN_POINT ( 'NONE',  ( -0.1743922129835736579, -0.5166151207188712791, 0.1000000000000000194 ) ) ;
#38070 = CARTESIAN_POINT ( 'NONE',  ( 0.1186213546926599971, -1.414144755877529969, 0.5682417269582831221 ) ) ;
#38071 = PERSON_AND_ORGANIZATION ( #28500, #32463 ) ;
#38072 = CARTESIAN_POINT ( 'NONE',  ( 0.3732864473234233649, -1.732922991205104735, -0.4865963089983659229 ) ) ;
#38073 = CARTESIAN_POINT ( 'NONE',  ( -0.04047043078436820401, 0.4923670751789595568, 0.09403524049742544022 ) ) ;
#38074 = CARTESIAN_POINT ( 'NONE',  ( 0.01548846960707528191, 0.3772621329472714558, 0.3651003739303416706 ) ) ;
#38075 = EDGE_CURVE ( 'NONE', #38007, #24330, #35459, .T. ) ;
#38076 = ADVANCED_FACE ( 'NONE', ( #23664 ), #6249, .F. ) ;
#38077 = DIRECTION ( 'NONE',  ( 1.000000000000000000, 1.450080480853946466E-15, -8.188689774234050758E-16 ) ) ;
#38078 = VERTEX_POINT ( 'NONE', #5115 ) ;
#38079 = DIRECTION ( 'NONE',  ( -0.4999551463232377313, 0.8660512985181132439, -0.000000000000000000 ) ) ;
#38080 = CARTESIAN_POINT ( 'NONE',  ( 0.2721694418667137683, -1.673780725527275415, 0.6241958521473389698 ) ) ;
#38081 = EDGE_CURVE ( 'NONE', #14602, #3320, #16139, .T. ) ;
#38082 = CARTESIAN_POINT ( 'NONE',  ( 0.5945617714832603928, -1.487100328519615378, 0.5656869075730865948 ) ) ;
#38083 = EDGE_CURVE ( 'NONE', #28470, #12691, #3011, .T. ) ;
#38085 = VERTEX_POINT ( 'NONE', #17485 ) ;
#38084 = CARTESIAN_POINT ( 'NONE',  ( 0.5511291867232482877, -1.181973051624798376, 0.6053111933194494920 ) ) ;
#38086 = EDGE_CURVE ( 'NONE', #23555, #2251, #16832, .T. ) ;
#38088 = EDGE_LOOP ( 'NONE', ( #28709, #18461, #9567, #8293 ) ) ;
#38087 = ORIENTED_EDGE ( 'NONE', *, *, #18962, .F. ) ;
#38089 = CARTESIAN_POINT ( 'NONE',  ( -0.2399999999999999079, -2.289343986263487896, -0.7686455968847020204 ) ) ;
#38090 = ORIENTED_EDGE ( 'NONE', *, *, #28811, .T. ) ;
#38091 = CARTESIAN_POINT ( 'NONE',  ( -0.1687956829044022500, 0.4914472887403520951, 0.1310621546645153179 ) ) ;
#38092 = PERSON_AND_ORGANIZATION_ROLE ( 'classification_officer' ) ;
#38093 = CARTESIAN_POINT ( 'NONE',  ( 0.1937211450672182700, -1.200652605839983345, 0.5182417262812423209 ) ) ;
#38094 = ORIENTED_EDGE ( 'NONE', *, *, #38178, .T. ) ;
#38095 = CARTESIAN_POINT ( 'NONE',  ( 0.1790044836746327306, -0.8586862843173230786, 0.5897763735302309351 ) ) ;
#38096 = CARTESIAN_POINT ( 'NONE',  ( 0.06924657340767528813, -0.5400045880099110240, 0.1446695161202853908 ) ) ;
#38097 = CARTESIAN_POINT ( 'NONE',  ( 0.3019806439885205362, -1.080587002428585075, 0.8099453515258236980 ) ) ;
#38098 = CARTESIAN_POINT ( 'NONE',  ( 0.6323818217483841986, -1.501417540436901454, -0.6354249433986968176 ) ) ;
#38099 = EDGE_CURVE ( 'NONE', #4081, #26629, #11106, .T. ) ;
#38100 = CARTESIAN_POINT ( 'NONE',  ( -0.1683868308082382692, 0.4901225108767979788, 0.1298109267597956917 ) ) ;
#38101 = CARTESIAN_POINT ( 'NONE',  ( -0.1681560115201613526, 0.5223552577132001273, 0.1414989390318074358 ) ) ;
#38102 = ORIENTED_EDGE ( 'NONE', *, *, #14563, .F. ) ;
#38103 = AXIS2_PLACEMENT_3D ( 'NONE', #11897, #11505, #21782 ) ;
#38104 = CARTESIAN_POINT ( 'NONE',  ( 0.4191100986681001173, -1.701672718972385701, 0.4233639548768205474 ) ) ;
#38105 = CARTESIAN_POINT ( 'NONE',  ( 0.7437942939300432599, -1.516352026067812497, 0.5793574310342267664 ) ) ;
#38106 = CARTESIAN_POINT ( 'NONE',  ( 0.5382321766149029685, -1.161161941655082241, 0.5682417262808779901 ) ) ;
#38107 = AXIS2_PLACEMENT_3D ( 'NONE', #28967, #16634, #34946 ) ;
#38108 = CARTESIAN_POINT ( 'NONE',  ( 0.1373265930037192717, -0.5877730220021950558, 0.2830141842532937768 ) ) ;
#38109 = CARTESIAN_POINT ( 'NONE',  ( 0.02953079040095673430, -0.5250338024619264354, 0.07436286310882474215 ) ) ;
#38110 =( NAMED_UNIT ( * ) PLANE_ANGLE_UNIT ( ) SI_UNIT ( $, .RADIAN. ) );
#38111 = CARTESIAN_POINT ( 'NONE',  ( 0.3211756810167746834, -1.183199798883805887, 0.5707417262808780478 ) ) ;
#38112 = DIRECTION ( 'NONE',  ( -1.188678714063518819E-15, 1.000000000000000000, 0.000000000000000000 ) ) ;
#38113 = CARTESIAN_POINT ( 'NONE',  ( 0.001991602493628476505, -0.9268535620581923595, 0.4078208622452191290 ) ) ;
#38114 = CARTESIAN_POINT ( 'NONE',  ( 0.5108734140540642787, -1.113869616463002643, 0.5959577563698095215 ) ) ;
#38115 = COORDINATED_UNIVERSAL_TIME_OFFSET ( 0, 0, .AHEAD. ) ;
#38116 = DIRECTION ( 'NONE',  ( -1.000000000000000000, -2.276539994720197063E-15, 5.691349986800492658E-16 ) ) ;
#38117 = LINE ( 'NONE', #35650, #9653 ) ;
#38118 = CARTESIAN_POINT ( 'NONE',  ( -0.02872242845530525307, 0.07817994906157108015, 0.5268390348591135419 ) ) ;
#38119 = EDGE_CURVE ( 'NONE', #35619, #32432, #10230, .T. ) ;
#38120 = ORIENTED_EDGE ( 'NONE', *, *, #13555, .F. ) ;
#38121 = CARTESIAN_POINT ( 'NONE',  ( 0.4355462401912356674, -1.577933922365856612, 0.5993494760761562956 ) ) ;
#38122 = CARTESIAN_POINT ( 'NONE',  ( 0.02999999999997886302, -2.183180860297921466, -0.2437760292030870524 ) ) ;
#38123 = EDGE_CURVE ( 'NONE', #22522, #19084, #34507, .T. ) ;
#38124 = AXIS2_PLACEMENT_3D ( 'NONE', #20292, #16801, #19876 ) ;
#38125 = FACE_OUTER_BOUND ( 'NONE', #17291, .T. ) ;
#38126 = ORIENTED_EDGE ( 'NONE', *, *, #15745, .F. ) ;
#38127 = CARTESIAN_POINT ( 'NONE',  ( 0.05573493074139709846, -1.335442843293342063, 0.4177417262808780229 ) ) ;
#38128 = EDGE_CURVE ( 'NONE', #20955, #26127, #29286, .T. ) ;
#38129 = CARTESIAN_POINT ( 'NONE',  ( 0.06979003654356794040, -1.061296314535375540, 0.7344295544536164622 ) ) ;
#38131 = VERTEX_POINT ( 'NONE', #9218 ) ;
#38130 = ORIENTED_EDGE ( 'NONE', *, *, #20087, .T. ) ;
#38132 = DIRECTION ( 'NONE',  ( 0.000000000000000000, 0.4393346272636315941, -0.8983234858819654223 ) ) ;
#38133 = VECTOR ( 'NONE', #39301, 39.37007874015748854 ) ;
#38134 = FACE_OUTER_BOUND ( 'NONE', #15992, .T. ) ;
#38135 = CARTESIAN_POINT ( 'NONE',  ( 0.01548846960707524721, -0.09061086148575756005, -0.5171215251571035232 ) ) ;
#38136 = VECTOR ( 'NONE', #18369, 39.37007874015748143 ) ;
#38137 = DIRECTION ( 'NONE',  ( 1.000000000000000000, 1.693379103678900805E-12, -2.967165974375313612E-13 ) ) ;
#38138 = DIRECTION ( 'NONE',  ( 1.000000000000000000, -0.000000000000000000, -0.000000000000000000 ) ) ;
#38139 = EDGE_LOOP ( 'NONE', ( #33084, #35214, #21113 ) ) ;
#38140 = CARTESIAN_POINT ( 'NONE',  ( 0.01562499999999999827, -0.4290069966815236446, 0.1935973392073239430 ) ) ;
#38141 = ORIENTED_EDGE ( 'NONE', *, *, #17292, .T. ) ;
#38142 = ORIENTED_EDGE ( 'NONE', *, *, #27838, .T. ) ;
#38143 = CARTESIAN_POINT ( 'NONE',  ( 0.1880902979351556092, -0.8183675832216642521, 0.6251957213044665451 ) ) ;
#38144 = ORIENTED_EDGE ( 'NONE', *, *, #17759, .F. ) ;
#38145 = CARTESIAN_POINT ( 'NONE',  ( 0.02567193737592736447, -0.6182554903973285221, 0.6062124708192494493 ) ) ;
#38146 = CARTESIAN_POINT ( 'NONE',  ( 0.4390231747115009853, -1.490295986258741046, 0.7935392936339821235 ) ) ;
#38147 = ADVANCED_FACE ( 'NONE', ( #21789 ), #15616, .F. ) ;
#38149 = CARTESIAN_POINT ( 'NONE',  ( -0.08000000000000000167, -2.626773565144302935, -0.2726934094652516127 ) ) ;
#38148 = CARTESIAN_POINT ( 'NONE',  ( 0.02587840337265700716, -0.7241365927453635720, 0.5953219528653882486 ) ) ;
#38150 = CARTESIAN_POINT ( 'NONE',  ( 0.008896642862326420084, -0.8607682488963684930, 0.3771998872101971489 ) ) ;
#38151 = CARTESIAN_POINT ( 'NONE',  ( 0.1499999999999990508, -0.5230810839623395436, 0.1699593469062158912 ) ) ;
#38152 = EDGE_CURVE ( 'NONE', #23391, #29449, #16776, .T. ) ;
#38153 = CARTESIAN_POINT ( 'NONE',  ( 0.3999999999999783729, -2.097675824466504135, -0.5196396315034577107 ) ) ;
#38154 = EDGE_CURVE ( 'NONE', #13061, #29245, #22083, .T. ) ;
#38155 = CARTESIAN_POINT ( 'NONE',  ( 0.1897112079047663935, -0.5340520988485703002, 0.1436109887884086111 ) ) ;
#38156 = CARTESIAN_POINT ( 'NONE',  ( -0.04945776359514979931, 0.3082555652855902273, -0.3644343153303183369 ) ) ;
#38157 = ADVANCED_FACE ( 'NONE', ( #11904 ), #33674, .T. ) ;
#38158 = DIRECTION ( 'NONE',  ( 0.4999551463232373427, -0.8660512985181134660, 0.000000000000000000 ) ) ;
#38159 = CONICAL_SURFACE ( 'NONE', #33564, 0.1600000000000006140, 1.047197551196598297 ) ;
#38160 = DIRECTION ( 'NONE',  ( 0.4999551463232372317, -0.8660512985181135770, 0.000000000000000000 ) ) ;
#38161 = CARTESIAN_POINT ( 'NONE',  ( 0.4504239474101026652, -1.039103266886249655, 0.7909361398939754872 ) ) ;
#38162 = VECTOR ( 'NONE', #30003, 39.37007874015748143 ) ;
#38163 = CARTESIAN_POINT ( 'NONE',  ( 0.5093734679828535450, -1.177557262684492123, 0.4426697169515769748 ) ) ;
#38164 = CARTESIAN_POINT ( 'NONE',  ( 0.04237657096039100513, -1.193514938088262589, 0.6790371710685850770 ) ) ;
#38165 = CIRCLE ( 'NONE', #20440, 0.4615209409081865166 ) ;
#38166 = CIRCLE ( 'NONE', #17817, 0.1333070866141734534 ) ;
#38167 = DIRECTION ( 'NONE',  ( -1.000000000000000000, -0.000000000000000000, -0.000000000000000000 ) ) ;
#38168 = CARTESIAN_POINT ( 'NONE',  ( 0.4725170613493049898, -1.127650739974109584, -0.3804102490670597247 ) ) ;
#38169 = CARTESIAN_POINT ( 'NONE',  ( 0.3172624056207399290, -1.074258392339833668, 0.7402716440859538061 ) ) ;
#38170 = DIRECTION ( 'NONE',  ( -7.000205099780314469E-17, -1.000000000000000000, 6.590151126658399604E-16 ) ) ;
#38171 = CARTESIAN_POINT ( 'NONE',  ( 0.7052223925351273071, -1.496651798270721478, 0.5101712127052632217 ) ) ;
#38172 = ORIENTED_EDGE ( 'NONE', *, *, #14031, .F. ) ;
#38173 = CARTESIAN_POINT ( 'NONE',  ( -0.2746410161513782033, -2.183180860297908144, -0.4937760292030871079 ) ) ;
#38174 = CARTESIAN_POINT ( 'NONE',  ( 0.5074983293434512932, -1.310930700276065286, 0.7866430700807623966 ) ) ;
#38175 = EDGE_CURVE ( 'NONE', #1496, #15591, #2859, .T. ) ;
#38176 = CARTESIAN_POINT ( 'NONE',  ( 0.5460456802599069626, -1.663806483198842612, -0.4748870211469257141 ) ) ;
#38177 = CARTESIAN_POINT ( 'NONE',  ( -0.02953079040095680369, -0.09152108205201929525, 0.5223162075576431862 ) ) ;
#38178 = EDGE_CURVE ( 'NONE', #24330, #24709, #31575, .T. ) ;
#38179 = VERTEX_POINT ( 'NONE', #35528 ) ;
#38180 = DIRECTION ( 'NONE',  ( 0.8660512985181134660, 0.4999551463232372872, 0.000000000000000000 ) ) ;
#38181 = CARTESIAN_POINT ( 'NONE',  ( 0.1810371303969632861, -0.5115429810441346481, 0.2061669964520652931 ) ) ;
#38182 = CARTESIAN_POINT ( 'NONE',  ( 0.000000000000000000, -0.4578766358967566452, -0.4053162176620347945 ) ) ;
#38183 = FACE_OUTER_BOUND ( 'NONE', #19336, .T. ) ;
#38184 = CARTESIAN_POINT ( 'NONE',  ( 0.4300745628493823358, -1.186155211153737232, 0.6976739215592587806 ) ) ;
#38185 = VECTOR ( 'NONE', #26468, 39.37007874015748854 ) ;
#38187 = CARTESIAN_POINT ( 'NONE',  ( 0.3105521454072050491, -1.758467560521084883, 0.5220235835725158813 ) ) ;
#38186 = CARTESIAN_POINT ( 'NONE',  ( -0.1743922129835733248, -0.5166151207188712791, 0.09999999999999961697 ) ) ;
#38188 = CARTESIAN_POINT ( 'NONE',  ( 0.4925986438152862856, -1.082524672201789828, 0.5763763218629267548 ) ) ;
#38189 = ORIENTED_EDGE ( 'NONE', *, *, #13768, .T. ) ;
#38190 = APPROVAL_STATUS ( 'not_yet_approved' ) ;
#38191 = CIRCLE ( 'NONE', #9940, 0.01999999999999927530 ) ;
#38192 = CARTESIAN_POINT ( 'NONE',  ( 0.03435895639558289583, -1.001604871562542964, 0.6814382083780546884 ) ) ;
#38193 = ORIENTED_EDGE ( 'NONE', *, *, #14239, .F. ) ;
#38194 = CONICAL_SURFACE ( 'NONE', #33575, 0.07499999999999991396, 0.6931599075767558293 ) ;
#38195 =( BOUNDED_SURFACE ( )  B_SPLINE_SURFACE ( 3, 2, ( 
 ( #15919, #340, #3577 ),
 ( #9551, #3782, #16532 ),
 ( #28875, #21911, #34644 ),
 ( #6254, #25404, #31368 ),
 ( #25807, #22127, #25185 ),
 ( #16336, #6444, #38329 ) ),
 .UNSPECIFIED., .F., .F., .T. ) 
 B_SPLINE_SURFACE_WITH_KNOTS ( ( 4, 2, 4 ),
 ( 3, 3 ),
 ( 0.001871265718127418636, 0.003264854125545280095, 0.004658442532963141987 ),
 ( 0.000000000000000000, 1.000000000000000000 ),
 .UNSPECIFIED. ) 
 GEOMETRIC_REPRESENTATION_ITEM ( )  RATIONAL_B_SPLINE_SURFACE ( (
 ( 1.000000000000000000, 0.9912868421517995188, 1.000000000000000000),
 ( 1.000000000000000000, 0.9874999437985944040, 1.000000000000000000),
 ( 1.000000000000000000, 0.9809055010152987197, 1.000000000000000000),
 ( 1.000000000000000000, 0.9631198196773240738, 1.000000000000000000),
 ( 1.000000000000000000, 0.9523038229114263453, 1.000000000000000000),
 ( 1.000000000000000000, 0.9405852554627024409, 1.000000000000000000) ) ) 
 REPRESENTATION_ITEM ( '' )  SURFACE ( )  );
#38196 = CARTESIAN_POINT ( 'NONE',  ( 0.3853488629557857981, -1.605649824104631307, 0.5756816568910164689 ) ) ;
#38198 = CARTESIAN_POINT ( 'NONE',  ( 0.1988841153628475300, -0.6078592671934165415, 0.3205631666503918620 ) ) ;
#38197 = CARTESIAN_POINT ( 'NONE',  ( 0.08691621476508532007, -0.7276673773931944256, 0.02918323030706625534 ) ) ;
#38199 = CARTESIAN_POINT ( 'NONE',  ( 0.3398694799145297596, -1.651829322229799057, -0.3839951212973800598 ) ) ;
#38200 = VECTOR ( 'NONE', #22415, 39.37007874015748143 ) ;
#38201 = ORIENTED_EDGE ( 'NONE', *, *, #16465, .F. ) ;
#38202 = AXIS2_PLACEMENT_3D ( 'NONE', #9387, #3630, #3419 ) ;
#38203 = EDGE_LOOP ( 'NONE', ( #28985, #28085, #20671, #25504 ) ) ;
#38204 = ORIENTED_EDGE ( 'NONE', *, *, #17479, .T. ) ;
#38205 = DIRECTION ( 'NONE',  ( -1.000000000000000000, -7.857794173099924470E-32, -8.628166150854818811E-32 ) ) ;
#38206 = CARTESIAN_POINT ( 'NONE',  ( 0.1307094081766367877, -0.6333278402568883747, 0.3902961089287821927 ) ) ;
#38207 = ORIENTED_EDGE ( 'NONE', *, *, #2257, .T. ) ;
#38208 = CARTESIAN_POINT ( 'NONE',  ( 0.3855953621615598736, -1.879051724042604121, -0.5131335247813605394 ) ) ;
#38209 = DIRECTION ( 'NONE',  ( 0.000000000000000000, 0.000000000000000000, -1.000000000000000000 ) ) ;
#38210 = DIRECTION ( 'NONE',  ( -0.000000000000000000, 0.3807313408632030383, 0.9246857012436753287 ) ) ;
#38211 = CARTESIAN_POINT ( 'NONE',  ( -1.019575837292303166, -0.04310840302197994911, 0.3599999999999993205 ) ) ;
#38212 = CARTESIAN_POINT ( 'NONE',  ( 0.1757972024313168569, -1.554466423739661707, -0.3564840659511942511 ) ) ;
#38213 = CARTESIAN_POINT ( 'NONE',  ( 0.7409681548321257472, -1.515722218252784748, 0.5271419462256154986 ) ) ;
#38214 = CARTESIAN_POINT ( 'NONE',  ( 0.1984327864668515018, -2.037394601422313212, -0.7106754852713771387 ) ) ;
#38215 = CARTESIAN_POINT ( 'NONE',  ( -0.02000000000000000042, -1.614234636154356251, 0.1774087976708900172 ) ) ;
#38216 = LINE ( 'NONE', #3861, #863 ) ;
#38217 = DATE_AND_TIME ( #8320, #27932 ) ;
#38218 = AXIS2_PLACEMENT_3D ( 'NONE', #21221, #18131, #17710 ) ;
#38219 = CARTESIAN_POINT ( 'NONE',  ( 0.3297668774377428558, -1.165569269438828215, 0.4615993935216395894 ) ) ;
#38220 = CARTESIAN_POINT ( 'NONE',  ( 0.6565177652365870031, -1.363219716956428407, 0.8083140950016142190 ) ) ;
#38221 = CARTESIAN_POINT ( 'NONE',  ( 0.6960413307267936389, -1.427205786779416785, 0.4634944759858370955 ) ) ;
#38222 = CARTESIAN_POINT ( 'NONE',  ( 0.2644966038856382817, -1.687071023141420545, 0.5682417262808783232 ) ) ;
#38223 = CIRCLE ( 'NONE', #38861, 0.08769881541126034463 ) ;
#38224 = AXIS2_PLACEMENT_3D ( 'NONE', #19569, #32288, #3909 ) ;
#38225 = CARTESIAN_POINT ( 'NONE',  ( 0.1835308262027276760, -1.352961526709849149, 0.9396307682827382823 ) ) ;
#38226 = CARTESIAN_POINT ( 'NONE',  ( 0.0001527010945176735684, -0.5560399355413865319, -0.06596982925828048794 ) ) ;
#38227 = CARTESIAN_POINT ( 'NONE',  ( 0.4265385717645384100, -1.610299123943391919, -0.3658380804397534103 ) ) ;
#38228 = CARTESIAN_POINT ( 'NONE',  ( 0.3509251431255968057, -1.165375537921118143, 0.4182417262808918457 ) ) ;
#38229 = VERTEX_POINT ( 'NONE', #16619 ) ;
#38230 = ORIENTED_EDGE ( 'NONE', *, *, #19620, .F. ) ;
#38231 = FACE_OUTER_BOUND ( 'NONE', #5542, .T. ) ;
#38232 = ORIENTED_EDGE ( 'NONE', *, *, #5740, .T. ) ;
#38233 = FACE_OUTER_BOUND ( 'NONE', #33481, .T. ) ;
#38234 = CARTESIAN_POINT ( 'NONE',  ( -0.2399999999999999079, -2.511040369707300268, -0.4948468226404901804 ) ) ;
#38235 = CARTESIAN_POINT ( 'NONE',  ( 0.4980693604982071032, -1.296659755426072147, 0.8022866093385110364 ) ) ;
#38237 = ORIENTED_EDGE ( 'NONE', *, *, #2997, .F. ) ;
#38236 = CARTESIAN_POINT ( 'NONE',  ( -2.070754768975505034, -0.09959325338431362917, 0.3749999999999976130 ) ) ;
#38238 = ORIENTED_EDGE ( 'NONE', *, *, #1734, .T. ) ;
#38239 = CARTESIAN_POINT ( 'NONE',  ( 0.5558873460704856218, -1.622947742269525095, 0.5440989928495453265 ) ) ;
#38240 = ORIENTED_EDGE ( 'NONE', *, *, #13288, .T. ) ;
#38241 = CARTESIAN_POINT ( 'NONE',  ( 0.2968959581392767166, -1.656557492789272779, 0.5695608020044338193 ) ) ;
#38243 = CARTESIAN_POINT ( 'NONE',  ( 0.2034275709668185161, -1.278716077829719300, -0.3194722003129935040 ) ) ;
#38242 = CARTESIAN_POINT ( 'NONE',  ( 0.6468566800937594063, -1.553424414166365564, 0.4209516853548616599 ) ) ;
#38244 = CARTESIAN_POINT ( 'NONE',  ( -0.2746410161513779258, -3.609310082097819894, -0.4498340178114252352 ) ) ;
#38245 = CARTESIAN_POINT ( 'NONE',  ( 0.1837169918685102876, -0.8266995537623093027, 0.1015045423513593059 ) ) ;
#38246 = VECTOR ( 'NONE', #15135, 39.37007874015748143 ) ;
#38247 = CARTESIAN_POINT ( 'NONE',  ( -7.749463158931491936E-06, -2.054538870594384115, -0.2740520340402112232 ) ) ;
#38249 = VERTEX_POINT ( 'NONE', #32444 ) ;
#38248 = ORIENTED_EDGE ( 'NONE', *, *, #1498, .F. ) ;
#38250 = DIRECTION ( 'NONE',  ( 1.000000000000000000, 0.000000000000000000, 0.000000000000000000 ) ) ;
#38251 = CARTESIAN_POINT ( 'NONE',  ( 0.1454380568973649701, -0.9477385833960229045, 0.4092464228063885101 ) ) ;
#38252 = PERSON ( 'NAUO-PER7', 'UNSPECIFIED', 'UNSPECIFIED', ('UNSPECIFIED'), ('UNSPECIFIED'), ('UNSPECIFIED') ) ;
#38253 = CARTESIAN_POINT ( 'NONE',  ( -0.04285561529641037509, -0.4433460678679742029, 0.2197428102801966265 ) ) ;
#38254 = CARTESIAN_POINT ( 'NONE',  ( 0.5706732878214085813, -1.412446763865061294, 0.7287409280026274638 ) ) ;
#38255 = VECTOR ( 'NONE', #16270, 39.37007874015748854 ) ;
#38256 = VECTOR ( 'NONE', #15907, 39.37007874015748143 ) ;
#38257 = CARTESIAN_POINT ( 'NONE',  ( 0.1351628486807437135, -0.8647813875850353105, 0.4853538377376631630 ) ) ;
#38258 = DIRECTION ( 'NONE',  ( 8.881784197001246407E-16, -2.361472542561082612E-16, 1.000000000000000000 ) ) ;
#38259 = AXIS2_PLACEMENT_3D ( 'NONE', #32167, #31972, #16150 ) ;
#38260 = CARTESIAN_POINT ( 'NONE',  ( 0.01548846960707524721, 0.000000000000000000, 0.000000000000000000 ) ) ;
#38261 = CARTESIAN_POINT ( 'NONE',  ( 0.3223215012880607522, -1.527613999045389415, -0.7370652326885508421 ) ) ;
#38262 = CARTESIAN_POINT ( 'NONE',  ( 0.6465835049539362389, -1.539613817736340318, 0.4182417262808776903 ) ) ;
#38263 = CARTESIAN_POINT ( 'NONE',  ( 0.3174184176267951796, -1.762933076790987874, 0.5319023928053561168 ) ) ;
#38264 = DIRECTION ( 'NONE',  ( 1.000000000000000000, 0.000000000000000000, 0.000000000000000000 ) ) ;
#38265 = CARTESIAN_POINT ( 'NONE',  ( 0.05279905671744906936, -0.3065870127357976926, 0.3541429396893026049 ) ) ;
#38266 = CARTESIAN_POINT ( 'NONE',  ( 0.2292082634166116850, -1.390808673668628259, 1.038138609612698327 ) ) ;
#38267 = CARTESIAN_POINT ( 'NONE',  ( 0.2927350798623002959, -1.544518291098198715, -0.6925464747855896164 ) ) ;
#38268 = PERSON_AND_ORGANIZATION_ROLE ( 'design_owner' ) ;
#38269 = CYLINDRICAL_SURFACE ( 'NONE', #26494, 0.06000000000000021289 ) ;
#38270 = CARTESIAN_POINT ( 'NONE',  ( 0.2927350798622761485, -1.544518291098210261, -0.6925464747855858416 ) ) ;
#38271 = AXIS2_PLACEMENT_3D ( 'NONE', #27415, #39938, #9476 ) ;
#38272 = CARTESIAN_POINT ( 'NONE',  ( -0.04946426091937417696, 0.4635716124040153985, 0.1136627969334571137 ) ) ;
#38273 = PLANE ( 'NONE',  #14257 ) ;
#38274 = CIRCLE ( 'NONE', #13325, 0.03000000000000022787 ) ;
#38275 = CIRCLE ( 'NONE', #25167, 0.07499999999999977518 ) ;
#38276 = VERTEX_POINT ( 'NONE', #4461 ) ;
#38277 = CARTESIAN_POINT ( 'NONE',  ( 0.4009272606926310711, -1.137264901707352172, 0.4308458577267786915 ) ) ;
#38278 = VERTEX_POINT ( 'NONE', #38023 ) ;
#38279 = CARTESIAN_POINT ( 'NONE',  ( 0.4720092934469595769, -1.159105807646246600, -0.4122610257295769576 ) ) ;
#38280 = APPLIED_PERSON_AND_ORGANIZATION_ASSIGNMENT ( #6317, #15595, ( #39358 ) ) ;
#38281 = DIRECTION ( 'NONE',  ( -0.000000000000000000, -0.7071067811865474617, -0.7071067811865474617 ) ) ;
#38282 = CARTESIAN_POINT ( 'NONE',  ( 0.5957392760757502792, -1.486251830005147712, 0.6051716374586044722 ) ) ;
#38284 = ORIENTED_EDGE ( 'NONE', *, *, #38099, .T. ) ;
#38283 = DIRECTION ( 'NONE',  ( 1.654489825136719548E-31, -0.9510565162951568619, -0.3090169943749375703 ) ) ;
#38286 = ORIENTED_EDGE ( 'NONE', *, *, #26778, .T. ) ;
#38285 = ORIENTED_EDGE ( 'NONE', *, *, #8618, .F. ) ;
#38287 = DIRECTION ( 'NONE',  ( 0.000000000000000000, 0.000000000000000000, 1.000000000000000000 ) ) ;
#38288 = ORIENTED_EDGE ( 'NONE', *, *, #21313, .F. ) ;
#38289 = AXIS2_PLACEMENT_3D ( 'NONE', #13533, #6940, #3456 ) ;
#38290 = FACE_OUTER_BOUND ( 'NONE', #10114, .T. ) ;
#38291 = PERSON_AND_ORGANIZATION ( #61, #5652 ) ;
#38292 = CARTESIAN_POINT ( 'NONE',  ( -2.112273405726188513E-14, -2.107936428766272741, -0.2870436526301873847 ) ) ;
#38293 = ORIENTED_EDGE ( 'NONE', *, *, #23537, .F. ) ;
#38294 = CARTESIAN_POINT ( 'NONE',  ( 0.08584567903155949919, -0.7460567843300386359, 0.1584740188193046739 ) ) ;
#38295 = CARTESIAN_POINT ( 'NONE',  ( 0.08990536851188075940, -0.5646295468557095409, 0.1389823447417319335 ) ) ;
#38296 = CARTESIAN_POINT ( 'NONE',  ( 0.1100377367245384957, -0.5478698975639066937, 0.1620895514292355621 ) ) ;
#38297 = EDGE_CURVE ( 'NONE', #17796, #28034, #6955, .T. ) ;
#38298 = CARTESIAN_POINT ( 'NONE',  ( 0.6434205324370606549, -1.429852958019900200, -0.6292195679946139819 ) ) ;
#38299 = FACE_OUTER_BOUND ( 'NONE', #29490, .T. ) ;
#38300 = CARTESIAN_POINT ( 'NONE',  ( -0.05634304521267748805, 1.092739197465705287E-15, 0.4588823192046724841 ) ) ;
#38301 = CIRCLE ( 'NONE', #8722, 0.04249999999999994754 ) ;
#38302 = DIRECTION ( 'NONE',  ( 0.000000000000000000, 0.000000000000000000, -1.000000000000000000 ) ) ;
#38303 = CARTESIAN_POINT ( 'NONE',  ( 0.7432279256316001170, -1.516441678994711051, 0.5660936748573839328 ) ) ;
#38304 = CARTESIAN_POINT ( 'NONE',  ( 0.1759300380180284507, -1.231083256582695684, -0.4125659523519146221 ) ) ;
#38305 = EDGE_CURVE ( 'NONE', #9503, #8761, #26686, .T. ) ;
#38306 = CIRCLE ( 'NONE', #23246, 0.1033070866141732325 ) ;
#38307 = CARTESIAN_POINT ( 'NONE',  ( 0.2044722610693382459, -0.7754815171928667317, 0.5837216336432284880 ) ) ;
#38308 = VECTOR ( 'NONE', #30187, 39.37007874015748143 ) ;
#38309 = DIRECTION ( 'NONE',  ( 7.771561172376107616E-16, -7.170354002788761615E-17, 1.000000000000000000 ) ) ;
#38310 = EDGE_CURVE ( 'NONE', #4385, #28969, #32234, .T. ) ;
#38311 = CARTESIAN_POINT ( 'NONE',  ( 0.3208715077212234701, -1.182672892261233732, 0.4687417262808780127 ) ) ;
#38312 = EDGE_CURVE ( 'NONE', #1588, #15168, #23207, .T. ) ;
#38313 = DIMENSIONAL_EXPONENTS ( 1.000000000000000000, 0.000000000000000000, 0.000000000000000000, 0.000000000000000000, 0.000000000000000000, 0.000000000000000000, 0.000000000000000000 ) ;
#38314 = CARTESIAN_POINT ( 'NONE',  ( 0.4567835194390648113, -1.106698506970852147, -0.3756906124113179035 ) ) ;
#38315 = EDGE_CURVE ( 'NONE', #1394, #13751, #36397, .T. ) ;
#38316 = CARTESIAN_POINT ( 'NONE',  ( 0.08042334443895514384, -1.362032735465325661, 0.6028738014108521170 ) ) ;
#38317 = AXIS2_PLACEMENT_3D ( 'NONE', #35394, #35202, #19572 ) ;
#38318 = CARTESIAN_POINT ( 'NONE',  ( 0.5078487756305317680, -1.109832367716456325, 0.6054007957810670915 ) ) ;
#38319 = COORDINATED_UNIVERSAL_TIME_OFFSET ( 0, 0, .AHEAD. ) ;
#38320 = LINE ( 'NONE', #16522, #38526 ) ;
#38321 = DIRECTION ( 'NONE',  ( 0.000000000000000000, 0.000000000000000000, 1.000000000000000000 ) ) ;
#38322 = CARTESIAN_POINT ( 'NONE',  ( 0.4688957988796484400, -1.165393138958765729, 0.4182417262808778013 ) ) ;
#38323 = EDGE_CURVE ( 'NONE', #17036, #22774, #18125, .T. ) ;
#38324 = EDGE_LOOP ( 'NONE', ( #8943, #31471, #10165, #7362 ) ) ;
#38325 = CARTESIAN_POINT ( 'NONE',  ( 0.05999999999999990757, -0.3458405862425447119, -0.2552451372150014719 ) ) ;
#38326 = APPLIED_DATE_AND_TIME_ASSIGNMENT ( #3911, #22878, ( #2940 ) ) ;
#38327 = CARTESIAN_POINT ( 'NONE',  ( 0.01055999354154976179, -0.5296565605740110039, 0.1431176680404075141 ) ) ;
#38328 = TOROIDAL_SURFACE ( 'NONE', #39011, 0.08830708661417342731, 0.01499999999999999944 ) ;
#38329 = CARTESIAN_POINT ( 'NONE',  ( 0.1927077495703349297, -0.8180328145591141409, 0.2791508387892265297 ) ) ;
#38330 = ORIENTED_EDGE ( 'NONE', *, *, #26399, .F. ) ;
#38331 = DIRECTION ( 'NONE',  ( 0.000000000000000000, 0.000000000000000000, -1.000000000000000000 ) ) ;
#38332 = CARTESIAN_POINT ( 'NONE',  ( 0.1969702849860160421, -0.5469408226469265610, 0.3272831088336244365 ) ) ;
#38334 = VERTEX_POINT ( 'NONE', #34932 ) ;
#38333 = ORIENTED_EDGE ( 'NONE', *, *, #17301, .T. ) ;
#38335 = DIRECTION ( 'NONE',  ( -0.007367783058131798131, -0.4999457213560382085, 0.8660253988599866393 ) ) ;
#38336 = CONICAL_SURFACE ( 'NONE', #12070, 0.1400000000000007627, 1.047197551196601406 ) ;
#38337 = AXIS2_PLACEMENT_3D ( 'NONE', #34502, #14974, #30808 ) ;
#38338 = PLANE ( 'NONE',  #14479 ) ;
#38339 = FACE_OUTER_BOUND ( 'NONE', #7623, .T. ) ;
#38340 = CARTESIAN_POINT ( 'NONE',  ( 0.02242828275838944924, -0.2417645306140268069, -0.4517153736362903849 ) ) ;
#38341 = ORIENTED_EDGE ( 'NONE', *, *, #24992, .T. ) ;
#38342 = CARTESIAN_POINT ( 'NONE',  ( 0.008458849636713906481, -0.6664941812440515756, -0.01118885721624096607 ) ) ;
#38343 = CARTESIAN_POINT ( 'NONE',  ( 0.09450633965359066246, -0.6214005085407516837, 0.2730725926996435127 ) ) ;
#38344 = CARTESIAN_POINT ( 'NONE',  ( 0.4640678500019702057, -1.188919783037170275, 0.5182417262812423209 ) ) ;
#38345 = CARTESIAN_POINT ( 'NONE',  ( 0.1277384056562314574, -0.7278354053324652684, 0.5494589346582330336 ) ) ;
#38347 = CARTESIAN_POINT ( 'NONE',  ( 0.1499999999999993561, 1.639108796198557931E-15, -0.5500000000000003775 ) ) ;
#38346 = CARTESIAN_POINT ( 'NONE',  ( 0.002290818369124609372, -0.5198888459286679087, 0.1457185332388686583 ) ) ;
#38348 = CARTESIAN_POINT ( 'NONE',  ( 0.06709112777885012369, -1.107863570390577479, 0.7528161107794053564 ) ) ;
#38349 = CARTESIAN_POINT ( 'NONE',  ( 0.3938498138106606428, -1.064849829384627800, 0.6374776580343812782 ) ) ;
#38350 = ORIENTED_EDGE ( 'NONE', *, *, #39190, .T. ) ;
#38351 = ORIENTED_EDGE ( 'NONE', *, *, #10988, .F. ) ;
#38352 = CARTESIAN_POINT ( 'NONE',  ( 0.3827397780245204162, -1.608088820898147864, 0.5231971522552248954 ) ) ;
#38353 = CARTESIAN_POINT ( 'NONE',  ( 0.1887413233215596287, -0.4595325217136330131, 0.1463014889510880212 ) ) ;
#38354 = CARTESIAN_POINT ( 'NONE',  ( -0.03642997641689344618, 0.3645929376994324067, -0.3593586258117690835 ) ) ;
#38355 = ADVANCED_FACE ( 'NONE', ( #35344 ), #7135, .F. ) ;
#38356 = LINE ( 'NONE', #3998, #21219 ) ;
#38357 = TOROIDAL_SURFACE ( 'NONE', #24579, 0.5250000000000000222, 0.01499999999999999944 ) ;
#38358 = EDGE_CURVE ( 'NONE', #36494, #8537, #35857, .T. ) ;
#38359 = CARTESIAN_POINT ( 'NONE',  ( 0.5022839945508311699, -1.192782407697791980, 0.4224083929475445642 ) ) ;
#38360 = EDGE_CURVE ( 'NONE', #20037, #7253, #10041, .T. ) ;
#38361 = CARTESIAN_POINT ( 'NONE',  ( 0.6761418372287171241, -1.395094899906518471, 0.6557117145240808354 ) ) ;
#38362 = VECTOR ( 'NONE', #13877, 39.37007874015748143 ) ;
#38363 = CONICAL_SURFACE ( 'NONE', #33797, 0.5399999999999999245, 1.211529128687673262 ) ;
#38364 = CARTESIAN_POINT ( 'NONE',  ( -0.02000000000000000042, -1.910390638264138685, -0.7420407338378623985 ) ) ;
#38365 = CARTESIAN_POINT ( 'NONE',  ( 0.01888917602804259660, -1.051501505208036313, 0.6153358008999590956 ) ) ;
#38366 = CARTESIAN_POINT ( 'NONE',  ( 0.04285640132274042002, 0.4433417433457765289, -0.2197472875419943517 ) ) ;
#38367 = CARTESIAN_POINT ( 'NONE',  ( 0.5353561135554193440, -1.635566321744903906, -0.5401600205605631144 ) ) ;
#38368 = ORIENTED_EDGE ( 'NONE', *, *, #3141, .F. ) ;
#38369 = CARTESIAN_POINT ( 'NONE',  ( 0.3291361082742700339, -1.091304683942979858, 0.7409066756199927939 ) ) ;
#38370 = CARTESIAN_POINT ( 'NONE',  ( 0.01895494625228206706, -0.07381100255646662334, 0.5147985126481147145 ) ) ;
#38371 = CIRCLE ( 'NONE', #37704, 0.05330708661417339622 ) ;
#38372 = DIRECTION ( 'NONE',  ( -0.4999551463232377313, 0.8660512985181132439, -0.000000000000000000 ) ) ;
#38373 = VECTOR ( 'NONE', #25683, 39.37007874015748854 ) ;
#38374 = EDGE_CURVE ( 'NONE', #33923, #10991, #23413, .T. ) ;
#38375 = VERTEX_POINT ( 'NONE', #1029 ) ;
#38376 = DIRECTION ( 'NONE',  ( 0.8660254037844395958, -0.2456612931291811963, -0.4354888391889014110 ) ) ;
#38377 = CARTESIAN_POINT ( 'NONE',  ( 0.5448400828272464969, -1.370358474244389502, 0.7639071756578307282 ) ) ;
#38378 = CARTESIAN_POINT ( 'NONE',  ( 0.6498387395261646660, -1.464631408770378673, 0.4182417262808778013 ) ) ;
#38379 = LINE ( 'NONE', #22783, #16710 ) ;
#38380 = ORIENTED_EDGE ( 'NONE', *, *, #8679, .F. ) ;
#38381 = CARTESIAN_POINT ( 'NONE',  ( -0.02000000000000000042, -2.071870001606465284, -0.3441689154348898105 ) ) ;
#38382 = CARTESIAN_POINT ( 'NONE',  ( 0.2231482617632921661, -1.353434846386320611, 0.5181482079951671427 ) ) ;
#38383 = CARTESIAN_POINT ( 'NONE',  ( 0.4778170654558047126, -1.668016138613298560, 0.5682417262808788783 ) ) ;
#38384 = LINE ( 'NONE', #16805, #5491 ) ;
#38385 = AXIS2_PLACEMENT_3D ( 'NONE', #21664, #6219, #11785 ) ;
#38386 = CARTESIAN_POINT ( 'NONE',  ( 0.4900744151468222065, -1.275953078071682789, 0.5997076496587170347 ) ) ;
#38388 = DIRECTION ( 'NONE',  ( -0.5000000000000001110, 4.252453317207020267E-31, 0.8660254037844385966 ) ) ;
#38387 = DIRECTION ( 'NONE',  ( 1.000000000000000000, 2.549619951388193009E-12, -4.473262954207831680E-13 ) ) ;
#38389 = CARTESIAN_POINT ( 'NONE',  ( 0.3238203105384647174, -0.9899218032796638367, 0.5856430185708639824 ) ) ;
#38390 = ORIENTED_EDGE ( 'NONE', *, *, #14499, .T. ) ;
#38392 = AXIS2_PLACEMENT_3D ( 'NONE', #3847, #16221, #6524 ) ;
#38391 = ITEM_DEFINED_TRANSFORMATION ( 'NONE', 'NONE', #27908,  #27819 ) ;
#38393 = CARTESIAN_POINT ( 'NONE',  ( 0.05668208346063462189, -1.107411393821966072, 0.7455345429973143645 ) ) ;
#38394 = VERTEX_POINT ( 'NONE', #4267 ) ;
#38395 = CIRCLE ( 'NONE', #31196, 0.01499999999999994567 ) ;
#38396 = VERTEX_POINT ( 'NONE', #28770 ) ;
#38397 = CIRCLE ( 'NONE', #32493, 2.001674066779347783 ) ;
#38398 = CARTESIAN_POINT ( 'NONE',  ( 0.4133974373207104369, -1.589464046522193419, 0.5703553845707169945 ) ) ;
#38400 = CARTESIAN_POINT ( 'NONE',  ( 0.2012013697609311147, -0.6235265729459525952, 0.3370440851636130053 ) ) ;
#38399 = CARTESIAN_POINT ( 'NONE',  ( 0.06591376428800177489, -0.7622139198468362853, 0.01798093938639453923 ) ) ;
#38401 = CARTESIAN_POINT ( 'NONE',  ( 0.1987142792575499195, -2.031216512937317642, -0.3109074494126257138 ) ) ;
#38402 = LOCAL_TIME ( 0, 53, 7.000000000000000000, #16621 ) ;
#38403 = VERTEX_POINT ( 'NONE', #629 ) ;
#38404 = CARTESIAN_POINT ( 'NONE',  ( 0.4155048779794340841, -1.128001391588047353, 0.5745684004788098598 ) ) ;
#38405 = CARTESIAN_POINT ( 'NONE',  ( 0.4522227720718606792, -1.319557941469291729, 0.8277251512335837003 ) ) ;
#38406 = VERTEX_POINT ( 'NONE', #26109 ) ;
#38407 = AXIS2_PLACEMENT_3D ( 'NONE', #27642, #2351, #27451 ) ;
#38408 = CARTESIAN_POINT ( 'NONE',  ( 0.1874572521746671327, -0.6893911860354969834, 0.06179796301327929176 ) ) ;
#38409 = CARTESIAN_POINT ( 'NONE',  ( 0.08471508035845262685, -1.662502673085205496, -0.3682490140513268728 ) ) ;
#38410 = B_SPLINE_CURVE_WITH_KNOTS ( 'NONE', 3,
 ( #34428, #28071, #12227, #34215, #8713, #30542 ),
 .UNSPECIFIED., .F., .F.,
 ( 4, 2, 4 ),
 ( -7.819781547275446803E-06, 0.0005992764336422149504, 0.001206372648831705204 ),
 .UNSPECIFIED. ) ;
#38411 = DIRECTION ( 'NONE',  ( 0.4999551463232372317, -0.8660512985181135770, 0.000000000000000000 ) ) ;
#38412 = DIRECTION ( 'NONE',  ( 0.4999551463232369541, -0.8660512985181135770, 8.034847040189003318E-16 ) ) ;
#38413 = EDGE_CURVE ( 'NONE', #38795, #34243, #20127, .T. ) ;
#38414 = CARTESIAN_POINT ( 'NONE',  ( 0.4158404862163792015, -1.704211426646492944, 0.6192745419747571756 ) ) ;
#38415 = B_SPLINE_CURVE_WITH_KNOTS ( 'NONE', 3,
 ( #35689, #23377, #32792, #29935 ),
 .UNSPECIFIED., .F., .F.,
 ( 4, 4 ),
 ( 0.000000000000000000, 0.1653597904024633469 ),
 .UNSPECIFIED. ) ;
#38416 = CARTESIAN_POINT ( 'NONE',  ( 0.08511258892558128120, -0.8122055842375904833, 0.1451433120779370700 ) ) ;
#38417 = CARTESIAN_POINT ( 'NONE',  ( 0.4676789493019616883, -1.559177855287317005, 0.5735223705611400824 ) ) ;
#38418 = CARTESIAN_POINT ( 'NONE',  ( 0.3873588152119425976, -1.881242926337077348, -0.4864542591168500296 ) ) ;
#38419 = CARTESIAN_POINT ( 'NONE',  ( 0.3207732826076518662, -1.759136744920719808, 0.5682417262808786562 ) ) ;
#38420 = DIRECTION ( 'NONE',  ( 0.000000000000000000, 0.000000000000000000, -1.000000000000000000 ) ) ;
#38421 = APPROVAL_STATUS ( 'not_yet_approved' ) ;
#38422 = AXIS2_PLACEMENT_3D ( 'NONE', #2292, #34354, #6168 ) ;
#38423 = CARTESIAN_POINT ( 'NONE',  ( 0.6453025834024398444, -1.483340485508765738, -0.6195432661420555709 ) ) ;
#38424 = AXIS2_PLACEMENT_3D ( 'NONE', #38969, #20458, #39186 ) ;
#38425 = DIRECTION ( 'NONE',  ( 1.000000000000000000, 0.000000000000000000, 0.000000000000000000 ) ) ;
#38426 = CARTESIAN_POINT ( 'NONE',  ( 0.1846093570424984787, -0.6365630712797759605, -0.02370498549722033915 ) ) ;
#38427 = CARTESIAN_POINT ( 'NONE',  ( 0.2592104087477605789, -1.679801881415013964, 0.6057417262800831592 ) ) ;
#38428 = CARTESIAN_POINT ( 'NONE',  ( -0.1743922129835736579, -0.5166151207188712791, 0.1000000000000000194 ) ) ;
#38429 = AXIS2_PLACEMENT_3D ( 'NONE', #16985, #4606, #33614 ) ;
#38430 = APPLIED_APPROVAL_ASSIGNMENT ( #29513, ( #19425 ) ) ;
#38431 = CARTESIAN_POINT ( 'NONE',  ( 0.2039603895705197623, -1.429414345016513765, 0.9236325154956378514 ) ) ;
#38432 = CARTESIAN_POINT ( 'NONE',  ( -0.0004431470427073231017, -0.9367128829938298207, 0.1457185332388704069 ) ) ;
#38433 = EDGE_CURVE ( 'NONE', #25698, #10115, #22760, .T. ) ;
#38434 = CARTESIAN_POINT ( 'NONE',  ( 0.000000000000000000, 0.000000000000000000, 0.000000000000000000 ) ) ;
#38435 = APPLIED_DATE_AND_TIME_ASSIGNMENT ( #23089, #29649, ( #24771 ) ) ;
#38436 = CARTESIAN_POINT ( 'NONE',  ( 0.5431716904107454225, -1.629634126750506340, -0.5863231643301370921 ) ) ;
#38437 = CARTESIAN_POINT ( 'NONE',  ( -0.05464101615137770263, -2.589364949149576933, -0.2950346662398796171 ) ) ;
#38438 = EDGE_CURVE ( 'NONE', #30555, #25449, #11580, .T. ) ;
#38439 = APPLICATION_CONTEXT ( 'configuration controlled 3d designs of mechanical parts and assemblies' ) ;
#38440 = VECTOR ( 'NONE', #14632, 39.37007874015748854 ) ;
#38441 = ORIENTED_EDGE ( 'NONE', *, *, #31414, .F. ) ;
#38442 = VERTEX_POINT ( 'NONE', #10641 ) ;
#38443 =( BOUNDED_SURFACE ( )  B_SPLINE_SURFACE ( 3, 2, ( 
 ( #36285, #22403, #5022 ),
 ( #20464, #8103, #1353 ),
 ( #16777, #1960, #23381 ),
 ( #36091, #26235, #29516 ) ),
 .UNSPECIFIED., .F., .F., .T. ) 
 B_SPLINE_SURFACE_WITH_KNOTS ( ( 4, 4 ),
 ( 3, 3 ),
 ( 0.007078665261326035942, 0.008688923783415654703 ),
 ( 0.000000000000000000, 1.000000000000000000 ),
 .UNSPECIFIED. ) 
 GEOMETRIC_REPRESENTATION_ITEM ( )  RATIONAL_B_SPLINE_SURFACE ( (
 ( 1.000000000000000000, 0.7038424801053242419, 1.000000000000000000),
 ( 1.000000000000000000, 0.7026662720910222815, 1.000000000000000000),
 ( 1.000000000000000000, 0.7015046397803297307, 1.000000000000000000),
 ( 1.000000000000000000, 0.7003330442032725811, 1.000000000000000000) ) ) 
 REPRESENTATION_ITEM ( '' )  SURFACE ( )  );
#38444 = CARTESIAN_POINT ( 'NONE',  ( -0.1157923916715200702, -0.5295015842444287246, 0.3181161673586325178 ) ) ;
#38445 = ORIENTED_EDGE ( 'NONE', *, *, #19710, .T. ) ;
#38446 = DIRECTION ( 'NONE',  ( 0.4999999999999988898, -0.8285110189370871181, -0.2521299099667287935 ) ) ;
#38447 = CARTESIAN_POINT ( 'NONE',  ( 0.5905148994843929522, -1.592503337285391174, -0.4381592367070794580 ) ) ;
#38448 = CARTESIAN_POINT ( 'NONE',  ( 0.5632287240488592639, -1.399421096049667579, 0.6902502155986122157 ) ) ;
#38450 = ORIENTED_EDGE ( 'NONE', *, *, #35863, .T. ) ;
#38449 = CARTESIAN_POINT ( 'NONE',  ( 0.5841409287570923370, -1.616576648741850253, 0.4600417456556253892 ) ) ;
#38451 = CARTESIAN_POINT ( 'NONE',  ( 0.5520143099787153673, -1.183365530476261585, 0.6129298035784942478 ) ) ;
#38452 = CARTESIAN_POINT ( 'NONE',  ( 0.03309060444528763578, 0.4608881774262347242, -0.2425132784556410515 ) ) ;
#38453 = ORIENTED_EDGE ( 'NONE', *, *, #29904, .F. ) ;
#38454 = CARTESIAN_POINT ( 'NONE',  ( 0.5538245623271985663, -1.622806740292896510, 0.5052194400116507556 ) ) ;
#38455 = ORIENTED_EDGE ( 'NONE', *, *, #16976, .T. ) ;
#38456 = CARTESIAN_POINT ( 'NONE',  ( 0.09652487719191069071, -0.9245692721911921153, 0.7742711943059148449 ) ) ;
#38458 = CARTESIAN_POINT ( 'NONE',  ( 0.1111680786003024363, -0.9208225436044804590, 0.08298286711937687132 ) ) ;
#38457 = DIRECTION ( 'NONE',  ( -1.000000000000000000, -0.000000000000000000, -0.000000000000000000 ) ) ;
#38459 = FACE_OUTER_BOUND ( 'NONE', #34906, .T. ) ;
#38460 = DIRECTION ( 'NONE',  ( -0.4999999999999974465, 0.7980870686147877313, 0.3362395439413060072 ) ) ;
#38461 = VECTOR ( 'NONE', #24260, 39.37007874015748143 ) ;
#38462 = CARTESIAN_POINT ( 'NONE',  ( 0.001120871055943682042, -1.921117088193987188, -0.3378957227562057741 ) ) ;
#38463 = ORIENTED_EDGE ( 'NONE', *, *, #36894, .T. ) ;
#38464 = B_SPLINE_CURVE_WITH_KNOTS ( 'NONE', 3,
 ( #40106, #6166, #5761, #37031, #34754, #31475, #5955, #22240, #15030, #34352, #12351, #25100, #24713, #18515, #24499, #40531, #34563, #15441, #8851, #27580, #9060, #6372, #3282, #9671, #18940, #30861, #31070, #6561, #21430, #37244, #37856, #30671, #18729, #2490, #15837, #24909, #31286, #40321, #2890, #11934, #25316, #33961, #18319, #21622 ),
 .UNSPECIFIED., .F., .F.,
 ( 4, 2, 2, 2, 2, 2, 2, 2, 2, 2, 2, 2, 2, 2, 2, 2, 2, 2, 2, 2, 2, 4 ),
 ( 4.382894615908098410E-08, 0.0008319673269041918387, 0.001663890824862219444, 0.002495814322820246942, 0.003327737820778274656, 0.004159661318736302370, 0.004991584816694329650, 0.005823508314652356931, 0.006655431812610384211, 0.007487355310568412359, 0.008319278808526441374, 0.009983125804442492465, 0.01081504930240051801, 0.01164697280035854356, 0.01331081979627459812, 0.01414274329423262540, 0.01497466679219065094, 0.01663851378810670203, 0.01830236078402274619, 0.01996620777993879381, 0.02329390177177089599, 0.02662159576360300164 ),
 .UNSPECIFIED. ) ;
#38465 = AXIS2_PLACEMENT_3D ( 'NONE', #18030, #2207, #14747 ) ;
#38466 = FACE_BOUND ( 'NONE', #19540, .T. ) ;
#38467 = CARTESIAN_POINT ( 'NONE',  ( 0.1402207406671886758, -0.9448101387227968440, 0.3912908471735270233 ) ) ;
#38468 = B_SPLINE_CURVE_WITH_KNOTS ( 'NONE', 3,
 ( #19747, #23262, #35788, #25533, #3720, #35388 ),
 .UNSPECIFIED., .F., .F.,
 ( 4, 2, 4 ),
 ( 0.000000000000000000, 0.0006454259618566229222, 0.001290851923713245844 ),
 .UNSPECIFIED. ) ;
#38469 = CARTESIAN_POINT ( 'NONE',  ( -0.03674260963082394416, -0.4430101671189292656, 0.1867880763203681183 ) ) ;
#38470 = CARTESIAN_POINT ( 'NONE',  ( 0.5862218696159900988, -1.490016463657622525, 0.6275474636321008992 ) ) ;
#38471 = CARTESIAN_POINT ( 'NONE',  ( 0.4299965955316200072, -1.218712715363120980, 0.6395725852502865960 ) ) ;
#38472 = APPLIED_SECURITY_CLASSIFICATION_ASSIGNMENT ( #27300, ( #30575 ) ) ;
#38473 = DIRECTION ( 'NONE',  ( 0.000000000000000000, 0.000000000000000000, -1.000000000000000000 ) ) ;
#38474 = ADVANCED_FACE ( 'NONE', ( #13328 ), #26047, .F. ) ;
#38475 = EDGE_CURVE ( 'NONE', #15629, #34573, #14841, .T. ) ;
#38476 = CARTESIAN_POINT ( 'NONE',  ( 0.4604079122430825288, -1.154977203505554773, 0.4182417262808743597 ) ) ;
#38477 = AXIS2_PLACEMENT_3D ( 'NONE', #37261, #3300, #21846 ) ;
#38478 = CARTESIAN_POINT ( 'NONE',  ( -0.001474785693551563560, -0.8508472180491982728, 0.1457185332388710453 ) ) ;
#38479 = CARTESIAN_POINT ( 'NONE',  ( 0.01548846960707524721, 0.4638115001430989648, -0.2459753896937820483 ) ) ;
#38480 = CARTESIAN_POINT ( 'NONE',  ( -0.2746410161513770931, -2.891403747035983240, -0.7012825271972917829 ) ) ;
#38481 = FACE_OUTER_BOUND ( 'NONE', #16151, .T. ) ;
#38482 = DIRECTION ( 'NONE',  ( -1.298300809103830214E-16, -0.9600278957180266026, -0.2799043398077594724 ) ) ;
#38483 = CARTESIAN_POINT ( 'NONE',  ( 0.05634402396114598227, -0.2780622203583502650, 0.3651830615696499138 ) ) ;
#38484 = CARTESIAN_POINT ( 'NONE',  ( 0.1821586897988819453, -0.5033064891650144146, 0.1063490580930545742 ) ) ;
#38485 = CARTESIAN_POINT ( 'NONE',  ( 0.1102650794266757106, -1.419061346167812099, 0.5811333943417352765 ) ) ;
#38486 = CARTESIAN_POINT ( 'NONE',  ( -0.02000000000000000042, -1.682484669133182953, -0.03683853088544706417 ) ) ;
#38487 = CARTESIAN_POINT ( 'NONE',  ( 0.3962688442617325890, -1.689744230457778773, -0.5025684713971244610 ) ) ;
#38488 = CARTESIAN_POINT ( 'NONE',  ( 0.3048570497350418518, -1.756853555320991189, 0.5694442476137144826 ) ) ;
#38489 = AXIS2_PLACEMENT_3D ( 'NONE', #32419, #1195, #29354 ) ;
#38490 = VECTOR ( 'NONE', #3892, 39.37007874015748143 ) ;
#38491 = CARTESIAN_POINT ( 'NONE',  ( 0.6933708823975106572, -1.493733918961976714, 0.4749053888396611578 ) ) ;
#38492 = ORIENTED_EDGE ( 'NONE', *, *, #36090, .T. ) ;
#38493 = CARTESIAN_POINT ( 'NONE',  ( 0.3504057387187116679, -1.153664717295437070, 0.4422128889498895266 ) ) ;
#38494 = ORIENTED_EDGE ( 'NONE', *, *, #5884, .T. ) ;
#38495 = LOCAL_TIME ( 0, 53, 7.000000000000000000, #25043 ) ;
#38496 = CARTESIAN_POINT ( 'NONE',  ( 0.2656260279857282081, -1.687710829545293834, 0.5802884372567370663 ) ) ;
#38498 = ORIENTED_EDGE ( 'NONE', *, *, #13242, .F. ) ;
#38497 = CARTESIAN_POINT ( 'NONE',  ( 0.5191802974051609176, -1.366849940342511172, 0.7967361778819540552 ) ) ;
#38499 = EDGE_CURVE ( 'NONE', #1427, #21489, #12222, .T. ) ;
#38501 = ORIENTED_EDGE ( 'NONE', *, *, #1886, .T. ) ;
#38500 = DIRECTION ( 'NONE',  ( 1.000000000000000000, 6.779273404243070203E-32, 4.314083075427408311E-32 ) ) ;
#38502 = AXIS2_PLACEMENT_3D ( 'NONE', #23433, #39631, #23620 ) ;
#38504 = ORIENTED_EDGE ( 'NONE', *, *, #29215, .T. ) ;
#38503 = ORIENTED_EDGE ( 'NONE', *, *, #28025, .T. ) ;
#38505 = CARTESIAN_POINT ( 'NONE',  ( 0.6094085419975362461, -1.415843169154349379, 0.8536811844606672084 ) ) ;
#38506 = ORIENTED_EDGE ( 'NONE', *, *, #9735, .T. ) ;
#38507 = CARTESIAN_POINT ( 'NONE',  ( 0.3734441402355138662, -1.768196402555201052, -0.5721408755833873316 ) ) ;
#38508 = CARTESIAN_POINT ( 'NONE',  ( 0.6100529622307712119, -1.615500794165734444, -0.5228307121444174532 ) ) ;
#38509 = CALENDAR_DATE ( 2026, 13, 10 ) ;
#38510 = CARTESIAN_POINT ( 'NONE',  ( 0.003741017115097356686, -0.5275076572294760124, 0.09509064842808913343 ) ) ;
#38511 = VERTEX_POINT ( 'NONE', #39027 ) ;
#38512 = CARTESIAN_POINT ( 'NONE',  ( 0.08797380359565291907, -0.7919620400412524797, 0.2352302520415841813 ) ) ;
#38513 = CARTESIAN_POINT ( 'NONE',  ( 0.06924657340766490754, -0.5400045880099092477, 0.1437216542238689831 ) ) ;
#38514 = CARTESIAN_POINT ( 'NONE',  ( 0.2162141278466277738, -0.8955401101134577990, 0.7086684481727526519 ) ) ;
#38515 = VERTEX_POINT ( 'NONE', #26899 ) ;
#38516 = CARTESIAN_POINT ( 'NONE',  ( 0.06318324162253809162, -1.280059889144033347, 0.6358524534319103250 ) ) ;
#38517 = CARTESIAN_POINT ( 'NONE',  ( 0.6984034912018327601, -1.438197739948913867, 0.5391927685615289789 ) ) ;
#38518 = CARTESIAN_POINT ( 'NONE',  ( 0.3216131088691095985, -1.758533047554937223, 0.5670923938871434977 ) ) ;
#38519 = CARTESIAN_POINT ( 'NONE',  ( 0.6980269330248262127, -1.438763980271349441, 0.5584498293197519558 ) ) ;
#38520 = CARTESIAN_POINT ( 'NONE',  ( 0.4848381743978809055, -1.590261796594116150, -0.5819748978324561506 ) ) ;
#38521 = CARTESIAN_POINT ( 'NONE',  ( 0.4865408785632933664, -1.302845980766627054, 0.8126564211098294965 ) ) ;
#38522 = CARTESIAN_POINT ( 'NONE',  ( 0.01172020176831022747, -0.7044715892658922618, -0.1131725940245311424 ) ) ;
#38523 = CARTESIAN_POINT ( 'NONE',  ( 0.02953079040095704308, 0.3810518745593911571, 0.3687679460475725701 ) ) ;
#38524 = CARTESIAN_POINT ( 'NONE',  ( 0.006049231046327587132, -0.8455795405855527358, 0.1352646710980445199 ) ) ;
#38525 = CARTESIAN_POINT ( 'NONE',  ( 0.04230188431063419685, -0.4483687697007490147, -0.1365048020681091379 ) ) ;
#38526 = VECTOR ( 'NONE', #40328, 39.37007874015748143 ) ;
#38527 = CARTESIAN_POINT ( 'NONE',  ( 0.1224152969000399382, -1.440949543414774547, 0.5682417262808782121 ) ) ;
#38528 = CARTESIAN_POINT ( 'NONE',  ( 0.4829770732687932999, -1.083865320555347678, 0.6394302686688468906 ) ) ;
#38529 = APPROVAL_STATUS ( 'not_yet_approved' ) ;
#38530 = LINE ( 'NONE', #10361, #28719 ) ;
#38531 = FACE_OUTER_BOUND ( 'NONE', #35509, .T. ) ;
#38532 = B_SPLINE_CURVE_WITH_KNOTS ( 'NONE', 3,
 ( #24429, #33464, #27517, #36963, #34078, #37177 ),
 .UNSPECIFIED., .F., .F.,
 ( 4, 2, 4 ),
 ( 0.001438281905272879684, 0.002932816318273989611, 0.004427350731275099538 ),
 .UNSPECIFIED. ) ;
#38533 = VERTEX_POINT ( 'NONE', #39843 ) ;
#38534 = CARTESIAN_POINT ( 'NONE',  ( 0.4343951858081425144, -1.578589645844999279, 0.5985257411299329533 ) ) ;
#38535 = CARTESIAN_POINT ( 'NONE',  ( 0.002367394983748904915, -0.5282119844061563541, 0.1394354128953861627 ) ) ;
#38536 = CARTESIAN_POINT ( 'NONE',  ( 0.3445219659096331322, -1.630113034086819290, -0.4330379103484555681 ) ) ;
#38537 = ORIENTED_EDGE ( 'NONE', *, *, #36308, .T. ) ;
#38538 = CIRCLE ( 'NONE', #3083, 0.1333070866141734534 ) ;
#38539 = FACE_OUTER_BOUND ( 'NONE', #3, .T. ) ;
#38540 = EDGE_CURVE ( 'NONE', #30458, #23204, #20104, .T. ) ;
#38541 = ADVANCED_FACE ( 'NONE', ( #10859 ), #39281, .T. ) ;
#38542 = CARTESIAN_POINT ( 'NONE',  ( 0.1905506861939139096, -0.5145941129025596306, 0.2257199139534598609 ) ) ;
#38544 = VERTEX_POINT ( 'NONE', #8161 ) ;
#38543 = VERTEX_POINT ( 'NONE', #29772 ) ;
#38545 = EDGE_CURVE ( 'NONE', #17659, #15479, #37180, .T. ) ;
#38546 = CARTESIAN_POINT ( 'NONE',  ( -0.01548846960707524721, 0.2306506793134049660, -0.4716198300880325434 ) ) ;
#38547 = CARTESIAN_POINT ( 'NONE',  ( 0.3601874435097799920, -1.787344030326375899, -0.5040241098297806310 ) ) ;
#38548 = SECURITY_CLASSIFICATION ( '', '', #27400 ) ;
#38549 = CARTESIAN_POINT ( 'NONE',  ( 0.2040530089634621236, -1.652187626897218653, -0.3590702193978799750 ) ) ;
#38550 = EDGE_CURVE ( 'NONE', #28258, #24493, #29080, .T. ) ;
#38551 = FACE_OUTER_BOUND ( 'NONE', #28701, .T. ) ;
#38552 = EDGE_LOOP ( 'NONE', ( #8023, #35608 ) ) ;
#38553 = CARTESIAN_POINT ( 'NONE',  ( 0.3739525536434556985, -1.751444307789024046, 0.9007940926418832595 ) ) ;
#38554 = ADVANCED_FACE ( 'NONE', ( #26491 ), #5629, .F. ) ;
#38555 = AXIS2_PLACEMENT_3D ( 'NONE', #29554, #23422, #10848 ) ;
#38556 = CARTESIAN_POINT ( 'NONE',  ( 0.1369077038689281156, -0.7638282256189674602, 0.4971742401558476576 ) ) ;
#38557 = CARTESIAN_POINT ( 'NONE',  ( 0.001081227941644962018, -0.4583518364089779196, 0.2957653468694024790 ) ) ;
#38558 = CARTESIAN_POINT ( 'NONE',  ( 0.4710354801145309467, -1.557935119788602663, 0.5965418981594908798 ) ) ;
#38560 = CARTESIAN_POINT ( 'NONE',  ( -0.1157923916715166146, -0.5295015842444106280, 0.3181161673586325178 ) ) ;
#38559 = CARTESIAN_POINT ( 'NONE',  ( 0.4582055935369603317, -1.592191023407962813, -0.4280546469726743686 ) ) ;
#38561 = CARTESIAN_POINT ( 'NONE',  ( 0.2251673531641388559, -1.129950269915442451, 0.6482802119689150544 ) ) ;
#38562 = EDGE_LOOP ( 'NONE', ( #11238, #12438 ) ) ;
#38563 = FACE_BOUND ( 'NONE', #25374, .T. ) ;
#38564 = CARTESIAN_POINT ( 'NONE',  ( 0.2649422998572272814, -0.6790022894220869576, 0.6063299226072803583 ) ) ;
#38565 = CARTESIAN_POINT ( 'NONE',  ( -0.04285561529641115919, 0.2295129201144932019, -0.4383679482630419288 ) ) ;
#38566 = EDGE_CURVE ( 'NONE', #25808, #5617, #14751, .T. ) ;
#38567 = APPLIED_PERSON_AND_ORGANIZATION_ASSIGNMENT ( #38071, #10099, ( #25357 ) ) ;
#38568 = DIRECTION ( 'NONE',  ( 1.000000000000000000, -0.000000000000000000, -0.000000000000000000 ) ) ;
#38569 = FACE_OUTER_BOUND ( 'NONE', #1002, .T. ) ;
#38570 = AXIS2_PLACEMENT_3D ( 'NONE', #34990, #13391, #4115 ) ;
#38571 = CARTESIAN_POINT ( 'NONE',  ( 0.6027116599735458102, -1.274749097762014616, 0.7879118535713135474 ) ) ;
#38572 = DIRECTION ( 'NONE',  ( 1.000000000000000000, 2.341930812374887555E-31, -1.664003471950578127E-31 ) ) ;
#38573 = CARTESIAN_POINT ( 'NONE',  ( -0.0008089698081453983516, -0.8558335556528616772, 0.3273597777360900962 ) ) ;
#38574 = ORGANIZATION ( 'NAUO-ORG19', 'UNSPECIFIED', 'UNSPECIFIED' ) ;
#38575 = B_SPLINE_CURVE_WITH_KNOTS ( 'NONE', 3,
 ( #23062, #11110, #13778, #4109, #10316, #19965, #877, #7805, #35203, #3913, #20181, #32706, #20375, #13595, #16471, #29013, #13382, #35591, #38484, #4513, #22880 ),
 .UNSPECIFIED., .F., .F.,
 ( 4, 2, 2, 2, 2, 2, 2, 1, 2, 2, 4 ),
 ( 0.000000000000000000, 0.1250000000000031641, 0.1875000000000039690, 0.2500000000000047740, 0.3125000000000055511, 0.3750000000000063838, 0.4375000000000071609, 0.4687500000000072164, 0.4843750000000069389, 0.5000000000000066613, 1.000000000000000000 ),
 .UNSPECIFIED. ) ;
#38576 = CARTESIAN_POINT ( 'NONE',  ( 0.02242828275838943536, 0.5043161982042990710, -0.09034400517546621601 ) ) ;
#38577 = CARTESIAN_POINT ( 'NONE',  ( 0.4781934768423675708, -1.682642038360962378, -0.6151431148613255573 ) ) ;
#38578 = CARTESIAN_POINT ( 'NONE',  ( 0.3764860865686396330, -1.114925686102496760, 0.7584753650261379931 ) ) ;
#38579 = CARTESIAN_POINT ( 'NONE',  ( 0.03664605387828129973, -0.04106737781738728499, 0.4792329708773133135 ) ) ;
#38580 = CARTESIAN_POINT ( 'NONE',  ( 0.5529638661199859362, -1.384232351104116132, 0.6057417262806752412 ) ) ;
#38581 = EDGE_LOOP ( 'NONE', ( #5293, #33221, #35889, #38193 ) ) ;
#38582 = DIRECTION ( 'NONE',  ( 0.000000000000000000, -0.9246857012436752177, 0.3807313408632033713 ) ) ;
#38583 = DIRECTION ( 'NONE',  ( 5.551115123125790098E-17, -6.347865096700338130E-31, -1.000000000000000000 ) ) ;
#38584 = CARTESIAN_POINT ( 'NONE',  ( 0.3066637369260901691, -1.757170009578179259, 0.5393777584040966300 ) ) ;
#38585 = SPHERICAL_SURFACE ( 'NONE', #24583, 0.01499999999999999944 ) ;
#38586 = CARTESIAN_POINT ( 'NONE',  ( 0.1343100678673626591, -1.002698383554990080, 0.7034404322865410730 ) ) ;
#38587 = ORIENTED_EDGE ( 'NONE', *, *, #20268, .F. ) ;
#38588 = ADVANCED_FACE ( 'NONE', ( #1409 ), #11061, .F. ) ;
#38589 = CARTESIAN_POINT ( 'NONE',  ( -0.03158843595483526445, -0.3316344853930296988, -0.3635668653053525934 ) ) ;
#38590 = CARTESIAN_POINT ( 'NONE',  ( -0.2399999999999999079, -4.120026397279962005, -0.6279592245183788224 ) ) ;
#38591 = DIRECTION ( 'NONE',  ( 0.03712106494698044767, -0.7041771612121668911, -0.7090532787910764911 ) ) ;
#38592 = CARTESIAN_POINT ( 'NONE',  ( 0.2026013104559352129, -1.284966392796108803, -0.7446432428005457238 ) ) ;
#38593 = EDGE_CURVE ( 'NONE', #38334, #30207, #20782, .T. ) ;
#38594 = CARTESIAN_POINT ( 'NONE',  ( 0.4837475926090684109, -1.264528724657570935, 0.6352410761543320072 ) ) ;
#38596 = CARTESIAN_POINT ( 'NONE',  ( 0.3844223753957967671, -1.715130776584119277, 0.4199023193696783673 ) ) ;
#38595 = DIRECTION ( 'NONE',  ( 1.702140497302369487E-12, 0.5877852522924830181, 0.8090169943749403458 ) ) ;
#38597 = DIRECTION ( 'NONE',  ( -7.771561172376107616E-16, 7.170354002788761615E-17, -1.000000000000000000 ) ) ;
#38598 = VERTEX_POINT ( 'NONE', #7756 ) ;
#38599 = APPROVAL_DATE_TIME ( #35321, #23717 ) ;
#38600 = EDGE_CURVE ( 'NONE', #33391, #35061, #34576, .T. ) ;
#38601 = CARTESIAN_POINT ( 'NONE',  ( -2.070754768975505034, -0.09959325338431362917, 0.09999999999999933942 ) ) ;
#38602 = VERTEX_POINT ( 'NONE', #20520 ) ;
#38603 = CARTESIAN_POINT ( 'NONE',  ( 0.07888544339681141659, -0.7040216271993084973, 0.5309320636121914738 ) ) ;
#38605 = CARTESIAN_POINT ( 'NONE',  ( 0.2031749929763018991, -0.6988986647121863127, 0.3457752107024871790 ) ) ;
#38604 = CARTESIAN_POINT ( 'NONE',  ( 0.08562435543972576890, -0.8179388245747207797, 0.08379651577411588448 ) ) ;
#38606 = CARTESIAN_POINT ( 'NONE',  ( 0.2230958589031876160, -1.614348418715432221, -0.3562888994457304448 ) ) ;
#38607 = EDGE_LOOP ( 'NONE', ( #32358, #25366, #29438, #16093, #4527, #16753, #31880, #12491, #12315, #20870, #402, #33951 ) ) ;
#38608 = CARTESIAN_POINT ( 'NONE',  ( 0.3280207512787571833, -1.293371038683761354, 0.5714539138005585439 ) ) ;
#38609 = CARTESIAN_POINT ( 'NONE',  ( 0.4829257366551612529, -1.359094011964862014, 0.8132530520444929412 ) ) ;
#38610 = CIRCLE ( 'NONE', #20898, 0.02999999999999997807 ) ;
#38611 = ORIENTED_EDGE ( 'NONE', *, *, #11422, .T. ) ;
#38612 = CARTESIAN_POINT ( 'NONE',  ( 0.3860292282735227620, -1.790736048274133685, -0.5258466387971835188 ) ) ;
#38613 = CARTESIAN_POINT ( 'NONE',  ( 0.05227399809316079365, -1.457268265538602670, -0.3759856532797451467 ) ) ;
#38614 = ADVANCED_FACE ( 'NONE', ( #33055 ), #16699, .T. ) ;
#38615 = LINE ( 'NONE', #3850, #8665 ) ;
#38616 = ORIENTED_EDGE ( 'NONE', *, *, #8472, .F. ) ;
#38617 = CARTESIAN_POINT ( 'NONE',  ( -0.02953079040095693900, -0.2329676531120485339, -0.4763574306556319637 ) ) ;
#38618 = CARTESIAN_POINT ( 'NONE',  ( -0.2746410161513782033, -1.990692974992658737, -0.4647843861454829528 ) ) ;
#38619 = CARTESIAN_POINT ( 'NONE',  ( 0.4428400309745522123, -1.146281092196613338, -0.3830631589809549431 ) ) ;
#38620 = CARTESIAN_POINT ( 'NONE',  ( 0.6473156011871936677, -1.349322671506162141, 0.8501878200258047302 ) ) ;
#38621 = CARTESIAN_POINT ( 'NONE',  ( 0.4149351083933472961, -1.715145687224109095, -0.4973294153635586801 ) ) ;
#38622 = CARTESIAN_POINT ( 'NONE',  ( -0.08000000000000000167, -2.551729310907437043, -0.5086726180052709712 ) ) ;
#38623 = CARTESIAN_POINT ( 'NONE',  ( -0.05464101615137795243, -1.669835911085076674, -0.2333336242928227000 ) ) ;
#38624 = COORDINATED_UNIVERSAL_TIME_OFFSET ( 0, 0, .AHEAD. ) ;
#38625 = CARTESIAN_POINT ( 'NONE',  ( 0.6567205214941880254, -1.402512679334766643, -0.6099112297698211504 ) ) ;
#38626 = CARTESIAN_POINT ( 'NONE',  ( 0.05279755784604189817, 0.3065965315811379766, 0.3541401437853790579 ) ) ;
#38627 = DIRECTION ( 'NONE',  ( -1.000000000000000000, -6.779273404243070203E-32, -4.314083075427408311E-32 ) ) ;
#38628 = CARTESIAN_POINT ( 'NONE',  ( 0.4386021513105624603, -1.229571196490931717, 0.4807399952002933685 ) ) ;
#38629 = DIRECTION ( 'NONE',  ( 0.4999551463232377313, -0.8660512985181132439, 0.000000000000000000 ) ) ;
#38630 = CARTESIAN_POINT ( 'NONE',  ( 0.01517484414490882783, -0.7999702980829028753, 0.5364596547344525623 ) ) ;
#38631 = DIRECTION ( 'NONE',  ( 1.000000000000000000, 0.000000000000000000, 0.000000000000000000 ) ) ;
#38632 = CARTESIAN_POINT ( 'NONE',  ( 0.4196702119927928076, -1.647204429517209023, -0.4088696122891719575 ) ) ;
#38633 = DIRECTION ( 'NONE',  ( 0.4999551463232373427, -0.8660512985181134660, 0.000000000000000000 ) ) ;
#38634 = CARTESIAN_POINT ( 'NONE',  ( 0.2026534980585697476, -1.284936265343112227, -0.2885610809406460309 ) ) ;
#38635 = AXIS2_PLACEMENT_3D ( 'NONE', #39460, #2247, #14170 ) ;
#38636 = EDGE_LOOP ( 'NONE', ( #1332, #14260, #265, #31457 ) ) ;
#38637 = VERTEX_POINT ( 'NONE', #31999 ) ;
#38638 = EDGE_CURVE ( 'NONE', #13200, #37623, #16812, .T. ) ;
#38639 = CARTESIAN_POINT ( 'NONE',  ( 0.3625960434667522270, -1.762758894398491982, -0.5926935080085825591 ) ) ;
#38640 = EDGE_LOOP ( 'NONE', ( #18103, #24897, #40535, #12381 ) ) ;
#38641 = DIRECTION ( 'NONE',  ( 1.000000000000000000, 6.779273404243070203E-32, 4.314083075427407763E-32 ) ) ;
#38642 = DIRECTION ( 'NONE',  ( 0.000000000000000000, 0.000000000000000000, -1.000000000000000000 ) ) ;
#38643 = EDGE_CURVE ( 'NONE', #35126, #23460, #40469, .T. ) ;
#38644 = CARTESIAN_POINT ( 'NONE',  ( 0.5515672481317782649, -1.380278329912550284, 0.6412555363875834802 ) ) ;
#38646 = ORIENTED_EDGE ( 'NONE', *, *, #1442, .F. ) ;
#38645 = CARTESIAN_POINT ( 'NONE',  ( 0.6590705178848084156, -1.601721441849921268, 0.5182417262812423209 ) ) ;
#38647 = CARTESIAN_POINT ( 'NONE',  ( 0.2618294899476097393, -0.7990503781373888836, 0.5447687035333291794 ) ) ;
#38648 = EDGE_CURVE ( 'NONE', #29903, #6931, #3617, .T. ) ;
#38649 = DIRECTION ( 'NONE',  ( 0.000000000000000000, 0.000000000000000000, -1.000000000000000000 ) ) ;
#38650 = ORIENTED_EDGE ( 'NONE', *, *, #1372, .T. ) ;
#38651 = CARTESIAN_POINT ( 'NONE',  ( 0.3242406000204350880, -1.171967933293699637, 0.5631067911264762138 ) ) ;
#38652 = ORIENTED_EDGE ( 'NONE', *, *, #33366, .T. ) ;
#38653 = CARTESIAN_POINT ( 'NONE',  ( 0.3306735325123419944, -1.633537559201160061, 0.6703962882651552935 ) ) ;
#38655 = CARTESIAN_POINT ( 'NONE',  ( -0.04230188431063396093, -0.4483687697007506245, 0.1365048020681099428 ) ) ;
#38654 = FACE_OUTER_BOUND ( 'NONE', #22514, .T. ) ;
#38656 = CARTESIAN_POINT ( 'NONE',  ( 0.03113248654051843992, 0.6304109427692223822, -0.1442409525262416947 ) ) ;
#38657 = CARTESIAN_POINT ( 'NONE',  ( 5.653807113072445720E-06, -2.020207405608465123, -0.2840335132522610051 ) ) ;
#38658 = ORIENTED_EDGE ( 'NONE', *, *, #34387, .F. ) ;
#38659 = CARTESIAN_POINT ( 'NONE',  ( 0.3211494819420748215, -1.297383677212298636, 0.5148643787740219135 ) ) ;
#38660 = CARTESIAN_POINT ( 'NONE',  ( 0.1852744361557795982, -0.8388916875311454024, 0.1498968110020814648 ) ) ;
#38661 = CARTESIAN_POINT ( 'NONE',  ( -0.03171893264489724501, -0.4702476704888112202, 0.2325692314475058253 ) ) ;
#38662 = DIRECTION ( 'NONE',  ( -0.8660254037844390407, 0.3535533905932734533, -0.3535533905932734533 ) ) ;
#38663 = EDGE_CURVE ( 'NONE', #28258, #545, #33242, .T. ) ;
#38664 = CARTESIAN_POINT ( 'NONE',  ( 0.1748016489742494628, -0.9194174328440815058, 0.6210426057618604334 ) ) ;
#38665 = CARTESIAN_POINT ( 'NONE',  ( 0.01548846960712800709, -0.4730347584885825629, 0.2341461249029146152 ) ) ;
#38666 = B_SPLINE_CURVE_WITH_KNOTS ( 'NONE', 3,
 ( #1053, #31876, #3694, #35553, #841, #13348, #4290, #25924, #38447, #13562, #5087, #36361, #39650, #17647, #11080, #35971, #14773, #24239 ),
 .UNSPECIFIED., .F., .F.,
 ( 4, 2, 2, 2, 2, 2, 2, 2, 4 ),
 ( 0.007419921033514278487, 0.008176191601852815169, 0.008932462170191350984, 0.009310597454360615421, 0.009688732738529879859, 0.01044500330686841567, 0.01120127387520694975, 0.01195754444354548210, 0.01347008558022255026 ),
 .UNSPECIFIED. ) ;
#38667 = EDGE_CURVE ( 'NONE', #10794, #33645, #3038, .T. ) ;
#38668 = CARTESIAN_POINT ( 'NONE',  ( 0.4065932041851609835, -1.147918556006405577, 0.4182417262808777458 ) ) ;
#38669 = ADVANCED_FACE ( 'NONE', ( #25442 ), #2758, .T. ) ;
#38670 = CARTESIAN_POINT ( 'NONE',  ( -0.1623927644724122987, 0.5045516355107032558, 0.3253307341376669437 ) ) ;
#38671 = CARTESIAN_POINT ( 'NONE',  ( -0.1129900121204593377, -0.5167580615068131378, 0.1415474730880576515 ) ) ;
#38672 = ADVANCED_FACE ( 'NONE', ( #28509 ), #34874, .F. ) ;
#38673 = FACE_OUTER_BOUND ( 'NONE', #7409, .T. ) ;
#38674 = FACE_OUTER_BOUND ( 'NONE', #8696, .T. ) ;
#38675 = CARTESIAN_POINT ( 'NONE',  ( 0.04566385930017818201, -1.214514029449272892, 0.6761745275914542441 ) ) ;
#38676 = CARTESIAN_POINT ( 'NONE',  ( 0.1905398795079399077, -1.256391271284680533, -0.3903413229800113959 ) ) ;
#38677 = DIRECTION ( 'NONE',  ( 0.000000000000000000, -0.4393346272636243222, 0.8983234858819689750 ) ) ;
#38678 = ORIENTED_EDGE ( 'NONE', *, *, #12169, .F. ) ;
#38679 = PRODUCT_DEFINITION_SHAPE ( 'NONE', 'NONE',  #40650 ) ;
#38680 = CARTESIAN_POINT ( 'NONE',  ( 0.4610032414159208614, -1.686334621966218306, 0.4527853876349565709 ) ) ;
#38681 = CARTESIAN_POINT ( 'NONE',  ( 0.4143292853021347533, -1.740072816664171684, -0.5834784908774952594 ) ) ;
#38682 = CARTESIAN_POINT ( 'NONE',  ( 0.2665932999777489432, -1.539397319814852949, 0.9862784934333517217 ) ) ;
#38683 = CARTESIAN_POINT ( 'NONE',  ( 0.6714407672615939626, -1.521867659483790547, 0.4359222191939696733 ) ) ;
#38684 = VERTEX_POINT ( 'NONE', #584 ) ;
#38685 = ORIENTED_EDGE ( 'NONE', *, *, #19527, .T. ) ;
#38686 = CARTESIAN_POINT ( 'NONE',  ( -0.02000000000000000042, -1.968175500587574067, -0.6048844944454191408 ) ) ;
#38687 = ORIENTED_EDGE ( 'NONE', *, *, #13427, .F. ) ;
#38688 = DIRECTION ( 'NONE',  ( 1.000000000000000000, -0.000000000000000000, -0.000000000000000000 ) ) ;
#38689 = EDGE_CURVE ( 'NONE', #37319, #2531, #36534, .T. ) ;
#38690 = CARTESIAN_POINT ( 'NONE',  ( 0.5943265527529638659, -1.468666372280408972, 0.6816657076235226320 ) ) ;
#38692 = ORIENTED_EDGE ( 'NONE', *, *, #31760, .T. ) ;
#38691 = CARTESIAN_POINT ( 'NONE',  ( 0.1539501873670340859, -1.278399339615925667, 0.4182417262808778013 ) ) ;
#38693 = EDGE_CURVE ( 'NONE', #28467, #478, #25364, .T. ) ;
#38695 = ORIENTED_EDGE ( 'NONE', *, *, #18426, .F. ) ;
#38694 = ORIENTED_EDGE ( 'NONE', *, *, #3438, .F. ) ;
#38696 = CARTESIAN_POINT ( 'NONE',  ( -0.01548846960707531660, -0.4770632572900511681, -0.2530032579707427454 ) ) ;
#38697 = VERTEX_POINT ( 'NONE', #29111 ) ;
#38698 = LINE ( 'NONE', #13799, #6164 ) ;
#38699 = CARTESIAN_POINT ( 'NONE',  ( 0.1801302324021237800, -1.378194537208108361, 0.5482363894879486166 ) ) ;
#38700 = DIRECTION ( 'NONE',  ( 1.000000000000000000, 0.000000000000000000, 0.000000000000000000 ) ) ;
#38701 = COORDINATED_UNIVERSAL_TIME_OFFSET ( 0, 0, .AHEAD. ) ;
#38702 = DIRECTION ( 'NONE',  ( -1.232595164407830672E-32, -0.6645646360916346307, 0.7472307839325098566 ) ) ;
#38704 = EDGE_LOOP ( 'NONE', ( #469, #613, #3371, #5454, #30312, #1015, #7110 ) ) ;
#38703 = ORIENTED_EDGE ( 'NONE', *, *, #24920, .T. ) ;
#38705 = CARTESIAN_POINT ( 'NONE',  ( 0.2439697435047648300, -0.9572542734378898244, 0.6693538292162648506 ) ) ;
#38706 = DIRECTION ( 'NONE',  ( 1.000000000000000000, 1.450080480853946466E-15, -8.881784197001242463E-16 ) ) ;
#38707 = CARTESIAN_POINT ( 'NONE',  ( 0.5388164341061177920, -1.518966147603598049, 0.5683445443996597568 ) ) ;
#38708 = VERTEX_POINT ( 'NONE', #974 ) ;
#38709 = CARTESIAN_POINT ( 'NONE',  ( 0.04171458440977070942, -1.134361221218466609, 0.6577934201144993720 ) ) ;
#38710 = CARTESIAN_POINT ( 'NONE',  ( 0.4907610854883471818, -1.588559784271378783, -0.4568777161905970274 ) ) ;
#38711 = CARTESIAN_POINT ( 'NONE',  ( -0.04582897286455953068, 0.06484386734940819630, 0.4825967645925812732 ) ) ;
#38712 = CARTESIAN_POINT ( 'NONE',  ( 0.3510995257679918602, -1.742526243202041192, 0.6036984576181094742 ) ) ;
#38713 = CARTESIAN_POINT ( 'NONE',  ( 0.1399999999999994582, 8.414405049830459540E-17, 0.2526340763130724976 ) ) ;
#38714 = DIRECTION ( 'NONE',  ( -0.9378410757839558132, 0.1072489841977658925, -0.3300784330442383396 ) ) ;
#38715 = DIRECTION ( 'NONE',  ( 8.881784197001246407E-16, -2.361472542561082612E-16, 1.000000000000000000 ) ) ;
#38716 = DIRECTION ( 'NONE',  ( -1.000000000000000000, -0.000000000000000000, -0.000000000000000000 ) ) ;
#38717 = CARTESIAN_POINT ( 'NONE',  ( -0.0001129244011828491533, -0.7912893389636214136, -0.08081660452504497993 ) ) ;
#38718 = CARTESIAN_POINT ( 'NONE',  ( 0.3688024341757283331, -1.123809055325019735, 0.8060765054549502429 ) ) ;
#38719 =( NAMED_UNIT ( * ) SI_UNIT ( $, .STERADIAN. ) SOLID_ANGLE_UNIT ( ) );
#38720 = CARTESIAN_POINT ( 'NONE',  ( 0.4971324743577882899, -1.079965756743124006, 0.4177417262808780229 ) ) ;
#38721 = CARTESIAN_POINT ( 'NONE',  ( 0.3609052982223109884, -1.620655244094860947, -0.5155029497116575543 ) ) ;
#38722 = CARTESIAN_POINT ( 'NONE',  ( -0.003124719664520056797, -0.8057675726412014683, 0.1627348865840318737 ) ) ;
#38723 = CARTESIAN_POINT ( 'NONE',  ( 0.4430687885351943245, -1.051147784193108281, 0.6535119922057798236 ) ) ;
#38724 = APPROVAL_STATUS ( 'not_yet_approved' ) ;
#38725 = CARTESIAN_POINT ( 'NONE',  ( 0.3699999999999786793, -2.166079853131637645, -0.5407606602423824516 ) ) ;
#38726 = CARTESIAN_POINT ( 'NONE',  ( -0.06034227824829814513, 0.05439570041090458635, -0.1249999999999998612 ) ) ;
#38727 = ORIENTED_EDGE ( 'NONE', *, *, #15467, .F. ) ;
#38728 = DIRECTION ( 'NONE',  ( -1.000000000000000000, -2.280301054154495132E-31, 1.664003471950577689E-31 ) ) ;
#38729 = CARTESIAN_POINT ( 'NONE',  ( 0.01210505692010079189, 0.06117178301711245769, 0.1249999999999993477 ) ) ;
#38730 = CARTESIAN_POINT ( 'NONE',  ( 0.2063161596972083733, -1.283719858747340625, -0.6406645764433035461 ) ) ;
#38731 = VERTEX_POINT ( 'NONE', #13489 ) ;
#38732 = DIRECTION ( 'NONE',  ( 0.4999999999999975575, 0.8322738431953016214, 0.2394164779895586459 ) ) ;
#38733 = CARTESIAN_POINT ( 'NONE',  ( 0.6807551469422991053, -1.407487954066357183, 0.5751647024762112093 ) ) ;
#38735 = ORIENTED_EDGE ( 'NONE', *, *, #12947, .F. ) ;
#38734 = EDGE_LOOP ( 'NONE', ( #17750, #12422, #21817, #20694 ) ) ;
#38736 = DIRECTION ( 'NONE',  ( -1.000000000000000000, 0.000000000000000000, 0.000000000000000000 ) ) ;
#38737 = EDGE_LOOP ( 'NONE', ( #39304, #34335, #27664 ) ) ;
#38738 = DIRECTION ( 'NONE',  ( 0.8660512985181134660, 0.4999551463232372317, 0.000000000000000000 ) ) ;
#38739 = CARTESIAN_POINT ( 'NONE',  ( 0.4101084439245127333, -1.675243471201324663, -0.5124304843287676992 ) ) ;
#38740 = DIRECTION ( 'NONE',  ( 1.000000000000000000, 0.000000000000000000, 0.000000000000000000 ) ) ;
#38741 = EDGE_LOOP ( 'NONE', ( #30855, #4293, #30189, #26355 ) ) ;
#38742 = CARTESIAN_POINT ( 'NONE',  ( 0.1875000000000003331, -0.4593131964907913867, 0.1457185332388697407 ) ) ;
#38743 = CARTESIAN_POINT ( 'NONE',  ( 0.1930736954529370941, -0.8449126200218157745, 0.6255041996076380340 ) ) ;
#38744 = DIRECTION ( 'NONE',  ( -0.4999551463232372317, 0.8660512985181134660, -0.000000000000000000 ) ) ;
#38745 = CARTESIAN_POINT ( 'NONE',  ( 0.08524078840219746767, -0.5428247996486973426, 0.1457185332388697407 ) ) ;
#38747 = DIRECTION ( 'NONE',  ( 0.000000000000000000, 0.000000000000000000, -1.000000000000000000 ) ) ;
#38746 = CARTESIAN_POINT ( 'NONE',  ( 0.2654443876445621298, -1.687660951001132004, 0.5779630316034871651 ) ) ;
#38748 = CARTESIAN_POINT ( 'NONE',  ( 0.1627198989308838994, -1.029848727310650469, 0.5977245216963805730 ) ) ;
#38749 = ORIENTED_EDGE ( 'NONE', *, *, #30892, .F. ) ;
#38750 = ORIENTED_EDGE ( 'NONE', *, *, #16428, .T. ) ;
#38751 = CARTESIAN_POINT ( 'NONE',  ( 0.3588042674141814214, -1.621950415644044963, 0.5547558322257422070 ) ) ;
#38752 = CARTESIAN_POINT ( 'NONE',  ( 0.2214772573562845126, -0.6571296826234386268, 0.4491444447770453485 ) ) ;
#38753 = CARTESIAN_POINT ( 'NONE',  ( -0.02881329448201560423, 0.2420398234037526297, -0.4354480552436177931 ) ) ;
#38754 = CARTESIAN_POINT ( 'NONE',  ( -0.01548846960707427230, -0.5203207976467948415, -0.08861466064782426433 ) ) ;
#38755 = CARTESIAN_POINT ( 'NONE',  ( -0.8248651029816859159, -8.267127619740731130E-16, -0.6154198107346400271 ) ) ;
#38756 = CARTESIAN_POINT ( 'NONE',  ( 0.1424029337235096226, -1.400533250147911746, -0.6250000000000000000 ) ) ;
#38757 = CARTESIAN_POINT ( 'NONE',  ( 0.4936113061342744524, -1.107001320208115036, 0.7496827700887727097 ) ) ;
#38758 = CARTESIAN_POINT ( 'NONE',  ( 0.5271543187458650470, -1.167382716756260042, 0.4878339827211743973 ) ) ;
#38759 = FACE_OUTER_BOUND ( 'NONE', #6101, .T. ) ;
#38760 = VECTOR ( 'NONE', #16638, 39.37007874015748143 ) ;
#38761 = CYLINDRICAL_SURFACE ( 'NONE', #28465, 0.1000000000000000194 ) ;
#38762 = CARTESIAN_POINT ( 'NONE',  ( 0.3289274145732573040, -1.292879115135177059, 0.4679791452570866150 ) ) ;
#38763 = ORIENTED_EDGE ( 'NONE', *, *, #30619, .T. ) ;
#38764 = CARTESIAN_POINT ( 'NONE',  ( 0.2270139475256796879, -0.9339256942224501978, 0.6530035840272132575 ) ) ;
#38765 = CARTESIAN_POINT ( 'NONE',  ( 0.03158843595483464689, -0.3316344853930294212, 0.3635668653053538146 ) ) ;
#38766 = DIRECTION ( 'NONE',  ( -1.355854680848614260E-31, 3.330669073875470114E-16, 1.000000000000000000 ) ) ;
#38767 = AXIS2_PLACEMENT_3D ( 'NONE', #23494, #20807, #11319 ) ;
#38768 = ORIENTED_EDGE ( 'NONE', *, *, #23058, .F. ) ;
#38769 = CARTESIAN_POINT ( 'NONE',  ( 0.4315909263077353786, -1.207668101024179430, 0.5182417262812423209 ) ) ;
#38770 = ORIENTED_EDGE ( 'NONE', *, *, #4454, .F. ) ;
#38771 = CARTESIAN_POINT ( 'NONE',  ( 0.08990536850430516647, -0.5646295866045974998, 0.1496696842286166784 ) ) ;
#38772 = CARTESIAN_POINT ( 'NONE',  ( 0.02999999999990876631, -2.097675084551054336, -0.7286989150923646186 ) ) ;
#38773 = CARTESIAN_POINT ( 'NONE',  ( 0.2219638282378538774, -1.211848774759766600, 0.7364796804151579890 ) ) ;
#38774 = ORIENTED_EDGE ( 'NONE', *, *, #20755, .F. ) ;
#38775 = CARTESIAN_POINT ( 'NONE',  ( -0.01548846960721245516, -0.3688619771570368910, -0.3775276577325204497 ) ) ;
#38776 = EDGE_CURVE ( 'NONE', #40488, #12799, #1099, .T. ) ;
#38777 = CARTESIAN_POINT ( 'NONE',  ( 0.03174060074382084595, 0.07585527192504755434, 0.5190439939302140537 ) ) ;
#38778 = CARTESIAN_POINT ( 'NONE',  ( 0.03643058821097028971, -0.5061858935230133527, -0.07642520143595077364 ) ) ;
#38779 = PRODUCT_DEFINITION ( 'UNKNOWN', '', #5625, #32707 ) ;
#38780 = DIRECTION ( 'NONE',  ( -0.000000000000000000, -0.5365213554527469286, 0.8438867430782088785 ) ) ;
#38781 = CARTESIAN_POINT ( 'NONE',  ( 0.3773743308125420692, -1.120461712655230091, 0.7152730075388841202 ) ) ;
#38783 = DIRECTION ( 'NONE',  ( 0.8660512985181133550, 0.4999551463232372317, 0.000000000000000000 ) ) ;
#38782 = CARTESIAN_POINT ( 'NONE',  ( 0.4027068045633697690, -1.135255088841635729, 0.5012202440948826387 ) ) ;
#38784 = CARTESIAN_POINT ( 'NONE',  ( 0.3026114960654325836, -0.9782852559307895213, 0.5634791713200563157 ) ) ;
#38785 = ORIENTED_EDGE ( 'NONE', *, *, #16782, .T. ) ;
#38786 = SPHERICAL_SURFACE ( 'NONE', #11908, 0.01499999999999999944 ) ;
#38787 = ORIENTED_EDGE ( 'NONE', *, *, #23159, .T. ) ;
#38788 = CARTESIAN_POINT ( 'NONE',  ( 0.06044531019120238241, -0.6298155687119810775, 0.4117843844938999243 ) ) ;
#38790 = CARTESIAN_POINT ( 'NONE',  ( 0.1744097386003500560, -0.9176933794257766674, 0.1353190812260986475 ) ) ;
#38789 = CARTESIAN_POINT ( 'NONE',  ( 0.08828494613019574611, -0.6323668545420986220, 0.03541928192839603751 ) ) ;
#38791 = CARTESIAN_POINT ( 'NONE',  ( 0.1907077899473081650, -1.700082312857616351, -0.3588694632811901819 ) ) ;
#38792 = VERTEX_POINT ( 'NONE', #29518 ) ;
#38793 = AXIS2_PLACEMENT_3D ( 'NONE', #13462, #10374, #35873 ) ;
#38794 = B_SPLINE_CURVE_WITH_KNOTS ( 'NONE', 3,
 ( #2565, #28078, #24971, #21691 ),
 .UNSPECIFIED., .F., .F.,
 ( 4, 4 ),
 ( 0.000000000000000000, 4.801453139129629977E-05 ),
 .UNSPECIFIED. ) ;
#38795 = VERTEX_POINT ( 'NONE', #32999 ) ;
#38796 = CARTESIAN_POINT ( 'NONE',  ( -0.2399999999999999079, -3.253611865733782693, -0.3464478357516359575 ) ) ;
#38797 = CARTESIAN_POINT ( 'NONE',  ( 0.5748884503991072981, -1.498777740968299188, 0.5996797115467191741 ) ) ;
#38798 = ORIENTED_EDGE ( 'NONE', *, *, #36152, .T. ) ;
#38799 = DIRECTION ( 'NONE',  ( -7.000205099780496893E-17, -1.000000000000000000, -6.590151126658374952E-16 ) ) ;
#38800 = CARTESIAN_POINT ( 'NONE',  ( 0.03171861681799757748, -0.5171399723077846344, 0.08825220573710579330 ) ) ;
#38801 = CIRCLE ( 'NONE', #40128, 0.01500000000000002547 ) ;
#38802 = EDGE_CURVE ( 'NONE', #18990, #12086, #14293, .T. ) ;
#38803 = CARTESIAN_POINT ( 'NONE',  ( 0.4175449395041774814, -1.738216479897680244, -0.4268450903248972028 ) ) ;
#38804 = VECTOR ( 'NONE', #25356, 39.37007874015748854 ) ;
#38805 = CARTESIAN_POINT ( 'NONE',  ( 0.1689017270382413005, -1.269576038341752700, 0.4229621067556875169 ) ) ;
#38806 = AXIS2_PLACEMENT_3D ( 'NONE', #31018, #40485, #18276 ) ;
#38807 = CARTESIAN_POINT ( 'NONE',  ( 0.4778170654558047126, -1.668016138613298560, 0.5682417262808788783 ) ) ;
#38808 = FACE_OUTER_BOUND ( 'NONE', #26930, .T. ) ;
#38809 = EDGE_CURVE ( 'NONE', #34759, #16750, #10907, .T. ) ;
#38810 = CARTESIAN_POINT ( 'NONE',  ( 0.5698123312952257935, -1.224001199585974087, 0.8774075775261976906 ) ) ;
#38811 = ADVANCED_FACE ( 'NONE', ( #33413 ), #26661, .F. ) ;
#38812 = CARTESIAN_POINT ( 'NONE',  ( 0.01548846960703782229, 0.3772621329472654605, -0.3651003739303476658 ) ) ;
#38813 = DIRECTION ( 'NONE',  ( 0.000000000000000000, 3.330669073875470114E-16, 1.000000000000000000 ) ) ;
#38814 = PERSON_AND_ORGANIZATION_ROLE ( 'design_owner' ) ;
#38815 = EDGE_CURVE ( 'NONE', #27374, #28606, #24667, .T. ) ;
#38816 = FACE_OUTER_BOUND ( 'NONE', #39974, .T. ) ;
#38817 = FACE_OUTER_BOUND ( 'NONE', #27267, .T. ) ;
#38818 = CARTESIAN_POINT ( 'NONE',  ( 0.1849146134180273127, -0.6975931602019068700, -0.02773678677584009988 ) ) ;
#38819 = EDGE_CURVE ( 'NONE', #31970, #3242, #16844, .T. ) ;
#38820 = CARTESIAN_POINT ( 'NONE',  ( -0.2399999999999999079, -2.183180860297908144, -0.4937760292030871079 ) ) ;
#38821 = CARTESIAN_POINT ( 'NONE',  ( -0.05082303569918696085, 0.4631054925596489458, -0.09932635337951989385 ) ) ;
#38822 = CARTESIAN_POINT ( 'NONE',  ( 0.003441938119505853853, -0.5826794048688673788, 0.2512083064573837898 ) ) ;
#38823 = CARTESIAN_POINT ( 'NONE',  ( 0.5875325861083496859, -1.566157533570999627, -0.5429603524405962611 ) ) ;
#38824 = DIRECTION ( 'NONE',  ( -1.000000000000000000, -2.280301054154495132E-31, 1.664003471950577689E-31 ) ) ;
#38825 = CIRCLE ( 'NONE', #2050, 0.08830708661417338567 ) ;
#38826 = DIRECTION ( 'NONE',  ( -0.4999999999999971134, -0.5122356157878134031, -0.6982941170584801016 ) ) ;
#38827 = CARTESIAN_POINT ( 'NONE',  ( -0.05279185365593383472, -0.3066183444142246417, 0.3541401447632906985 ) ) ;
#38828 = ORIENTED_EDGE ( 'NONE', *, *, #16685, .F. ) ;
#38829 = ORIENTED_EDGE ( 'NONE', *, *, #17306, .F. ) ;
#38830 = AXIS2_PLACEMENT_3D ( 'NONE', #11830, #36927, #30958 ) ;
#38831 = EDGE_CURVE ( 'NONE', #32272, #32303, #24743, .T. ) ;
#38832 = DIRECTION ( 'NONE',  ( -1.000000000000000000, 0.000000000000000000, 0.000000000000000000 ) ) ;
#38833 = ORIENTED_EDGE ( 'NONE', *, *, #35060, .F. ) ;
#38834 = VECTOR ( 'NONE', #37071, 39.37007874015748854 ) ;
#38835 = CARTESIAN_POINT ( 'NONE',  ( 0.01220508677664999299, -0.4284039737085656996, 0.1457185332388702959 ) ) ;
#38836 = FACE_OUTER_BOUND ( 'NONE', #7219, .T. ) ;
#38837 = CARTESIAN_POINT ( 'NONE',  ( 0.4924747549555801851, -1.284741442926763400, 0.7473512348121129634 ) ) ;
#38839 = ORIENTED_EDGE ( 'NONE', *, *, #29817, .F. ) ;
#38838 = CARTESIAN_POINT ( 'NONE',  ( -0.1542132178619239902, 0.4779941576916497126, 0.1100664889103544625 ) ) ;
#38840 = CARTESIAN_POINT ( 'NONE',  ( 0.4556718857535577705, -1.059138143784118302, 0.6919068033735837897 ) ) ;
#38841 = FACE_OUTER_BOUND ( 'NONE', #3936, .T. ) ;
#38842 = ORIENTED_EDGE ( 'NONE', *, *, #31693, .F. ) ;
#38843 = ORIENTED_EDGE ( 'NONE', *, *, #35867, .F. ) ;
#38844 = ORIENTED_EDGE ( 'NONE', *, *, #10262, .F. ) ;
#38845 = CARTESIAN_POINT ( 'NONE',  ( 0.02473703078937821917, -0.5631418136270044394, 0.2740291547039533926 ) ) ;
#38847 = CARTESIAN_POINT ( 'NONE',  ( 0.1113805825442736736, -0.9071550240875194682, 0.04606443103390334137 ) ) ;
#38846 = CARTESIAN_POINT ( 'NONE',  ( 0.6047538891612445067, -1.605163873594934065, 0.4396382108053981663 ) ) ;
#38848 = CARTESIAN_POINT ( 'NONE',  ( 0.05583995664670776682, -1.335624775257321817, 0.3157417262808777658 ) ) ;
#38849 = CARTESIAN_POINT ( 'NONE',  ( 0.08942791728960713948, -1.375947154762177105, -0.3595196034401970664 ) ) ;
#38850 = EDGE_LOOP ( 'NONE', ( #28082, #34703 ) ) ;
#38851 = DIRECTION ( 'NONE',  ( 1.000000000000000000, 0.000000000000000000, 0.000000000000000000 ) ) ;
#38852 = CARTESIAN_POINT ( 'NONE',  ( 0.3484951945142048535, -1.627819363848378220, -0.3328913857909800433 ) ) ;
#38853 = CARTESIAN_POINT ( 'NONE',  ( 0.1826249073287988522, -1.261667980084789420, 0.4182417262808778569 ) ) ;
#38854 = CARTESIAN_POINT ( 'NONE',  ( 0.04154009738085434611, 0.4523583096281919014, 0.1287716261385795091 ) ) ;
#38855 = CARTESIAN_POINT ( 'NONE',  ( 0.1524423687509998404, -0.8872256037779822080, 0.5537346710474807532 ) ) ;
#38856 = FACE_OUTER_BOUND ( 'NONE', #37844, .T. ) ;
#38857 = AXIS2_PLACEMENT_3D ( 'NONE', #10837, #4441, #17001 ) ;
#38858 = CARTESIAN_POINT ( 'NONE',  ( 0.1462308410358738320, -0.9164545692843373281, 0.1457042957556350660 ) ) ;
#38859 = CARTESIAN_POINT ( 'NONE',  ( 0.01548846960712783535, -0.2450655194479442189, 0.4674710490748163472 ) ) ;
#38860 = EDGE_CURVE ( 'NONE', #37863, #5937, #26068, .T. ) ;
#38861 = AXIS2_PLACEMENT_3D ( 'NONE', #24300, #23905, #2077 ) ;
#38862 = CARTESIAN_POINT ( 'NONE',  ( 0.1499999999999994948, -0.4770632572900429524, 0.2530032579707506835 ) ) ;
#38863 = CIRCLE ( 'NONE', #262, 0.05330708661417342398 ) ;
#38864 = DIRECTION ( 'NONE',  ( 1.000000000000000000, 0.000000000000000000, 0.000000000000000000 ) ) ;
#38865 = CARTESIAN_POINT ( 'NONE',  ( -0.06980746140711623082, -7.971802777789936683E-17, -0.1750000000000000167 ) ) ;
#38866 = CARTESIAN_POINT ( 'NONE',  ( 0.2737252524196370218, -1.671010326955969960, 0.4800311348041322868 ) ) ;
#38867 = AXIS2_PLACEMENT_3D ( 'NONE', #19068, #25238, #6697 ) ;
#38868 = EDGE_CURVE ( 'NONE', #8591, #25449, #6338, .T. ) ;
#38869 = CARTESIAN_POINT ( 'NONE',  ( 0.3834349357971629790, -1.149375767803377135, 0.4315005731421182600 ) ) ;
#38870 = EDGE_CURVE ( 'NONE', #3414, #9996, #14864, .T. ) ;
#38871 = DIRECTION ( 'NONE',  ( 0.9344312650838934031, 0.2480862795823838285, 0.2555218360858536597 ) ) ;
#38872 = PRODUCT_DEFINITION_CONTEXT ( 'detailed design', #29256, 'design' ) ;
#38873 = CARTESIAN_POINT ( 'NONE',  ( 0.1153471662232078698, -0.4465907064269051263, 0.1457432652200511269 ) ) ;
#38874 = CARTESIAN_POINT ( 'NONE',  ( 0.4382015218937659884, -1.612541052972227940, -0.6615483979663951963 ) ) ;
#38875 = CARTESIAN_POINT ( 'NONE',  ( 0.3624136781422674924, -1.762859772815410508, -0.5929287727032674926 ) ) ;
#38876 = CARTESIAN_POINT ( 'NONE',  ( 5.463695987328526437E-16, -0.2899999999999993694, -7.171100983368691195E-16 ) ) ;
#38877 = B_SPLINE_CURVE_WITH_KNOTS ( 'NONE', 3,
 ( #31627, #18896, #31434, #22806, #6720, #3240, #35329, #19088, #7118, #207, #15786, #13, #12495, #6929, #12699, #28936, #3442, #16000 ),
 .UNSPECIFIED., .F., .F.,
 ( 4, 2, 2, 2, 2, 2, 2, 2, 4 ),
 ( 0.005943923758767621912, 0.006685218669166347917, 0.007426513579565073922, 0.008167808489963800794, 0.008909103400362525932, 0.009650398310761251069, 0.01039169322115997794, 0.01113298813155870481, 0.01187428304195742995 ),
 .UNSPECIFIED. ) ;
#38878 = CARTESIAN_POINT ( 'NONE',  ( 0.01895884884825187189, -0.07380796352548207873, -0.5147901372834211564 ) ) ;
#38879 = EDGE_LOOP ( 'NONE', ( #39251, #31243, #31780, #38896, #25240 ) ) ;
#38880 = EDGE_CURVE ( 'NONE', #40536, #12086, #16196, .T. ) ;
#38881 = CARTESIAN_POINT ( 'NONE',  ( 0.1886928464339920619, -0.5387472362569383222, 0.2832338156061069423 ) ) ;
#38882 = ORIENTED_EDGE ( 'NONE', *, *, #3328, .T. ) ;
#38883 = CARTESIAN_POINT ( 'NONE',  ( -0.09579104668929012967, -0.04310840302198021973, 0.3599999999999992095 ) ) ;
#38884 = ADVANCED_FACE ( 'NONE', ( #39381 ), #20135, .T. ) ;
#38885 = B_SPLINE_CURVE_WITH_KNOTS ( 'NONE', 3,
 ( #12488, #31013, #2834, #27943, #40481, #12306, #37382, #21764, #34905, #37999, #22589, #31831, #13305, #6714, #19288, #31429, #13100, #607, #7112, #16597, #25660, #3648, #38393, #28328, #3436, #202, #19495, #19082, #6318, #38192, #16209, #3233, #18891, #28745, #15780, #3833, #21978, #10018, #34706, #35116, #25878, #15995, #28540, #9808 ),
 .UNSPECIFIED., .F., .F.,
 ( 4, 2, 2, 2, 2, 2, 2, 2, 2, 2, 2, 2, 2, 2, 2, 2, 2, 2, 2, 2, 2, 4 ),
 ( 7.720987835474815629E-06, 0.0008870064552703168593, 0.001766291922705158935, 0.002645577390140001553, 0.003524862857574843304, 0.004404148325009685054, 0.005283433792444528106, 0.006162719259879370290, 0.007042004727314211607, 0.008800575662183894241, 0.009679861129618742496, 0.01055914659705358728, 0.01143843206448843554, 0.01231771753192328206, 0.01319700299935812858, 0.01407628846679297684, 0.01583485940166267161, 0.01671414486909751987, 0.01759343033653236812, 0.02111057220627177503, 0.02462771407601118540, 0.02814485594575059230 ),
 .UNSPECIFIED. ) ;
#38886 = CIRCLE ( 'NONE', #11968, 0.07749999999977555398 ) ;
#38887 = CARTESIAN_POINT ( 'NONE',  ( 0.6018806508000521527, -1.483118007491554646, 0.5713872269410379401 ) ) ;
#38889 = ORIENTED_EDGE ( 'NONE', *, *, #20957, .T. ) ;
#38888 = LINE ( 'NONE', #38691, #19161 ) ;
#38890 = EDGE_CURVE ( 'NONE', #7737, #21571, #34596, .T. ) ;
#38892 = ORIENTED_EDGE ( 'NONE', *, *, #17491, .F. ) ;
#38891 = ORIENTED_EDGE ( 'NONE', *, *, #21073, .T. ) ;
#38893 = CARTESIAN_POINT ( 'NONE',  ( 0.1320833403089577973, -0.5364814942693221234, 0.4244164861031392566 ) ) ;
#38894 = CIRCLE ( 'NONE', #17867, 0.1020173459747797384 ) ;
#38895 = ORIENTED_EDGE ( 'NONE', *, *, #29866, .T. ) ;
#38896 = ORIENTED_EDGE ( 'NONE', *, *, #10763, .F. ) ;
#38897 = CARTESIAN_POINT ( 'NONE',  ( -0.01313218671590571027, -0.5535711118707772327, 0.2673923889699659218 ) ) ;
#38899 = DIRECTION ( 'NONE',  ( 0.000000000000000000, 0.000000000000000000, 1.000000000000000000 ) ) ;
#38898 = CARTESIAN_POINT ( 'NONE',  ( 0.01548846960706641053, 0.4730347584886938073, 0.2341461249029914427 ) ) ;
#38900 = CARTESIAN_POINT ( 'NONE',  ( 0.6271571286872942297, -1.601904976971373795, -0.4537812407007095206 ) ) ;
#38901 = DATE_TIME_ROLE ( 'classification_date' ) ;
#38902 = CIRCLE ( 'NONE', #3429, 0.01500000000000006536 ) ;
#38903 = CARTESIAN_POINT ( 'NONE',  ( 0.004891213885548088142, -0.6339827964191876442, 0.1483282180229320291 ) ) ;
#38905 = ORIENTED_EDGE ( 'NONE', *, *, #10188, .F. ) ;
#38904 = ORIENTED_EDGE ( 'NONE', *, *, #20852, .T. ) ;
#38906 = CARTESIAN_POINT ( 'NONE',  ( 0.1548341679632025680, -0.8596504379563697507, 0.5333057515477647170 ) ) ;
#38907 = CARTESIAN_POINT ( 'NONE',  ( 0.06944579691897743989, -0.5431860149686560391, 0.1791531423689709523 ) ) ;
#38908 = CARTESIAN_POINT ( 'NONE',  ( 0.5390157067140883829, -1.519029365507106988, 0.5719888029048197930 ) ) ;
#38909 = DIRECTION ( 'NONE',  ( 1.000000000000000000, -0.000000000000000000, -0.000000000000000000 ) ) ;
#38910 = LINE ( 'NONE', #10738, #35610 ) ;
#38911 = CARTESIAN_POINT ( 'NONE',  ( 0.6413355266909854802, -1.469255435513146413, 0.4003763534992342832 ) ) ;
#38912 = CARTESIAN_POINT ( 'NONE',  ( 0.3478054713553065946, -1.744458529272713498, 0.6010704396163429886 ) ) ;
#38913 = FACE_OUTER_BOUND ( 'NONE', #19605, .T. ) ;
#38914 = CARTESIAN_POINT ( 'NONE',  ( 0.06690744896826546217, -1.340115430975673316, 0.5315786376783453449 ) ) ;
#38915 = DIRECTION ( 'NONE',  ( 0.000000000000000000, 0.4393346272636334260, 0.8983234858819645341 ) ) ;
#38916 = FACE_OUTER_BOUND ( 'NONE', #12394, .T. ) ;
#38917 = CARTESIAN_POINT ( 'NONE',  ( -0.0002454585711109004810, -0.8766763345964988519, -0.01713775608600108177 ) ) ;
#38918 = CARTESIAN_POINT ( 'NONE',  ( 0.2509773515924360043, -0.9519638977167713678, 0.7406622671168548999 ) ) ;
#38919 =( LENGTH_UNIT ( ) NAMED_UNIT ( * ) SI_UNIT ( $, .METRE. ) );
#38920 = VECTOR ( 'NONE', #18025, 39.37007874015748854 ) ;
#38921 = EDGE_CURVE ( 'NONE', #1162, #22334, #35248, .T. ) ;
#38922 = CARTESIAN_POINT ( 'NONE',  ( 0.05999999999999990757, -0.3458405862425447119, -0.1052451372150005060 ) ) ;
#38923 = CARTESIAN_POINT ( 'NONE',  ( 0.6209938526331848507, -1.607187025150189186, -0.4652530029513053389 ) ) ;
#38924 = EDGE_CURVE ( 'NONE', #5913, #17036, #39576, .T. ) ;
#38925 = CARTESIAN_POINT ( 'NONE',  ( 0.007928552535923857544, -0.8847668029847218785, 0.5082548692313750838 ) ) ;
#38926 = CARTESIAN_POINT ( 'NONE',  ( 0.1854168535569867549, -0.8697360073808747538, 0.1457185332388700738 ) ) ;
#38927 = PERSON_AND_ORGANIZATION ( #28500, #32463 ) ;
#38928 = AXIS2_PLACEMENT_3D ( 'NONE', #39094, #20182, #11310 ) ;
#38929 = CARTESIAN_POINT ( 'NONE',  ( 0.5961566725213064410, -1.266700452128206367, 0.8733730542187856383 ) ) ;
#38930 = VECTOR ( 'NONE', #16627, 39.37007874015748143 ) ;
#38931 = CIRCLE ( 'NONE', #36964, 0.02999999999999998501 ) ;
#38932 = CARTESIAN_POINT ( 'NONE',  ( -0.04230188431063486992, 0.4483687697007486817, -0.1365048020681075003 ) ) ;
#38933 = CARTESIAN_POINT ( 'NONE',  ( 0.3136505104175751346, -1.762210813257952147, 0.5687094762557387551 ) ) ;
#38934 = AXIS2_PLACEMENT_3D ( 'NONE', #15958, #38158, #35470 ) ;
#38935 = VERTEX_POINT ( 'NONE', #7707 ) ;
#38936 = CARTESIAN_POINT ( 'NONE',  ( 0.3159174789885340617, -1.473577620167767277, -0.7462941026102613007 ) ) ;
#38937 = CARTESIAN_POINT ( 'NONE',  ( 0.01058516978236496812, -0.5329851777183867156, 0.1813778425092805180 ) ) ;
#38938 = EDGE_CURVE ( 'NONE', #2775, #30856, #1648, .T. ) ;
#38939 = APPROVAL ( #3286, 'UNKNOWN' ) ;
#38940 = CARTESIAN_POINT ( 'NONE',  ( 0.6431982980546400164, -1.414041713902329356, -0.6250000000000000000 ) ) ;
#38941 = ORIENTED_EDGE ( 'NONE', *, *, #18046, .T. ) ;
#38942 = EDGE_CURVE ( 'NONE', #20946, #17780, #5971, .T. ) ;
#38943 = CARTESIAN_POINT ( 'NONE',  ( 0.3395132021710796644, -1.113556448477543981, -0.5155029497116575543 ) ) ;
#38944 = CARTESIAN_POINT ( 'NONE',  ( 0.5969179818652998737, -1.265625243575819514, 0.7915741918176316672 ) ) ;
#38946 = EDGE_LOOP ( 'NONE', ( #4296, #5186, #39182, #7062 ) ) ;
#38945 = EDGE_LOOP ( 'NONE', ( #29198, #15645, #12241, #35771 ) ) ;
#38947 = CARTESIAN_POINT ( 'NONE',  ( 0.001082033974601749821, -1.915745596563056985, -0.6835195572584209511 ) ) ;
#38948 = EDGE_CURVE ( 'NONE', #15927, #38637, #480, .T. ) ;
#38949 = ORIENTED_EDGE ( 'NONE', *, *, #8112, .F. ) ;
#38950 = CARTESIAN_POINT ( 'NONE',  ( 0.1999999999999765299, -2.090543227368257373, -0.6941777981885114412 ) ) ;
#38951 = CARTESIAN_POINT ( 'NONE',  ( 0.4697623592636160361, -1.061459377010899541, -0.6056023639864149821 ) ) ;
#38952 = CIRCLE ( 'NONE', #2170, 0.009999999999999981126 ) ;
#38953 = CARTESIAN_POINT ( 'NONE',  ( -0.05268850283020629077, 0.4471020566665069862, -0.1404229504685556851 ) ) ;
#38954 = ORIENTED_EDGE ( 'NONE', *, *, #38550, .F. ) ;
#38955 = CARTESIAN_POINT ( 'NONE',  ( 0.7429241260303106609, -1.515741207197444984, 0.5682417262808784342 ) ) ;
#38956 = CARTESIAN_POINT ( 'NONE',  ( 0.2162507585142164346, -0.8790159608897792909, 0.6620781576653871348 ) ) ;
#38957 = CIRCLE ( 'NONE', #40280, 0.06000000000000045575 ) ;
#38958 = CARTESIAN_POINT ( 'NONE',  ( 0.2326140044019894271, -1.416031621593191181, 1.021274582455189428 ) ) ;
#38959 = AXIS2_PLACEMENT_3D ( 'NONE', #11021, #11415, #30334 ) ;
#38960 = CARTESIAN_POINT ( 'NONE',  ( 0.4696795125927291092, -1.557974007221949453, 0.5725897366691788948 ) ) ;
#38962 = CARTESIAN_POINT ( 'NONE',  ( 0.2779095291147324343, -1.668760755457822986, 0.5790662758146200018 ) ) ;
#38961 = CARTESIAN_POINT ( 'NONE',  ( 0.1157284135122316898, -1.105864713636613317, 0.8979452765864521790 ) ) ;
#38963 = CARTESIAN_POINT ( 'NONE',  ( 0.05024437483578383934, -0.9472498927431809435, 0.3056578206038833012 ) ) ;
#38964 = ORIENTED_EDGE ( 'NONE', *, *, #1226, .T. ) ;
#38965 = VERTEX_POINT ( 'NONE', #40184 ) ;
#38966 = AXIS2_PLACEMENT_3D ( 'NONE', #36687, #27239, #23742 ) ;
#38967 = DIRECTION ( 'NONE',  ( 1.000000000000000000, 0.000000000000000000, 0.000000000000000000 ) ) ;
#38968 = CARTESIAN_POINT ( 'NONE',  ( 0.1903103077163704193, -0.5412354413273032794, 0.1986930158102075406 ) ) ;
#38969 = CARTESIAN_POINT ( 'NONE',  ( -0.2746410161513779258, -3.253295730098268113, -0.6063490597057096254 ) ) ;
#38970 = CARTESIAN_POINT ( 'NONE',  ( 0.2246635286622190308, -1.191403667735409178, -0.5155029497116575543 ) ) ;
#38971 = EDGE_CURVE ( 'NONE', #26971, #39255, #38410, .T. ) ;
#38972 = ADVANCED_FACE ( 'NONE', ( #24967 ), #27463, .F. ) ;
#38973 = DIRECTION ( 'NONE',  ( -1.000000000000000000, 0.000000000000000000, 0.000000000000000000 ) ) ;
#38974 = DIRECTION ( 'NONE',  ( 0.8660512985181135770, 0.4999551463232368431, 0.000000000000000000 ) ) ;
#38975 = CARTESIAN_POINT ( 'NONE',  ( 0.5468032192656866464, -1.183383020191767443, 0.7376474321803302425 ) ) ;
#38976 = DIRECTION ( 'NONE',  ( -1.473712114141921197E-62, 5.978086547377980088E-31, 1.000000000000000000 ) ) ;
#38977 = CARTESIAN_POINT ( 'NONE',  ( 0.01301404012986586214, -0.8779095112082120345, 0.4619222818525974272 ) ) ;
#38978 = B_SPLINE_CURVE_WITH_KNOTS ( 'NONE', 3,
 ( #36958, #20940, #5877, #8563 ),
 .UNSPECIFIED., .F., .F.,
 ( 4, 4 ),
 ( 0.006562375122924405529, 0.006754369985014277260 ),
 .UNSPECIFIED. ) ;
#38979 = CARTESIAN_POINT ( 'NONE',  ( 0.06646545803895723137, -1.528777460197568328, -0.3435740225710798845 ) ) ;
#38980 = CARTESIAN_POINT ( 'NONE',  ( 0.4885114638772957707, -1.656959017372544807, -0.6069631137146730415 ) ) ;
#38981 = CARTESIAN_POINT ( 'NONE',  ( 0.3889638052529856282, -1.132903526660985705, 0.7528812961574173901 ) ) ;
#38982 = CARTESIAN_POINT ( 'NONE',  ( 0.02869712619511914989, -0.06034133159975874766, 0.4947855140619932257 ) ) ;
#38983 = CARTESIAN_POINT ( 'NONE',  ( -0.05489899477340663692, -0.2510719788555806353, -0.3887182106515197355 ) ) ;
#38984 = CIRCLE ( 'NONE', #22604, 0.1762268159172233339 ) ;
#38985 = AXIS2_PLACEMENT_3D ( 'NONE', #37300, #36699, #36893 ) ;
#38986 = ORIENTED_EDGE ( 'NONE', *, *, #34783, .F. ) ;
#38987 = CARTESIAN_POINT ( 'NONE',  ( 0.5095252007787752779, -1.122954523980121744, 0.6801752979809041477 ) ) ;
#38988 = CARTESIAN_POINT ( 'NONE',  ( 0.08996836131725784169, -0.5655380582595669336, 0.1615303154345441861 ) ) ;
#38989 = CARTESIAN_POINT ( 'NONE',  ( 0.3612374285823241049, -1.754314597143267429, -0.4836476399974993789 ) ) ;
#38990 = CARTESIAN_POINT ( 'NONE',  ( 2.048885995248197414E-16, 0.2900000000000004796, -5.122214988120493288E-16 ) ) ;
#38991 = CIRCLE ( 'NONE', #36350, 0.01000000000000004184 ) ;
#38992 = CARTESIAN_POINT ( 'NONE',  ( 0.2656213591975871147, -1.296266830651302993, 0.6616968573301059697 ) ) ;
#38993 = ORIENTED_EDGE ( 'NONE', *, *, #30119, .T. ) ;
#38994 = DIRECTION ( 'NONE',  ( -0.4999551463232385085, 0.8660512985181127998, 0.000000000000000000 ) ) ;
#38995 = AXIS2_PLACEMENT_3D ( 'NONE', #26192, #10538, #16924 ) ;
#38996 = DIRECTION ( 'NONE',  ( 1.000000000000000000, 2.099003099963413025E-12, -1.419325098918985577E-12 ) ) ;
#38997 = CARTESIAN_POINT ( 'NONE',  ( 0.4751758298663427693, -1.652426242819087010, -0.6334442537810193175 ) ) ;
#38998 = CARTESIAN_POINT ( 'NONE',  ( -0.01548846960707524721, 0.2372406987223596164, -0.4850946823762614102 ) ) ;
#38999 = CARTESIAN_POINT ( 'NONE',  ( 0.4198966019305932496, -1.174027997756919239, 0.7144634253752220054 ) ) ;
#39001 = CARTESIAN_POINT ( 'NONE',  ( 0.4759292920945783489, -1.117238247451545874, 0.5687629415736369376 ) ) ;
#39000 = FACE_BOUND ( 'NONE', #7164, .T. ) ;
#39002 = CARTESIAN_POINT ( 'NONE',  ( 0.5722472701422883778, -1.544651279766090957, -0.4985846812144399398 ) ) ;
#39003 = ORIENTED_EDGE ( 'NONE', *, *, #8114, .F. ) ;
#39004 = LINE ( 'NONE', #8135, #22447 ) ;
#39005 = ORIENTED_EDGE ( 'NONE', *, *, #9431, .F. ) ;
#39006 = CARTESIAN_POINT ( 'NONE',  ( 0.2937365356607388733, -1.300204286310561175, 0.8910421725200852183 ) ) ;
#39008 = CARTESIAN_POINT ( 'NONE',  ( 0.1966785637937622788, -0.7882153485089888889, 0.3097641500712802198 ) ) ;
#39007 = CARTESIAN_POINT ( 'NONE',  ( 0.08738472799975360861, -0.6969953448697594478, 0.001717529511606559391 ) ) ;
#39009 = CARTESIAN_POINT ( 'NONE',  ( 0.1176733790823393522, -1.298938889880303371, 0.5182417262812425429 ) ) ;
#39010 = EDGE_LOOP ( 'NONE', ( #7021, #27033 ) ) ;
#39011 = AXIS2_PLACEMENT_3D ( 'NONE', #22423, #6156, #18720 ) ;
#39012 = CARTESIAN_POINT ( 'NONE',  ( -0.2399999999999999079, -3.647187793141847045, -0.4766722536777797115 ) ) ;
#39013 = CARTESIAN_POINT ( 'NONE',  ( 0.1396989859084467323, -0.6541046724775327892, 0.4283214651078913748 ) ) ;
#39014 = ORIENTED_EDGE ( 'NONE', *, *, #9676, .F. ) ;
#39015 = DIRECTION ( 'NONE',  ( 1.000000000000000000, 0.000000000000000000, 0.000000000000000000 ) ) ;
#39016 = DIRECTION ( 'NONE',  ( 0.000000000000000000, 0.000000000000000000, -1.000000000000000000 ) ) ;
#39017 = AXIS2_PLACEMENT_3D ( 'NONE', #26453, #14099, #29343 ) ;
#39018 = VECTOR ( 'NONE', #5947, 39.37007874015748143 ) ;
#39019 = CARTESIAN_POINT ( 'NONE',  ( 0.6404849885218004690, -1.549707582885980761, 0.4182417262808776903 ) ) ;
#39020 = PRODUCT_DEFINITION_SHAPE ( 'NONE', 'NONE',  #40658 ) ;
#39021 = CARTESIAN_POINT ( 'NONE',  ( 0.2228277390803876379, -1.238373433379782229, 0.4925787018828454711 ) ) ;
#39022 = CARTESIAN_POINT ( 'NONE',  ( 0.3968672699137553161, -1.750153310133208739, -0.5142725273527540830 ) ) ;
#39023 = CARTESIAN_POINT ( 'NONE',  ( 0.02953079040095704308, -0.09152108205201929525, 0.5223162075576431862 ) ) ;
#39024 = CIRCLE ( 'NONE', #19342, 0.1500000000000011324 ) ;
#39025 = CARTESIAN_POINT ( 'NONE',  ( 0.2020777887685438201, -0.5385241820806814239, 0.3979124043150588097 ) ) ;
#39026 = CONICAL_SURFACE ( 'NONE', #33125, 0.1050424246542346202, 1.047197551196599852 ) ;
#39027 = CARTESIAN_POINT ( 'NONE',  ( 0.1424029337235096226, -1.400533250147911746, -0.3552704771134632677 ) ) ;
#39028 = CARTESIAN_POINT ( 'NONE',  ( 0.04230188431063457155, -0.2825024449121523729, -0.3739792551055103331 ) ) ;
#39029 = APPROVAL_STATUS ( 'not_yet_approved' ) ;
#39030 = CARTESIAN_POINT ( 'NONE',  ( 0.6433013898879852421, -1.424917313305586131, -0.6283493189352619135 ) ) ;
#39031 = CARTESIAN_POINT ( 'NONE',  ( 0.1399999999999994582, 7.160938508832261116E-17, 0.2149999999999999967 ) ) ;
#39032 = CARTESIAN_POINT ( 'NONE',  ( -0.1163452666695150850, -0.5320157244525763884, 0.3133290949223796473 ) ) ;
#39033 = CARTESIAN_POINT ( 'NONE',  ( 0.4103535367438664871, -1.245886191849670421, 0.5133467982331404444 ) ) ;
#39034 = CARTESIAN_POINT ( 'NONE',  ( 0.1581650021276234941, -1.285700486175304746, 0.4182417262808776903 ) ) ;
#39035 =( BOUNDED_SURFACE ( )  B_SPLINE_SURFACE ( 3, 2, ( 
 ( #32307, #28641, #19175 ),
 ( #512, #1097, #34791 ),
 ( #6809, #13606, #23079 ),
 ( #19985, #32516, #4338 ),
 ( #16899, #6594, #3534 ),
 ( #16298, #13006, #31926 ),
 ( #28836, #694, #37779 ),
 ( #28128, #184, #37984 ),
 ( #781, #3036, #12676 ),
 ( #24848, #399, #38176 ),
 ( #9794, #34281, #6089 ),
 ( #16194, #9600, #22177 ) ),
 .UNSPECIFIED., .F., .F., .T. ) 
 B_SPLINE_SURFACE_WITH_KNOTS ( ( 4, 2, 2, 2, 2, 4 ),
 ( 3, 3 ),
 ( 0.000000000000000000, 0.0009332466819807876948, 0.001399870022971181488, 0.001866493363961575390, 0.002799740045942362976, 0.003732986727923150779 ),
 ( 0.000000000000000000, 1.000000000000000000 ),
 .UNSPECIFIED. ) 
 GEOMETRIC_REPRESENTATION_ITEM ( )  RATIONAL_B_SPLINE_SURFACE ( (
 ( 1.000000000000000000, 0.8102556146343726784, 1.000000000000000000),
 ( 1.000000000000000000, 0.8006762349670663026, 1.000000000000000000),
 ( 1.000000000000000000, 0.7913450566296021949, 1.000000000000000000),
 ( 1.000000000000000000, 0.7775533969568005910, 1.000000000000000000),
 ( 1.000000000000000000, 0.7729619784068304522, 1.000000000000000000),
 ( 1.000000000000000000, 0.7640664544802193703, 1.000000000000000000),
 ( 1.000000000000000000, 0.7597351442530375643, 1.000000000000000000),
 ( 1.000000000000000000, 0.7469609109291713844, 1.000000000000000000),
 ( 1.000000000000000000, 0.7386488374089775766, 1.000000000000000000),
 ( 1.000000000000000000, 0.7225489873383396100, 1.000000000000000000),
 ( 1.000000000000000000, 0.7144344824572226305, 1.000000000000000000),
 ( 1.000000000000000000, 0.7071067811865492381, 1.000000000000000000) ) ) 
 REPRESENTATION_ITEM ( '' )  SURFACE ( )  );
#39036 = CARTESIAN_POINT ( 'NONE',  ( 0.002392376194700432737, -0.7211561054371403712, 0.3442605867753443794 ) ) ;
#39037 = CARTESIAN_POINT ( 'NONE',  ( 0.5927337715469158663, -1.512431713927492316, -0.6345249349069799205 ) ) ;
#39038 = VECTOR ( 'NONE', #33024, 39.37007874015748854 ) ;
#39039 = DIRECTION ( 'NONE',  ( -0.4999999999999972800, 0.000000000000000000, 0.8660254037844402619 ) ) ;
#39040 = DIRECTION ( 'NONE',  ( 0.000000000000000000, -1.328828465659078041E-14, -1.000000000000000000 ) ) ;
#39041 = CARTESIAN_POINT ( 'NONE',  ( -0.03303708955568371991, -0.3731861634337418354, 0.3634708273687238256 ) ) ;
#39042 = VECTOR ( 'NONE', #30423, 39.37007874015748143 ) ;
#39043 = ORIENTED_EDGE ( 'NONE', *, *, #37914, .T. ) ;
#39044 = AXIS2_PLACEMENT_3D ( 'NONE', #33311, #20177, #7387 ) ;
#39045 = ORIENTED_EDGE ( 'NONE', *, *, #37336, .F. ) ;
#39046 = CARTESIAN_POINT ( 'NONE',  ( 0.4646907997295934845, -1.115905291537239830, 0.5753588453296760719 ) ) ;
#39047 = AXIS2_PLACEMENT_3D ( 'NONE', #22794, #28535, #38595 ) ;
#39048 = CARTESIAN_POINT ( 'NONE',  ( 0.05573493074139709846, -1.335442843293342063, 0.4177417262808780229 ) ) ;
#39049 = ORIENTED_EDGE ( 'NONE', *, *, #25513, .F. ) ;
#39050 = AXIS2_PLACEMENT_3D ( 'NONE', #17718, #11961, #2515 ) ;
#39051 = CARTESIAN_POINT ( 'NONE',  ( -0.1167294259372882170, -0.5331983348239496268, 0.1476740372344552410 ) ) ;
#39052 = CARTESIAN_POINT ( 'NONE',  ( 0.3460467764047484573, -1.678194475986896084, -0.4563891808276777096 ) ) ;
#39053 = CARTESIAN_POINT ( 'NONE',  ( 0.4814929157054633202, -1.267930000418878045, 0.7540278765520666004 ) ) ;
#39055 = VERTEX_POINT ( 'NONE', #36904 ) ;
#39054 = CARTESIAN_POINT ( 'NONE',  ( -0.1583356623530577378, 0.4914777262839040151, 0.1012105261660898592 ) ) ;
#39056 = CARTESIAN_POINT ( 'NONE',  ( 0.5083828713348212958, -1.120917766412646177, 0.6786323191735850191 ) ) ;
#39057 = EDGE_CURVE ( 'NONE', #28442, #11318, #16873, .T. ) ;
#39058 = AXIS2_PLACEMENT_3D ( 'NONE', #33594, #2549, #33207 ) ;
#39059 = DIRECTION ( 'NONE',  ( -1.000000000000000000, -0.000000000000000000, -0.000000000000000000 ) ) ;
#39060 = EDGE_LOOP ( 'NONE', ( #37419, #30234, #10558, #9048, #4519, #9680 ) ) ;
#39061 = CARTESIAN_POINT ( 'NONE',  ( -0.05634304521267748805, 1.092739197465705287E-15, 0.4588823192046724841 ) ) ;
#39062 = ADVANCED_FACE ( 'NONE', ( #8929 ), #39851, .T. ) ;
#39063 = ORIENTED_EDGE ( 'NONE', *, *, #22536, .F. ) ;
#39064 = AXIS2_PLACEMENT_3D ( 'NONE', #13333, #6744, #22408 ) ;
#39065 = CARTESIAN_POINT ( 'NONE',  ( 0.3297717883327160870, -1.638642138455859376, 0.6197557731930207758 ) ) ;
#39067 = CARTESIAN_POINT ( 'NONE',  ( 0.1140740010698196444, -0.5454507455871950850, -0.04915391599425626701 ) ) ;
#39066 = CARTESIAN_POINT ( 'NONE',  ( 0.6621646329316274171, -1.547049793389352557, 0.4306066971441852020 ) ) ;
#39068 = CARTESIAN_POINT ( 'NONE',  ( 0.3210085668004670767, -1.182910313946810010, 0.5197417262808780025 ) ) ;
#39069 = EDGE_CURVE ( 'NONE', #34794, #40356, #21686, .T. ) ;
#39070 = CARTESIAN_POINT ( 'NONE',  ( -2.106084062615542560E-14, -2.087756091470926556, -0.2623975632731757046 ) ) ;
#39071 = ORIENTED_EDGE ( 'NONE', *, *, #7687, .F. ) ;
#39072 = ADVANCED_FACE ( 'NONE', ( #24789 ), #24365, .T. ) ;
#39073 = DIRECTION ( 'NONE',  ( 0.000000000000000000, 0.000000000000000000, -1.000000000000000000 ) ) ;
#39074 = CARTESIAN_POINT ( 'NONE',  ( 0.001120486222623293246, -1.913917409099062272, -0.6537566358931722332 ) ) ;
#39075 = FACE_OUTER_BOUND ( 'NONE', #38581, .T. ) ;
#39076 = CARTESIAN_POINT ( 'NONE',  ( 0.2995545230446825524, -1.131849367291001274, 0.7413806071029465095 ) ) ;
#39077 = CARTESIAN_POINT ( 'NONE',  ( 0.5848508152300195828, -1.486263022089187036, 0.6467108361231791447 ) ) ;
#39078 = VECTOR ( 'NONE', #6375, 39.37007874015748143 ) ;
#39079 = CARTESIAN_POINT ( 'NONE',  ( 0.05283719472145131241, 0.03966590960886431233, -0.4666299489511750997 ) ) ;
#39080 = AXIS2_PLACEMENT_3D ( 'NONE', #12005, #30923, #17970 ) ;
#39081 = AXIS2_PLACEMENT_3D ( 'NONE', #10912, #23479, #33106 ) ;
#39082 = CARTESIAN_POINT ( 'NONE',  ( -0.1710642718812837582, 0.4986889572247744651, 0.3032895567580805585 ) ) ;
#39083 = FACE_OUTER_BOUND ( 'NONE', #17859, .T. ) ;
#39084 = CARTESIAN_POINT ( 'NONE',  ( 0.6295207451518218811, -1.563610154300691502, 0.4182417262808778013 ) ) ;
#39085 = EDGE_CURVE ( 'NONE', #37238, #20093, #40380, .T. ) ;
#39086 = DIRECTION ( 'NONE',  ( 0.000000000000000000, 0.000000000000000000, -1.000000000000000000 ) ) ;
#39087 = CARTESIAN_POINT ( 'NONE',  ( 0.1581650021276240492, -1.285700486175305635, 0.4182417262808778013 ) ) ;
#39088 = COORDINATED_UNIVERSAL_TIME_OFFSET ( 0, 0, .AHEAD. ) ;
#39089 = LOCAL_TIME ( 0, 53, 7.000000000000000000, #1031 ) ;
#39090 = APPROVAL ( #27861, 'UNSPECIFIED' ) ;
#39091 = CARTESIAN_POINT ( 'NONE',  ( 0.3983340929409861508, -1.147351698812145049, 0.4237746715961450694 ) ) ;
#39092 = DIRECTION ( 'NONE',  ( 1.000000000000000000, -0.000000000000000000, -0.000000000000000000 ) ) ;
#39093 = AXIS2_PLACEMENT_3D ( 'NONE', #624, #32230, #4048 ) ;
#39094 = CARTESIAN_POINT ( 'NONE',  ( 0.4315909263077353786, -1.207668101024179430, 0.5182417262812423209 ) ) ;
#39095 = DIRECTION ( 'NONE',  ( 0.000000000000000000, 0.000000000000000000, -1.000000000000000000 ) ) ;
#39096 = CARTESIAN_POINT ( 'NONE',  ( 0.3613982139085152312, -1.770628929897791526, -0.5799859875462475278 ) ) ;
#39097 = CARTESIAN_POINT ( 'NONE',  ( 0.2330432091865630995, -1.417564937792536117, 1.021065090758958238 ) ) ;
#39098 = B_SPLINE_CURVE_WITH_KNOTS ( 'NONE', 3,
 ( #26294, #35533, #28960, #13126, #4467, #10268, #1415, #26498, #13547, #38628, #17227, #16419, #7143, #10648, #35748, #7560, #39033, #824 ),
 .UNSPECIFIED., .F., .F.,
 ( 4, 2, 2, 2, 2, 2, 2, 2, 4 ),
 ( 0.000000000000000000, 0.0003722438250988956946, 0.0007444876501977913891, 0.001116731475296687138, 0.001488975300395582778, 0.001861219125494478419, 0.002233462950593374276, 0.002605706775692269699, 0.002977950600791165556 ),
 .UNSPECIFIED. ) ;
#39099 = CARTESIAN_POINT ( 'NONE',  ( 0.03159140494780060537, -0.05458666898339327445, -0.4890560705835259592 ) ) ;
#39100 = EDGE_LOOP ( 'NONE', ( #13240, #20536, #18938, #13805 ) ) ;
#39101 = ORIENTED_EDGE ( 'NONE', *, *, #29541, .T. ) ;
#39102 = CARTESIAN_POINT ( 'NONE',  ( 0.1744808239353030921, -0.5220121294792338107, 0.1088806183924514309 ) ) ;
#39103 = ORIENTED_EDGE ( 'NONE', *, *, #26822, .T. ) ;
#39104 = CARTESIAN_POINT ( 'NONE',  ( 0.4620955415748976280, -1.655440927177989963, -0.3953929602407867949 ) ) ;
#39105 = CIRCLE ( 'NONE', #3628, 0.01500000000000005843 ) ;
#39106 = CARTESIAN_POINT ( 'NONE',  ( 0.6027238554419750427, -1.482183870088574773, 0.6047563465127264726 ) ) ;
#39108 = EDGE_LOOP ( 'NONE', ( #30568, #5187, #2343, #23082 ) ) ;
#39107 = CARTESIAN_POINT ( 'NONE',  ( 0.006827740514596677447, -0.8142735967992830171, 0.05084675703196275820 ) ) ;
#39109 = CIRCLE ( 'NONE', #26654, 0.01500000000000004802 ) ;
#39110 = ORIENTED_EDGE ( 'NONE', *, *, #18256, .T. ) ;
#39111 = CARTESIAN_POINT ( 'NONE',  ( 0.3204479958614548929, -1.182666560659948907, 0.5682417262808776570 ) ) ;
#39112 = EDGE_CURVE ( 'NONE', #24957, #20339, #21730, .T. ) ;
#39113 = ORIENTED_EDGE ( 'NONE', *, *, #25547, .F. ) ;
#39114 = CARTESIAN_POINT ( 'NONE',  ( 0.2298583264429857054, -1.515562747760924145, 0.9092735558684903463 ) ) ;
#39116 = DIRECTION ( 'NONE',  ( 0.1858595909941346824, 0.1072932506077139692, -0.9767007580674458289 ) ) ;
#39115 = CARTESIAN_POINT ( 'NONE',  ( -0.03158843595483416811, -0.4819971762524441483, -0.09920191295803088005 ) ) ;
#39117 = PRODUCT_DEFINITION_FORMATION_WITH_SPECIFIED_SOURCE ( 'ANY', '', #35054, .NOT_KNOWN. ) ;
#39118 = FACE_OUTER_BOUND ( 'NONE', #31666, .T. ) ;
#39119 = CALENDAR_DATE ( 2026, 13, 10 ) ;
#39120 = EDGE_CURVE ( 'NONE', #25611, #1427, #8955, .T. ) ;
#39121 = CARTESIAN_POINT ( 'NONE',  ( -0.0003981105962839171755, -0.8469330747986117958, -0.1178596299512797430 ) ) ;
#39123 = ORIENTED_EDGE ( 'NONE', *, *, #15523, .T. ) ;
#39122 = ORIENTED_EDGE ( 'NONE', *, *, #32847, .F. ) ;
#39124 = EDGE_CURVE ( 'NONE', #24171, #3794, #1147, .T. ) ;
#39125 = CARTESIAN_POINT ( 'NONE',  ( 0.08591970961800117490, -0.7898962715215620545, 0.1943287141640972771 ) ) ;
#39126 = AXIS2_PLACEMENT_3D ( 'NONE', #10698, #35200, #22877 ) ;
#39127 = CARTESIAN_POINT ( 'NONE',  ( 0.06088048528104925139, -1.075208222708675887, 0.7418958488900205817 ) ) ;
#39128 = CARTESIAN_POINT ( 'NONE',  ( 0.1312574532462938703, -0.6907975637544085945, 0.4921479965689204983 ) ) ;
#39129 = CARTESIAN_POINT ( 'NONE',  ( 0.1758720408525228374, -0.7793959872790835464, 0.5981583825683202127 ) ) ;
#39130 = CARTESIAN_POINT ( 'NONE',  ( 0.06841984176915458238, -1.324714172852429650, 0.5852474161806638930 ) ) ;
#39131 = DIRECTION ( 'NONE',  ( -8.881784197001246407E-16, 2.361472542561082612E-16, -1.000000000000000000 ) ) ;
#39132 = CARTESIAN_POINT ( 'NONE',  ( 0.6508782539171524828, -1.549424043532367179, 0.4232305864574226750 ) ) ;
#39133 = CARTESIAN_POINT ( 'NONE',  ( -0.2399999999999999079, -3.068736697824639759, 0.08412833800243627036 ) ) ;
#39134 = DIRECTION ( 'NONE',  ( 1.000000000000000000, 7.857794173099924470E-32, 8.628166150854818811E-32 ) ) ;
#39135 = DIRECTION ( 'NONE',  ( -0.4261641068392685860, 0.000000000000000000, 0.9046458721742383080 ) ) ;
#39136 = DIRECTION ( 'NONE',  ( 0.02743089364023493237, 0.02297375779311301713, -0.9993596712530287141 ) ) ;
#39137 = FACE_OUTER_BOUND ( 'NONE', #33204, .T. ) ;
#39138 = CARTESIAN_POINT ( 'NONE',  ( 0.01159392866623401054, -0.8181752906802141068, -0.07781262754897533274 ) ) ;
#39139 = EDGE_CURVE ( 'NONE', #34573, #8954, #6989, .T. ) ;
#39140 = DIRECTION ( 'NONE',  ( 0.4999551463232373427, -0.8660512985181134660, 0.000000000000000000 ) ) ;
#39141 = CARTESIAN_POINT ( 'NONE',  ( 0.007159747793320437280, -0.7917788012823626653, 0.02659789922158702774 ) ) ;
#39142 = VECTOR ( 'NONE', #19491, 39.37007874015748143 ) ;
#39143 = CIRCLE ( 'NONE', #5621, 0.08000000000000000167 ) ;
#39144 = CARTESIAN_POINT ( 'NONE',  ( -0.2746410161513779258, -1.804235510932644004, -0.05018601889714981862 ) ) ;
#39145 = CARTESIAN_POINT ( 'NONE',  ( 0.03167879690716527558, -0.8799939210571326997, 0.6541495583543271986 ) ) ;
#39146 = CARTESIAN_POINT ( 'NONE',  ( 0.2317493251130877951, -0.9016848682509819302, 0.4453502113744062241 ) ) ;
#39147 = CALENDAR_DATE ( 2026, 13, 10 ) ;
#39148 = CARTESIAN_POINT ( 'NONE',  ( 0.6320591615222423965, -1.324690328322339239, 0.8595101463142521547 ) ) ;
#39149 = PRODUCT_DEFINITION_FORMATION_WITH_SPECIFIED_SOURCE ( 'ANY', '', #4853, .NOT_KNOWN. ) ;
#39150 = CARTESIAN_POINT ( 'NONE',  ( 0.4038123414656494270, -1.648191853347414693, -0.6342846586131767328 ) ) ;
#39151 = AXIS2_PLACEMENT_3D ( 'NONE', #17171, #36288, #20467 ) ;
#39152 = CARTESIAN_POINT ( 'NONE',  ( 0.3110204894824479260, -1.761578038038337235, 0.5680195786030766136 ) ) ;
#39153 = ORIENTED_EDGE ( 'NONE', *, *, #6663, .F. ) ;
#39154 = CARTESIAN_POINT ( 'NONE',  ( -0.2666757540196700305, 0.4921670437878979398, 0.09999999999999879818 ) ) ;
#39155 = CARTESIAN_POINT ( 'NONE',  ( 0.04534555968120922154, -0.8363173250083066890, 0.7068803008767403639 ) ) ;
#39156 = CARTESIAN_POINT ( 'NONE',  ( 0.2089288257737619836, -1.288245670442317525, -0.6300528582021277524 ) ) ;
#39158 = ORIENTED_EDGE ( 'NONE', *, *, #6617, .F. ) ;
#39157 = CARTESIAN_POINT ( 'NONE',  ( 0.3949726910288821058, -1.765807112359412567, -0.5057413602038844935 ) ) ;
#39159 = CARTESIAN_POINT ( 'NONE',  ( -0.2399999999999999079, -3.941790907013290823, -0.4709369376873030477 ) ) ;
#39160 = CARTESIAN_POINT ( 'NONE',  ( 0.5799898087634006716, -1.239070881731211049, 0.8001874111395332889 ) ) ;
#39162 = ORIENTED_EDGE ( 'NONE', *, *, #16565, .F. ) ;
#39161 = EDGE_LOOP ( 'NONE', ( #605, #22907, #22440, #5560 ) ) ;
#39163 = CARTESIAN_POINT ( 'NONE',  ( 0.03311111702111442512, -1.809660005586617437, -0.6723719395828864354 ) ) ;
#39164 = ADVANCED_FACE ( 'NONE', ( #3961 ), #31318, .T. ) ;
#39165 = ORIENTED_EDGE ( 'NONE', *, *, #20057, .T. ) ;
#39166 = VERTEX_POINT ( 'NONE', #3351 ) ;
#39167 = DIRECTION ( 'NONE',  ( 0.000000000000000000, 0.000000000000000000, -1.000000000000000000 ) ) ;
#39168 = CARTESIAN_POINT ( 'NONE',  ( 0.4389213214516935468, -1.229316516391377956, 0.5870219547771845514 ) ) ;
#39169 = EDGE_CURVE ( 'NONE', #799, #13526, #39820, .T. ) ;
#39170 = CARTESIAN_POINT ( 'NONE',  ( -0.04087116408466956452, 0.4416914123362159494, -0.1656680454788639623 ) ) ;
#39171 = ORIENTED_EDGE ( 'NONE', *, *, #22553, .F. ) ;
#39172 = CARTESIAN_POINT ( 'NONE',  ( 0.1260557303073279456, -1.253941604664451592, 0.6054858248391781217 ) ) ;
#39173 = CIRCLE ( 'NONE', #3061, 0.03999999999999950817 ) ;
#39174 = CARTESIAN_POINT ( 'NONE',  ( 0.08875147084456939950, -0.6445117467991265947, 0.1457185332388690746 ) ) ;
#39175 = CARTESIAN_POINT ( 'NONE',  ( 0.2149123625260831172, -1.353071881634811735, 1.025762950587601807 ) ) ;
#39176 = CARTESIAN_POINT ( 'NONE',  ( 0.4696012870462846767, -1.557946535618014661, 0.5713013830897200052 ) ) ;
#39178 = CARTESIAN_POINT ( 'NONE',  ( 0.3222894045021684195, -1.758215778056678724, 0.5682417262808792113 ) ) ;
#39177 = CARTESIAN_POINT ( 'NONE',  ( 0.2646723247128293655, -1.687375416948911244, 0.5682417262808783232 ) ) ;
#39179 = CARTESIAN_POINT ( 'NONE',  ( 0.04687500000000017347, -0.9399235171994243521, 0.1457185332388702959 ) ) ;
#39180 = APPLIED_SECURITY_CLASSIFICATION_ASSIGNMENT ( #28638, ( #40650 ) ) ;
#39181 = EDGE_LOOP ( 'NONE', ( #5713, #27011, #11117, #26467 ) ) ;
#39182 = ORIENTED_EDGE ( 'NONE', *, *, #32557, .F. ) ;
#39183 = CARTESIAN_POINT ( 'NONE',  ( 0.1499999999999996336, 0.09061086148575973886, 0.5171215251571029681 ) ) ;
#39184 = CARTESIAN_POINT ( 'NONE',  ( 0.1919946538045175233, -0.5556448844311334678, 0.2441157438994971951 ) ) ;
#39185 = AXIS2_PLACEMENT_3D ( 'NONE', #22118, #9936, #38116 ) ;
#39186 = DIRECTION ( 'NONE',  ( 0.000000000000000000, 0.000000000000000000, -1.000000000000000000 ) ) ;
#39187 = CARTESIAN_POINT ( 'NONE',  ( -0.04308745346420585209, -0.4845670975328188468, -0.09763449863321065070 ) ) ;
#39188 = ADVANCED_FACE ( 'NONE', ( #25398 ), #19008, .F. ) ;
#39189 = CARTESIAN_POINT ( 'NONE',  ( -0.08000000000000000167, -1.599201040860868339, 0.1642182323853691728 ) ) ;
#39190 = EDGE_CURVE ( 'NONE', #12319, #22735, #22113, .T. ) ;
#39191 = CYLINDRICAL_SURFACE ( 'NONE', #20529, 0.1946589359789743512 ) ;
#39192 = CARTESIAN_POINT ( 'NONE',  ( 0.5847200959167868639, -1.241056950120674518, 0.7055318339491533086 ) ) ;
#39193 = EDGE_CURVE ( 'NONE', #37380, #12338, #4340, .T. ) ;
#39194 = CARTESIAN_POINT ( 'NONE',  ( -0.1142976700078457836, -0.5226524673290442458, 0.1219895833617486020 ) ) ;
#39195 = CARTESIAN_POINT ( 'NONE',  ( 0.02999778723028691946, -2.087755359801442445, -0.2623954751430958021 ) ) ;
#39196 = CONICAL_SURFACE ( 'NONE', #31967, 0.04999999999999888561, 1.047197551196599630 ) ;
#39197 = CARTESIAN_POINT ( 'NONE',  ( 0.5360167750696916977, -1.632603989559125557, -0.5957800154415829885 ) ) ;
#39198 = ORIENTED_EDGE ( 'NONE', *, *, #38890, .T. ) ;
#39199 = DIRECTION ( 'NONE',  ( 2.686534417925915961E-31, -0.5877852522924640333, 0.8090169943749540016 ) ) ;
#39200 = PLANE ( 'NONE',  #889 ) ;
#39201 = CARTESIAN_POINT ( 'NONE',  ( -0.01899468245562016197, -0.2428515268394236259, -0.4597785848521230290 ) ) ;
#39202 = APPLIED_APPROVAL_ASSIGNMENT ( #4473, ( #38548 ) ) ;
#39203 = ORIENTED_EDGE ( 'NONE', *, *, #9000, .F. ) ;
#39204 = CARTESIAN_POINT ( 'NONE',  ( 0.4804449940050610768, -1.088495069837083662, 0.7089115947332130796 ) ) ;
#39205 = DIRECTION ( 'NONE',  ( 1.000000000000000000, 0.000000000000000000, 0.000000000000000000 ) ) ;
#39206 = CARTESIAN_POINT ( 'NONE',  ( 0.2859919059094789273, -1.317642033747133734, -0.5155029497116575543 ) ) ;
#39207 = AXIS2_PLACEMENT_3D ( 'NONE', #28341, #26476, #33042 ) ;
#39208 = CARTESIAN_POINT ( 'NONE',  ( 0.1854929114990819528, -1.130708035657951305, 0.7521778099971917486 ) ) ;
#39209 = EDGE_LOOP ( 'NONE', ( #20814, #5999, #18671, #4451, #36913, #27542, #34486 ) ) ;
#39210 = CARTESIAN_POINT ( 'NONE',  ( 0.04582889109739184119, 0.2312034125369037685, 0.4285435303321080691 ) ) ;
#39211 = DIRECTION ( 'NONE',  ( 0.000000000000000000, 0.000000000000000000, 1.000000000000000000 ) ) ;
#39212 = CARTESIAN_POINT ( 'NONE',  ( 0.3771322225225746672, -1.765190303781668968, -0.4446624772603183229 ) ) ;
#39213 = CARTESIAN_POINT ( 'NONE',  ( 0.3969700875656382300, -1.750093955434189663, -0.5306525527942058673 ) ) ;
#39214 = CARTESIAN_POINT ( 'NONE',  ( 0.4639714015768776623, -1.230980424943016516, 0.6209263965717269906 ) ) ;
#39215 = ADVANCED_FACE ( 'NONE', ( #22307 ), #30638, .T. ) ;
#39217 = CARTESIAN_POINT ( 'NONE',  ( 0.3563380670180646970, -1.791703161805209277, -0.4886643292207938361 ) ) ;
#39216 = FACE_BOUND ( 'NONE', #14011, .T. ) ;
#39218 = CARTESIAN_POINT ( 'NONE',  ( 0.2448569360945407336, -0.9465973144586597998, 0.4687868266098103587 ) ) ;
#39219 = EDGE_LOOP ( 'NONE', ( #34834, #11123, #30102, #2668 ) ) ;
#39220 = EDGE_CURVE ( 'NONE', #4891, #27130, #37212, .T. ) ;
#39221 = CARTESIAN_POINT ( 'NONE',  ( -0.02000000000000000042, -2.626773565144302935, -0.2726934094652516127 ) ) ;
#39222 = ORIENTED_EDGE ( 'NONE', *, *, #14046, .T. ) ;
#39223 = DIRECTION ( 'NONE',  ( 0.000000000000000000, 0.000000000000000000, -1.000000000000000000 ) ) ;
#39224 = CARTESIAN_POINT ( 'NONE',  ( 0.4045308282536131950, -1.554303138208902757, 0.7579804941832600784 ) ) ;
#39226 = CARTESIAN_POINT ( 'NONE',  ( -1.502516396515344672E-15, -0.3899999999999999578, 5.463695987328526437E-16 ) ) ;
#39225 = CARTESIAN_POINT ( 'NONE',  ( 0.08904850043071313448, -0.5718714707336374214, 0.05944887859078885201 ) ) ;
#39227 = CARTESIAN_POINT ( 'NONE',  ( 0.1185312037127926460, -1.298473412180007669, 0.5084237371918658432 ) ) ;
#39228 = ORIENTED_EDGE ( 'NONE', *, *, #38540, .F. ) ;
#39229 = VECTOR ( 'NONE', #24581, 39.37007874015748143 ) ;
#39230 = CARTESIAN_POINT ( 'NONE',  ( -2.112273405726188513E-14, -2.183180860297921466, -0.4937760292030871079 ) ) ;
#39231 = CARTESIAN_POINT ( 'NONE',  ( 0.4167025260715199186, -1.244396403474990809, 0.8329684759543855010 ) ) ;
#39232 = ORIENTED_EDGE ( 'NONE', *, *, #7717, .F. ) ;
#39233 = CARTESIAN_POINT ( 'NONE',  ( 0.6342910143488530439, -1.590277009563203503, 0.6099924316480835884 ) ) ;
#39234 = CARTESIAN_POINT ( 'NONE',  ( 0.03674078017396374685, -0.4681991728402142283, 0.1092756390057521149 ) ) ;
#39235 = CARTESIAN_POINT ( 'NONE',  ( 0.4242133616548363628, -1.734366925052854391, -0.4397180493288433967 ) ) ;
#39236 = CARTESIAN_POINT ( 'NONE',  ( 0.1521839796440336845, -1.267694068221620896, 0.4309206314624388079 ) ) ;
#39237 = LINE ( 'NONE', #32652, #4924 ) ;
#39238 = CARTESIAN_POINT ( 'NONE',  ( 0.6998761188508713094, -1.434392152549301747, 0.7385670194571644087 ) ) ;
#39239 = DIRECTION ( 'NONE',  ( 0.4999999999999974465, -0.4440468346413919409, -0.7435202812600089084 ) ) ;
#39240 = CARTESIAN_POINT ( 'NONE',  ( 0.04229956186878609803, -0.2683474741743136494, -0.3842687663629391626 ) ) ;
#39241 = CARTESIAN_POINT ( 'NONE',  ( 0.6284115775016231309, -1.542760345567441460, -0.6058523010359371241 ) ) ;
#39242 = FACE_OUTER_BOUND ( 'NONE', #32071, .T. ) ;
#39243 = CARTESIAN_POINT ( 'NONE',  ( 0.1842078230746693746, -0.5805659298032126436, 0.0009058688700998594528 ) ) ;
#39244 = DIRECTION ( 'NONE',  ( 1.000000000000000000, 0.000000000000000000, 0.000000000000000000 ) ) ;
#39245 = CARTESIAN_POINT ( 'NONE',  ( -0.05561176441985838520, 0.4442366066780379374, -0.1229089882096660452 ) ) ;
#39246 = CARTESIAN_POINT ( 'NONE',  ( 0.09104835764951833832, -0.9296025949902090302, 0.8700335549320106221 ) ) ;
#39247 = CARTESIAN_POINT ( 'NONE',  ( 0.5867991090592019621, -1.567604868959546760, -0.5372565133074018728 ) ) ;
#39248 = CARTESIAN_POINT ( 'NONE',  ( 0.02999999999910716447, -2.094379624028320563, -0.2600525928522836039 ) ) ;
#39249 = CARTESIAN_POINT ( 'NONE',  ( -0.02000000000000000042, -2.022243545323729741, -0.2876084842891860061 ) ) ;
#39250 = CARTESIAN_POINT ( 'NONE',  ( -0.04574984450155204774, -0.3363984555176520175, 0.3523422282978331266 ) ) ;
#39251 = ORIENTED_EDGE ( 'NONE', *, *, #7418, .F. ) ;
#39252 = ORIENTED_EDGE ( 'NONE', *, *, #2946, .T. ) ;
#39253 = CARTESIAN_POINT ( 'NONE',  ( 0.6179330812053925870, -1.625469311300162811, 0.5182417262812423209 ) ) ;
#39254 = CARTESIAN_POINT ( 'NONE',  ( 0.3210085668004670767, -1.182910313946810010, 0.5197417262808780025 ) ) ;
#39255 = VERTEX_POINT ( 'NONE', #7051 ) ;
#39256 = DIRECTION ( 'NONE',  ( 1.386669559958804888E-32, 0.8983234858819696411, 0.4393346272636231564 ) ) ;
#39257 = CARTESIAN_POINT ( 'NONE',  ( 0.02238826743733597635, 0.2417677220642130975, -0.4518145715460058498 ) ) ;
#39258 = CARTESIAN_POINT ( 'NONE',  ( 0.5269365913707252380, -1.338824413986121842, 0.7108823065707898792 ) ) ;
#39260 = VERTEX_POINT ( 'NONE', #12614 ) ;
#39259 = CARTESIAN_POINT ( 'NONE',  ( -0.1621871387067581605, 0.5037941088976199966, 0.1094562450723028518 ) ) ;
#39261 = CARTESIAN_POINT ( 'NONE',  ( 0.2858575041057334065, -0.8891697324286316206, 0.5691962326423758434 ) ) ;
#39262 = VECTOR ( 'NONE', #25517, 39.37007874015748143 ) ;
#39263 = CARTESIAN_POINT ( 'NONE',  ( 0.05083665881509014800, 0.4630607685881601987, -0.09936361682460806422 ) ) ;
#39264 = ORIENTED_EDGE ( 'NONE', *, *, #1206, .T. ) ;
#39265 = CARTESIAN_POINT ( 'NONE',  ( 0.01548846960706664298, -0.2306506793134169842, -0.4716198300880524719 ) ) ;
#39266 = CARTESIAN_POINT ( 'NONE',  ( 0.3270478934205144350, -1.639199132634546086, 0.5744591934003364653 ) ) ;
#39268 = DIRECTION ( 'NONE',  ( 0.4999551463232373427, -0.8660512985181134660, 0.000000000000000000 ) ) ;
#39267 = CARTESIAN_POINT ( 'NONE',  ( 0.7067742920676829410, -1.507341406312437293, 0.5470997294487818241 ) ) ;
#39269 = LINE ( 'NONE', #30205, #5002 ) ;
#39270 = CARTESIAN_POINT ( 'NONE',  ( 0.1999999999999781675, -2.107936428766273629, -0.7005084057759864979 ) ) ;
#39271 = ORIENTED_EDGE ( 'NONE', *, *, #10924, .T. ) ;
#39272 = DIRECTION ( 'NONE',  ( 0.000000000000000000, 0.000000000000000000, -1.000000000000000000 ) ) ;
#39273 = CARTESIAN_POINT ( 'NONE',  ( 0.1548759089261008415, -1.279768374172244316, 0.4182417262808777458 ) ) ;
#39274 = CARTESIAN_POINT ( 'NONE',  ( 0.03159140494780057068, 0.4819881711443544936, 0.09921162977303653319 ) ) ;
#39275 = CARTESIAN_POINT ( 'NONE',  ( 0.3303989628691124114, -1.288507568649391866, 0.5994241297422728820 ) ) ;
#39276 = CARTESIAN_POINT ( 'NONE',  ( -0.1574377185082707353, 0.4885537809602767401, 0.1000000000000000194 ) ) ;
#39277 = CARTESIAN_POINT ( 'NONE',  ( -0.02000000000000000042, -2.332630956013932888, -0.5701767140373721343 ) ) ;
#39278 = ADVANCED_BREP_SHAPE_REPRESENTATION ( '', ( #18583, #27819 ), #21247 ) ;
#39279 = CARTESIAN_POINT ( 'NONE',  ( 0.3422841821767727000, -1.070812901706339693, 0.6386172016438887988 ) ) ;
#39280 = CARTESIAN_POINT ( 'NONE',  ( -0.08000000000000000167, -1.845925619402022155, -0.3444148183989317880 ) ) ;
#39281 =( BOUNDED_SURFACE ( )  B_SPLINE_SURFACE ( 3, 2, ( 
 ( #17821, #36558, #32844 ),
 ( #4861, #8365, #36137 ),
 ( #5263, #33656, #5469 ),
 ( #24223, #21129, #20934 ) ),
 .UNSPECIFIED., .F., .F., .F. ) 
 B_SPLINE_SURFACE_WITH_KNOTS ( ( 4, 4 ),
 ( 3, 3 ),
 ( -8.890457814381136359E-18, 0.0004170061191612176076 ),
 ( 0.000000000000000000, 1.000000000000000000 ),
 .UNSPECIFIED. ) 
 GEOMETRIC_REPRESENTATION_ITEM ( )  RATIONAL_B_SPLINE_SURFACE ( (
 ( 1.000000000000000000, 0.8864945003983012439, 1.000000000000000000),
 ( 1.000000000000000000, 0.8852517754806471517, 1.000000000000000000),
 ( 1.000000000000000000, 0.8837135633426822512, 1.000000000000000000),
 ( 1.000000000000000000, 0.8817574585067771142, 1.000000000000000000) ) ) 
 REPRESENTATION_ITEM ( '' )  SURFACE ( )  );
#39282 = CARTESIAN_POINT ( 'NONE',  ( 0.03654364704248852513, 0.4542255574219836167, 0.2354487068768196523 ) ) ;
#39283 = CARTESIAN_POINT ( 'NONE',  ( 0.6499222637756963961, -1.534002237024607584, 0.4182417262808776903 ) ) ;
#39284 = CARTESIAN_POINT ( 'NONE',  ( 0.2821932362258575688, -1.666110558802125441, 0.4618966104728081667 ) ) ;
#39285 = COORDINATED_UNIVERSAL_TIME_OFFSET ( 0, 0, .AHEAD. ) ;
#39286 = CARTESIAN_POINT ( 'NONE',  ( 0.4108854627016636507, -1.135744711144478503, 0.4324876386359573499 ) ) ;
#39287 = CARTESIAN_POINT ( 'NONE',  ( 0.1909286924077255310, -1.257064795538239022, -0.3864493710799625781 ) ) ;
#39288 = AXIS2_PLACEMENT_3D ( 'NONE', #29096, #15946, #22150 ) ;
#39289 = PRODUCT_DEFINITION_CONTEXT ( 'detailed design', #39759, 'design' ) ;
#39290 = CYLINDRICAL_SURFACE ( 'NONE', #38928, 0.03749999999977551152 ) ;
#39291 = FACE_OUTER_BOUND ( 'NONE', #11277, .T. ) ;
#39292 = CARTESIAN_POINT ( 'NONE',  ( 0.4578538094500779754, -1.109988817041876352, 0.5689675956757063169 ) ) ;
#39293 = CARTESIAN_POINT ( 'NONE',  ( 0.2153927220196321379, -1.354775012865835349, 1.025737857953066712 ) ) ;
#39294 = EDGE_CURVE ( 'NONE', #28758, #39975, #19483, .T. ) ;
#39295 = CARTESIAN_POINT ( 'NONE',  ( 0.5264113014007612001, -1.640729993778266893, -0.5166151207188711680 ) ) ;
#39296 = EDGE_CURVE ( 'NONE', #34573, #12958, #32596, .T. ) ;
#39297 = ORIENTED_EDGE ( 'NONE', *, *, #7725, .T. ) ;
#39298 = ORIENTED_EDGE ( 'NONE', *, *, #10922, .T. ) ;
#39299 = LINE ( 'NONE', #11119, #33506 ) ;
#39300 = ORIENTED_EDGE ( 'NONE', *, *, #5436, .F. ) ;
#39301 = DIRECTION ( 'NONE',  ( -0.4999999999999986677, 0.4122333455936965096, -0.7616191100416460635 ) ) ;
#39302 = CARTESIAN_POINT ( 'NONE',  ( 0.1344514937509518615, -0.5566420558580671418, 0.1875615093596288141 ) ) ;
#39304 = ORIENTED_EDGE ( 'NONE', *, *, #11512, .T. ) ;
#39303 = CARTESIAN_POINT ( 'NONE',  ( -0.0008048508911302323975, -0.7725538104732808664, 0.0005696801228754680814 ) ) ;
#39305 = ORIENTED_EDGE ( 'NONE', *, *, #13191, .F. ) ;
#39306 = CARTESIAN_POINT ( 'NONE',  ( 0.3382129488829186403, -0.9467566114000368627, 0.8359658843758493996 ) ) ;
#39307 = EDGE_CURVE ( 'NONE', #13712, #22389, #3714, .T. ) ;
#39308 = CARTESIAN_POINT ( 'NONE',  ( -0.01330129037024533299, -0.5512292143768563468, 0.2608376860888254600 ) ) ;
#39310 = CARTESIAN_POINT ( 'NONE',  ( 0.1723747331277147021, -1.257869073915691915, 0.6009879486010095695 ) ) ;
#39309 = CARTESIAN_POINT ( 'NONE',  ( -0.03159140494780089681, -0.4482517543799761084, -0.2030416442520474596 ) ) ;
#39311 = APPLIED_PERSON_AND_ORGANIZATION_ASSIGNMENT ( #26998, #32753, ( #9542 ) ) ;
#39312 = CARTESIAN_POINT ( 'NONE',  ( 0.6410892975813305972, -1.609168521141159047, -0.4443638777805624662 ) ) ;
#39313 = CALENDAR_DATE ( 2026, 13, 10 ) ;
#39314 = LINE ( 'NONE', #36638, #15238 ) ;
#39316 = EDGE_LOOP ( 'NONE', ( #1538, #26742, #19894, #26780, #15678, #12197, #19234, #2540 ) ) ;
#39315 = ORIENTED_EDGE ( 'NONE', *, *, #32187, .T. ) ;
#39317 = CARTESIAN_POINT ( 'NONE',  ( 0.2071075748763558100, -0.9148240409056219713, 0.6263237739596859699 ) ) ;
#39318 = CYLINDRICAL_SURFACE ( 'NONE', #12239, 0.1620173459747806799 ) ;
#39319 = CARTESIAN_POINT ( 'NONE',  ( 0.1134335511682827979, -0.6991477288424914338, 0.5114506147767768907 ) ) ;
#39320 = CARTESIAN_POINT ( 'NONE',  ( 0.4972768597348715680, -1.421470149658270898, 0.7931024745911073870 ) ) ;
#39321 = CARTESIAN_POINT ( 'NONE',  ( 0.02122736906704300250, -1.007833681744604748, 0.5273104902783299908 ) ) ;
#39322 = DIRECTION ( 'NONE',  ( -1.000000000000000000, -1.450080480853946466E-15, 8.188689774234050758E-16 ) ) ;
#39323 = CARTESIAN_POINT ( 'NONE',  ( 0.1849096901904443147, -1.549205955729533235, 0.5682417262808779901 ) ) ;
#39324 = LINE ( 'NONE', #39133, #33159 ) ;
#39325 = CARTESIAN_POINT ( 'NONE',  ( 0.4039575731531036551, -1.662086776922496734, -0.3578710663349294330 ) ) ;
#39326 = DIRECTION ( 'NONE',  ( 0.01455087615875037474, 0.9998941303973200023, 0.000000000000000000 ) ) ;
#39327 = DIRECTION ( 'NONE',  ( 0.000000000000000000, 0.3420201433256707668, 0.9396926207859077618 ) ) ;
#39328 = DIRECTION ( 'NONE',  ( -1.000000000000000000, -6.779273404243070203E-32, -4.314083075427407763E-32 ) ) ;
#39329 = CARTESIAN_POINT ( 'NONE',  ( 0.4690998592273773471, -1.116607765959707343, 0.5684169780556365126 ) ) ;
#39330 = CARTESIAN_POINT ( 'NONE',  ( 0.3837623509413576883, -1.658427931343763762, -0.4031416779713772325 ) ) ;
#39331 = LENGTH_MEASURE_WITH_UNIT ( LENGTH_MEASURE( 0.02539999999999999897 ), #29884 );
#39332 = CARTESIAN_POINT ( 'NONE',  ( -0.08000000000000000167, -2.070343076906777213, -0.2454056712452573896 ) ) ;
#39333 = ADVANCED_FACE ( 'NONE', ( #3775 ), #32154, .F. ) ;
#39334 = CARTESIAN_POINT ( 'NONE',  ( 0.006982617232424345385, -0.7536834681452820872, 0.4384055362127323718 ) ) ;
#39335 = CARTESIAN_POINT ( 'NONE',  ( 0.4216623502531439693, -1.034931331451964143, 0.6525378447207771382 ) ) ;
#39336 = EDGE_CURVE ( 'NONE', #24285, #3165, #33268, .T. ) ;
#39337 = PERSON_AND_ORGANIZATION ( #28500, #32463 ) ;
#39338 = CARTESIAN_POINT ( 'NONE',  ( 0.3173647091058168779, -0.7919842589448738979, 0.7159411547141941723 ) ) ;
#39339 = EDGE_CURVE ( 'NONE', #36294, #26509, #38320, .T. ) ;
#39340 = EDGE_CURVE ( 'NONE', #29449, #29150, #16273, .T. ) ;
#39341 = CARTESIAN_POINT ( 'NONE',  ( -0.02000000000000000042, -2.551729310907437043, -0.5086726180052709712 ) ) ;
#39342 = ADVANCED_FACE ( 'NONE', ( #18948 ), #3105, .F. ) ;
#39343 = CARTESIAN_POINT ( 'NONE',  ( -0.01210526301015805301, 0.06117178301711216626, -0.1249999999999999029 ) ) ;
#39344 = VERTEX_POINT ( 'NONE', #15648 ) ;
#39345 = CARTESIAN_POINT ( 'NONE',  ( 0.4697228370620195048, -1.442521976758482261, -0.5166151207188711680 ) ) ;
#39346 = CARTESIAN_POINT ( 'NONE',  ( 0.1514923887095717958, -1.230592969833345540, 0.9376751449580931208 ) ) ;
#39347 = CARTESIAN_POINT ( 'NONE',  ( 0.1577606996786170002, -1.264465854478742157, 0.4314197961377732038 ) ) ;
#39349 = ORIENTED_EDGE ( 'NONE', *, *, #2712, .F. ) ;
#39348 = CARTESIAN_POINT ( 'NONE',  ( 0.3892111963516278195, -1.924636834596797463, -0.5051628067631914742 ) ) ;
#39350 = CARTESIAN_POINT ( 'NONE',  ( 0.5362507510587237736, -1.657686573918387252, -0.4612641151860342181 ) ) ;
#39351 = CARTESIAN_POINT ( 'NONE',  ( 0.2019795930595086331, -0.6216091269244319317, 0.3384082674912240463 ) ) ;
#39353 = ORIENTED_EDGE ( 'NONE', *, *, #27805, .F. ) ;
#39352 = EDGE_LOOP ( 'NONE', ( #35606, #26090, #35728, #1338 ) ) ;
#39354 = CARTESIAN_POINT ( 'NONE',  ( 0.02991800254585390284, -1.951451259341335343, -0.6900850705760112058 ) ) ;
#39355 = ORIENTED_EDGE ( 'NONE', *, *, #32264, .F. ) ;
#39356 = CARTESIAN_POINT ( 'NONE',  ( 0.1399999999999994582, 0.000000000000000000, 0.000000000000000000 ) ) ;
#39357 = ADVANCED_FACE ( 'NONE', ( #24722 ), #11162, .T. ) ;
#39358 = PRODUCT ( 'Top Pivot Bracket', 'Top Pivot Bracket', '', ( #31427 ) ) ;
#39359 = CARTESIAN_POINT ( 'NONE',  ( -0.1499999999999996336, -2.632527843410151989E-17, -0.1250000000000000000 ) ) ;
#39360 = CALENDAR_DATE ( 2026, 13, 10 ) ;
#39361 = CARTESIAN_POINT ( 'NONE',  ( -0.05187277790672228939, 0.4419080096627327481, -0.1624279055868658173 ) ) ;
#39362 = ORIENTED_EDGE ( 'NONE', *, *, #13917, .T. ) ;
#39363 = CARTESIAN_POINT ( 'NONE',  ( 0.1396326186464584285, -1.245954038625972871, 0.6057265985168657219 ) ) ;
#39364 = CARTESIAN_POINT ( 'NONE',  ( 0.2446503497336322552, -0.9283727152547225359, 0.6908355059567328205 ) ) ;
#39365 = CARTESIAN_POINT ( 'NONE',  ( 0.1472436744124528685, -1.061356063222618218, 0.9705180032994723538 ) ) ;
#39366 = CARTESIAN_POINT ( 'NONE',  ( 0.4991955362234085647, -1.540752879515209450, 0.6255465156695737550 ) ) ;
#39368 = CARTESIAN_POINT ( 'NONE',  ( 0.3051615010899081382, -1.653119291639537636, 0.5908386205647984113 ) ) ;
#39367 = CARTESIAN_POINT ( 'NONE',  ( 0.1131241454731939100, -0.6872203660140440151, -0.09530310615070609892 ) ) ;
#39369 = CARTESIAN_POINT ( 'NONE',  ( 0.2487198563054835165, -1.164593893902498234, 0.6393759972551884552 ) ) ;
#39370 = ORIENTED_EDGE ( 'NONE', *, *, #6439, .T. ) ;
#39371 = ORIENTED_EDGE ( 'NONE', *, *, #15487, .F. ) ;
#39372 = CARTESIAN_POINT ( 'NONE',  ( -0.02000000000000000042, -1.459219328725982034, -0.1828911325362468643 ) ) ;
#39373 = CARTESIAN_POINT ( 'NONE',  ( 0.1402999466524724737, -0.5606445496649763438, 0.4675943975877205894 ) ) ;
#39374 = LINE ( 'NONE', #4589, #30503 ) ;
#39375 = CARTESIAN_POINT ( 'NONE',  ( -0.2399999999999999079, -2.183180860297908144, -0.3591170932241134484 ) ) ;
#39376 = CARTESIAN_POINT ( 'NONE',  ( 0.07620027864266576412, -1.321376928151553498, 0.4820378534147667371 ) ) ;
#39377 = CARTESIAN_POINT ( 'NONE',  ( 0.3870588290862405079, -1.884497726405092832, -0.6962470674797399672 ) ) ;
#39378 = DIRECTION ( 'NONE',  ( 0.000000000000000000, 0.000000000000000000, 1.000000000000000000 ) ) ;
#39379 = CARTESIAN_POINT ( 'NONE',  ( 0.3677026761718887315, -0.9383931188863808837, 0.6934371584156296953 ) ) ;
#39380 = EDGE_CURVE ( 'NONE', #26668, #1874, #9602, .T. ) ;
#39381 = FACE_OUTER_BOUND ( 'NONE', #21088, .T. ) ;
#39382 = EDGE_CURVE ( 'NONE', #36294, #12543, #37040, .T. ) ;
#39383 = DIRECTION ( 'NONE',  ( 0.4999999999999962252, -0.6509737717187612516, 0.5711682313769330666 ) ) ;
#39384 = CYLINDRICAL_SURFACE ( 'NONE', #2219, 0.1000000000000000194 ) ;
#39385 = ORIENTED_EDGE ( 'NONE', *, *, #13691, .T. ) ;
#39386 = LINE ( 'NONE', #34429, #24129 ) ;
#39387 = FACE_OUTER_BOUND ( 'NONE', #6006, .T. ) ;
#39388 = EDGE_CURVE ( 'NONE', #3365, #35412, #7013, .T. ) ;
#39389 = CARTESIAN_POINT ( 'NONE',  ( -0.03672309138969661463, -0.2485858928251903077, -0.4115746274616722267 ) ) ;
#39390 = ORIENTED_EDGE ( 'NONE', *, *, #31822, .T. ) ;
#39391 = CARTESIAN_POINT ( 'NONE',  ( 0.5136072266423519217, -1.127739116876707470, 0.6738619914697276947 ) ) ;
#39392 = CARTESIAN_POINT ( 'NONE',  ( -0.1157923916715206808, -0.5295015842444287246, 0.3749999999999999445 ) ) ;
#39393 = B_SPLINE_CURVE_WITH_KNOTS ( 'NONE', 3,
 ( #30035, #30436, #2263, #36607 ),
 .UNSPECIFIED., .F., .F.,
 ( 4, 4 ),
 ( 0.000000000000000000, 1.000000000000000000 ),
 .UNSPECIFIED. ) ;
#39394 = CARTESIAN_POINT ( 'NONE',  ( 0.1803246710466453739, -1.251562748998523489, 0.7307791269380327082 ) ) ;
#39395 = ORIENTED_EDGE ( 'NONE', *, *, #36047, .T. ) ;
#39396 = LINE ( 'NONE', #8336, #8674 ) ;
#39397 = ADVANCED_FACE ( 'NONE', ( #21441 ), #35915, .T. ) ;
#39398 = CARTESIAN_POINT ( 'NONE',  ( 0.02953079040095491978, 0.09152108205202105773, 0.5223162075576462948 ) ) ;
#39399 = LINE ( 'NONE', #23591, #32937 ) ;
#39400 = EDGE_CURVE ( 'NONE', #38684, #13521, #9637, .T. ) ;
#39401 = CARTESIAN_POINT ( 'NONE',  ( 0.02953079040095717839, 0.4684706630666118365, 0.2484463060367366194 ) ) ;
#39402 = CARTESIAN_POINT ( 'NONE',  ( 0.4358268961743849146, -1.190236072996399441, 0.6640218714533226985 ) ) ;
#39404 = DIRECTION ( 'NONE',  ( -1.000000000000000000, 0.000000000000000000, 0.000000000000000000 ) ) ;
#39403 = CARTESIAN_POINT ( 'NONE',  ( -0.2399999999999999079, -3.681106669851795132, -0.07175300799092947102 ) ) ;
#39405 = CARTESIAN_POINT ( 'NONE',  ( -0.05283102792148800658, -0.2421768296208681170, -0.4008516595826048245 ) ) ;
#39406 = ORIENTED_EDGE ( 'NONE', *, *, #36575, .T. ) ;
#39407 = ADVANCED_FACE ( 'NONE', ( #25110 ), #18742, .T. ) ;
#39408 = CARTESIAN_POINT ( 'NONE',  ( 0.2059273467974225835, -1.283046334493782359, -0.4125659523519145111 ) ) ;
#39409 = VERTEX_POINT ( 'NONE', #15234 ) ;
#39410 = FACE_OUTER_BOUND ( 'NONE', #21298, .T. ) ;
#39411 = CARTESIAN_POINT ( 'NONE',  ( 0.08491816545164443397, -0.6773013968507372029, 0.4888687927153864132 ) ) ;
#39413 = CARTESIAN_POINT ( 'NONE',  ( 0.4793242053826342608, -1.117309586606285210, -0.6340321207832128048 ) ) ;
#39412 = CARTESIAN_POINT ( 'NONE',  ( 0.08805611400531067334, -0.6473513853021811704, 0.02913009454904720227 ) ) ;
#39414 = CARTESIAN_POINT ( 'NONE',  ( 0.1761392914182259850, -1.265181628236080824, 0.4952186049836316828 ) ) ;
#39415 = ORIENTED_EDGE ( 'NONE', *, *, #22567, .F. ) ;
#39416 = ORIENTED_EDGE ( 'NONE', *, *, #22110, .F. ) ;
#39417 = DIRECTION ( 'NONE',  ( 0.8660512985181135770, 0.4999551463232370652, -1.983296656985675225E-15 ) ) ;
#39418 = CARTESIAN_POINT ( 'NONE',  ( 0.2649443680508836718, -0.9506954219886920576, 0.7345657905482877448 ) ) ;
#39419 = EDGE_LOOP ( 'NONE', ( #24004, #38882, #1428, #1238 ) ) ;
#39420 = CARTESIAN_POINT ( 'NONE',  ( 0.05999999999999990757, 0.09520121321898405986, -0.1758883992810029440 ) ) ;
#39421 = CARTESIAN_POINT ( 'NONE',  ( 0.05634402396114423367, -0.4396062797411974254, 0.1319984305213770803 ) ) ;
#39422 = CARTESIAN_POINT ( 'NONE',  ( 0.3673299760992552176, -1.767204635010063196, -0.4401329826727911620 ) ) ;
#39423 = CARTESIAN_POINT ( 'NONE',  ( 0.2257601701386385828, -1.236660534205411333, 0.5094317095389198080 ) ) ;
#39424 = CIRCLE ( 'NONE', #12498, 0.2000000000000000111 ) ;
#39425 = FACE_OUTER_BOUND ( 'NONE', #11540, .T. ) ;
#39426 = DIRECTION ( 'NONE',  ( -1.000000000000000000, -2.280301054154495132E-31, 1.664003471950577689E-31 ) ) ;
#39427 = CARTESIAN_POINT ( 'NONE',  ( 0.7110913793137424443, -1.453804679565707803, 0.7028629728786995878 ) ) ;
#39428 = AXIS2_PLACEMENT_3D ( 'NONE', #36804, #8616, #33724 ) ;
#39429 = CARTESIAN_POINT ( 'NONE',  ( -0.02000000000000000042, -1.598492537578166672, -0.1971380022280825872 ) ) ;
#39430 = FACE_OUTER_BOUND ( 'NONE', #30025, .T. ) ;
#39431 = EDGE_CURVE ( 'NONE', #37277, #8591, #504, .T. ) ;
#39432 = CARTESIAN_POINT ( 'NONE',  ( 0.6156641970611075321, -1.571178582061410145, -0.5844328501603425208 ) ) ;
#39433 = DIRECTION ( 'NONE',  ( 1.000000000000000000, 0.000000000000000000, 7.734859593387037307E-16 ) ) ;
#39434 = DIRECTION ( 'NONE',  ( 1.000000000000000000, 0.000000000000000000, 0.000000000000000000 ) ) ;
#39435 = ADVANCED_FACE ( 'NONE', ( #22048 ), #19591, .T. ) ;
#39436 = FACE_OUTER_BOUND ( 'NONE', #23774, .T. ) ;
#39437 = CARTESIAN_POINT ( 'NONE',  ( -0.1061036098701634706, -0.4827967145417200179, 0.3599999999999998757 ) ) ;
#39438 = CARTESIAN_POINT ( 'NONE',  ( -3.276078897458520021E-17, -0.4262518876079541830, 0.1281883534109924672 ) ) ;
#39439 = CARTESIAN_POINT ( 'NONE',  ( 0.5752554920797638971, -1.540183446532599643, -0.5501855072907599897 ) ) ;
#39440 = CARTESIAN_POINT ( 'NONE',  ( -0.02000000000000000042, -2.551729310907437043, -0.4286726180052709001 ) ) ;
#39441 = FACE_OUTER_BOUND ( 'NONE', #30206, .T. ) ;
#39442 = CARTESIAN_POINT ( 'NONE',  ( -0.04211812644076929485, -0.2687274166943736664, 0.3844079338164319570 ) ) ;
#39443 = ORIENTED_EDGE ( 'NONE', *, *, #33563, .F. ) ;
#39444 = CARTESIAN_POINT ( 'NONE',  ( 0.4612498305140941834, -1.075380691928112586, -0.6133311933496794488 ) ) ;
#39445 = CARTESIAN_POINT ( 'NONE',  ( 0.2322138788700108258, -1.233113307957229177, 0.3157417262808777658 ) ) ;
#39446 = CARTESIAN_POINT ( 'NONE',  ( 0.08030483728411769162, -0.5440987430357651089, 0.1459341340629038419 ) ) ;
#39447 = DIRECTION ( 'NONE',  ( -0.9378410757839555911, 0.2807814858886595322, -0.2039996905746409572 ) ) ;
#39448 = CARTESIAN_POINT ( 'NONE',  ( 0.3633940536647746189, -1.097306544473756640, 0.7529995174779674505 ) ) ;
#39450 = EDGE_LOOP ( 'NONE', ( #23654, #35220, #19592 ) ) ;
#39449 = CARTESIAN_POINT ( 'NONE',  ( -0.04293701532779589658, 0.4432143466407589272, 0.2195216604697213802 ) ) ;
#39451 = CARTESIAN_POINT ( 'NONE',  ( 0.4504611332311936889, -1.053473412190887304, 0.6915920958210214353 ) ) ;
#39452 = EDGE_CURVE ( 'NONE', #38533, #17741, #37889, .T. ) ;
#39453 = DIRECTION ( 'NONE',  ( -0.4999551463232372317, 0.8660512985181135770, -0.000000000000000000 ) ) ;
#39454 = EDGE_LOOP ( 'NONE', ( #5051, #19392, #35451, #12861, #10631, #22271 ) ) ;
#39455 = DIRECTION ( 'NONE',  ( 1.000000000000000000, 0.000000000000000000, 0.000000000000000000 ) ) ;
#39456 = ORIENTED_EDGE ( 'NONE', *, *, #12267, .F. ) ;
#39457 = AXIS2_PLACEMENT_3D ( 'NONE', #34550, #15021, #40095 ) ;
#39458 = CARTESIAN_POINT ( 'NONE',  ( 0.3583310641576757938, -1.622257436576277190, 0.6094965212440786040 ) ) ;
#39460 = CARTESIAN_POINT ( 'NONE',  ( -0.2399999999999999079, -3.849534981189179028, -0.1910928155360645808 ) ) ;
#39459 = CARTESIAN_POINT ( 'NONE',  ( 0.6778803828687806066, -1.516512415086665344, 0.4467122667541399972 ) ) ;
#39461 = CARTESIAN_POINT ( 'NONE',  ( -0.1499999999999996336, 0.000000000000000000, 0.000000000000000000 ) ) ;
#39462 = CARTESIAN_POINT ( 'NONE',  ( 0.1820341357843785479, -1.296823278962681902, -0.2983537100936060060 ) ) ;
#39463 = ORIENTED_EDGE ( 'NONE', *, *, #7001, .T. ) ;
#39464 = ORIENTED_EDGE ( 'NONE', *, *, #4503, .F. ) ;
#39465 = CARTESIAN_POINT ( 'NONE',  ( 0.0005169533006796693227, -1.951327190372867504, -0.6596122894433742445 ) ) ;
#39466 = CARTESIAN_POINT ( 'NONE',  ( -0.02000000000000000042, -2.626773565144302935, -0.2726934094652516127 ) ) ;
#39467 = CARTESIAN_POINT ( 'NONE',  ( 0.09580522634512994573, -0.8544855528359687202, 0.4211259006973531172 ) ) ;
#39468 = CARTESIAN_POINT ( 'NONE',  ( 0.3405242896115074913, -1.744906522954273731, 0.4484829386636806081 ) ) ;
#39469 = DIRECTION ( 'NONE',  ( 0.8660512985181134660, 0.4999551463232372872, 0.000000000000000000 ) ) ;
#39470 = CARTESIAN_POINT ( 'NONE',  ( -0.2399999999999999079, -2.183180860297908144, -0.4937760292030871079 ) ) ;
#39471 = DIRECTION ( 'NONE',  ( 0.3468893892380805477, -0.2594111197900994537, -0.9013177145509114752 ) ) ;
#39472 = CARTESIAN_POINT ( 'NONE',  ( 0.04582889109739231304, 0.4389390569944019438, 0.2108010426992244501 ) ) ;
#39473 = CARTESIAN_POINT ( 'NONE',  ( -0.06908312040360713169, -0.09959325338431362917, 0.3602693341844379060 ) ) ;
#39474 = DIRECTION ( 'NONE',  ( 0.8660512985181134660, 0.4999551463232371762, 0.000000000000000000 ) ) ;
#39475 = APPROVAL_ROLE ( '' ) ;
#39476 = VECTOR ( 'NONE', #3051, 39.37007874015748143 ) ;
#39477 = CARTESIAN_POINT ( 'NONE',  ( 0.06056337598226081698, -1.309773928473624505, 0.6311107274231992914 ) ) ;
#39478 = CARTESIAN_POINT ( 'NONE',  ( 0.4510273968575216341, -1.245587961952838718, 0.6057417262809815517 ) ) ;
#39479 = CARTESIAN_POINT ( 'NONE',  ( 0.3249483201304784741, -1.768002432019315728, 0.5182417262812728520 ) ) ;
#39480 = AXIS2_PLACEMENT_3D ( 'NONE', #24238, #12479, #27720 ) ;
#39481 = CIRCLE ( 'NONE', #36844, 0.04999999999999998890 ) ;
#39482 = CARTESIAN_POINT ( 'NONE',  ( 2.290505790419000988E-05, -0.4780051411654945848, -0.01121176583438007919 ) ) ;
#39483 = CARTESIAN_POINT ( 'NONE',  ( 0.3971095453229756544, -1.735560539021580695, -0.5931764296607824338 ) ) ;
#39484 = CIRCLE ( 'NONE', #21775, 0.1400000000000007350 ) ;
#39485 = DIRECTION ( 'NONE',  ( -0.4887635750372988364, -0.8724162812079787610, 3.838072908882819854E-15 ) ) ;
#39486 = CARTESIAN_POINT ( 'NONE',  ( 0.02869942827333498564, -0.06034320897027730529, -0.4947801815387851132 ) ) ;
#39487 = ORIENTED_EDGE ( 'NONE', *, *, #5444, .T. ) ;
#39488 = EDGE_LOOP ( 'NONE', ( #17131, #4953, #30355, #12849 ) ) ;
#39489 = DIRECTION ( 'NONE',  ( 2.532366176626896502E-12, 1.000000000000000000, 5.691349986800531115E-16 ) ) ;
#39490 = ORIENTED_EDGE ( 'NONE', *, *, #14535, .T. ) ;
#39491 = CARTESIAN_POINT ( 'NONE',  ( 0.000000000000000000, 0.08637707520836798714, -0.07506498716826678907 ) ) ;
#39492 = CARTESIAN_POINT ( 'NONE',  ( -0.1081053389376798041, -0.4929871184167937126, 0.1128267017629384777 ) ) ;
#39494 = ORIENTED_EDGE ( 'NONE', *, *, #21320, .T. ) ;
#39493 = CARTESIAN_POINT ( 'NONE',  ( 0.008656601633535388959, -0.6460992163107364128, -0.007090344436191942101 ) ) ;
#39495 = VERTEX_POINT ( 'NONE', #805 ) ;
#39496 = CARTESIAN_POINT ( 'NONE',  ( 0.1519284701276231164, -0.5919472871766352506, 0.5183721702484739291 ) ) ;
#39497 = VERTEX_POINT ( 'NONE', #29152 ) ;
#39498 = DIRECTION ( 'NONE',  ( 0.000000000000000000, -0.7071067811865474617, -0.7071067811865475727 ) ) ;
#39500 = CARTESIAN_POINT ( 'NONE',  ( 0.5444814301263717349, -1.595658467509692313, -0.4724618950513508331 ) ) ;
#39499 = CARTESIAN_POINT ( 'NONE',  ( -0.04230188431063475890, -0.4429734639576313193, -0.1531098457317282835 ) ) ;
#39501 = DIRECTION ( 'NONE',  ( 1.000000000000000000, 6.779273404243070203E-32, 4.314083075427408311E-32 ) ) ;
#39502 = COORDINATED_UNIVERSAL_TIME_OFFSET ( 0, 0, .AHEAD. ) ;
#39503 = AXIS2_PLACEMENT_3D ( 'NONE', #14930, #40211, #5661 ) ;
#39504 = CARTESIAN_POINT ( 'NONE',  ( 0.1909293087668044175, -1.257065863231180858, -0.7137147910705018417 ) ) ;
#39506 = ORIENTED_EDGE ( 'NONE', *, *, #24256, .F. ) ;
#39505 = EDGE_LOOP ( 'NONE', ( #26448, #20878, #3482, #24975, #6163 ) ) ;
#39507 = CARTESIAN_POINT ( 'NONE',  ( -0.02000000000000000042, -2.183180860297908144, -0.4937760292030871079 ) ) ;
#39508 = CARTESIAN_POINT ( 'NONE',  ( 0.1059350862884271965, -1.337751531233084545, 0.7070564584916527728 ) ) ;
#39509 = CARTESIAN_POINT ( 'NONE',  ( 0.09365314453647033410, -0.5743219976380223857, 0.2688796733879867951 ) ) ;
#39510 = CIRCLE ( 'NONE', #21798, 0.1249999999999999584 ) ;
#39511 =( BOUNDED_SURFACE ( )  B_SPLINE_SURFACE ( 3, 2, ( 
 ( #29533, #19485, #10219 ),
 ( #16799, #29347, #16584 ),
 ( #13882, #7100, #991 ),
 ( #4433, #31818, #35104 ),
 ( #6909, #4020, #32014 ),
 ( #7297, #16992, #1375 ),
 ( #23401, #3823, #19669 ),
 ( #16198, #25649, #32410 ),
 ( #10003, #16380, #26071 ),
 ( #22577, #28920, #22788 ),
 ( #26456, #13692, #26259 ),
 ( #4233, #32623, #25864 ) ),
 .UNSPECIFIED., .F., .F., .T. ) 
 B_SPLINE_SURFACE_WITH_KNOTS ( ( 4, 2, 2, 2, 2, 4 ),
 ( 3, 3 ),
 ( 0.001713391272003884783, 0.002288612648294801721, 0.002863834024585718441, 0.003151444712731176802, 0.003439055400876635596, 0.004014276777167552317 ),
 ( 0.000000000000000000, 1.000000000000000000 ),
 .UNSPECIFIED. ) 
 GEOMETRIC_REPRESENTATION_ITEM ( )  RATIONAL_B_SPLINE_SURFACE ( (
 ( 1.000000000000000000, 0.9128709291753012156, 1.000000000000000000),
 ( 1.000000000000000000, 0.9128719127418516432, 1.000000000000000000),
 ( 1.000000000000000000, 0.9128123349203235426, 1.000000000000000000),
 ( 1.000000000000000000, 0.9126095266096564407, 1.000000000000000000),
 ( 1.000000000000000000, 0.9124632789547948430, 1.000000000000000000),
 ( 1.000000000000000000, 0.9122369551430161705, 1.000000000000000000),
 ( 1.000000000000000000, 0.9121592698944235300, 1.000000000000000000),
 ( 1.000000000000000000, 0.9120159902105161587, 1.000000000000000000),
 ( 1.000000000000000000, 0.9119497308970357929, 1.000000000000000000),
 ( 1.000000000000000000, 0.9117802546605157099, 1.000000000000000000),
 ( 1.000000000000000000, 0.9117114107497396036, 1.000000000000000000),
 ( 1.000000000000000000, 0.9117127123830639501, 1.000000000000000000) ) ) 
 REPRESENTATION_ITEM ( '' )  SURFACE ( )  );
#39512 = CARTESIAN_POINT ( 'NONE',  ( 0.1870925830679437130, -0.7146760840282513350, 0.03103855360005942920 ) ) ;
#39513 = CARTESIAN_POINT ( 'NONE',  ( 0.4757310988838256427, -1.669109449190596228, 0.5669542959959941175 ) ) ;
#39514 = CARTESIAN_POINT ( 'NONE',  ( -0.2746410161513782033, -2.253314830856113726, -0.6753616220517687507 ) ) ;
#39515 = CIRCLE ( 'NONE', #36905, 0.03000000000000008910 ) ;
#39516 = CARTESIAN_POINT ( 'NONE',  ( 0.3461189067787796558, -1.156139424848509956, 0.4335238789691411299 ) ) ;
#39517 = FACE_OUTER_BOUND ( 'NONE', #11921, .T. ) ;
#39518 = CARTESIAN_POINT ( 'NONE',  ( 0.1876053338355621880, -0.6785855078148245179, 0.1477569985384105666 ) ) ;
#39519 = CARTESIAN_POINT ( 'NONE',  ( 0.1999999999696201736, -2.080276846833732929, -0.2651855839716015795 ) ) ;
#39520 = CARTESIAN_POINT ( 'NONE',  ( 0.01135805250241819081, -0.9385525037653906777, 0.08271764842014434072 ) ) ;
#39521 = CARTESIAN_POINT ( 'NONE',  ( 0.4115766028365042128, -1.733048369835246794, 0.5182417262812423209 ) ) ;
#39522 =( CONVERSION_BASED_UNIT ( 'INCH', #26991 ) LENGTH_UNIT ( ) NAMED_UNIT ( #4161 ) );
#39523 = CARTESIAN_POINT ( 'NONE',  ( 0.6121698487542911460, -1.614213617923458521, -0.4893840166461958519 ) ) ;
#39524 = CARTESIAN_POINT ( 'NONE',  ( 0.0003293075040918708759, -0.6974492147978401668, 0.2474296275395909961 ) ) ;
#39525 = CARTESIAN_POINT ( 'NONE',  ( 0.4718294406633598559, -1.074170765704426822, 0.6461978756939577018 ) ) ;
#39526 = DATE_AND_TIME ( #17541, #31900 ) ;
#39527 = CARTESIAN_POINT ( 'NONE',  ( 0.5225354986670117663, -1.146792065252953297, 0.8742509268737332917 ) ) ;
#39528 = AXIS2_PLACEMENT_3D ( 'NONE', #22446, #16271, #38473 ) ;
#39529 = LINE ( 'NONE', #32959, #8976 ) ;
#39530 = CARTESIAN_POINT ( 'NONE',  ( 0.03174060074381680058, -0.07585527192505218952, -0.5190439939302199379 ) ) ;
#39531 = CIRCLE ( 'NONE', #9980, 0.02499999999999993894 ) ;
#39532 = AXIS2_PLACEMENT_3D ( 'NONE', #31255, #18693, #15615 ) ;
#39533 = ORIENTED_EDGE ( 'NONE', *, *, #26487, .T. ) ;
#39534 = CARTESIAN_POINT ( 'NONE',  ( 0.1406468284892466447, -1.193466478313442991, 0.9284149979398328423 ) ) ;
#39535 = CIRCLE ( 'NONE', #33643, 0.01499999999999995087 ) ;
#39536 = CARTESIAN_POINT ( 'NONE',  ( 0.3538719729184752749, -1.624715450675502160, 0.4182417262808775238 ) ) ;
#39538 = ORIENTED_EDGE ( 'NONE', *, *, #12510, .T. ) ;
#39537 = CARTESIAN_POINT ( 'NONE',  ( 0.3891966927463759718, -1.924247350197065609, -0.4910180813531025978 ) ) ;
#39539 = CARTESIAN_POINT ( 'NONE',  ( -0.08000000000000000167, -2.585754275622221154, -0.2040099479399058724 ) ) ;
#39540 = CARTESIAN_POINT ( 'NONE',  ( 0.5387674647098039671, -1.171534441891039169, 0.7413454372389880476 ) ) ;
#39542 = ORIENTED_EDGE ( 'NONE', *, *, #25336, .T. ) ;
#39541 = EDGE_LOOP ( 'NONE', ( #30524, #24546, #121, #21912 ) ) ;
#39543 = CARTESIAN_POINT ( 'NONE',  ( 0.02999607453758948092, -2.087869005097287900, -0.7252195465745520098 ) ) ;
#39544 = ORIENTED_EDGE ( 'NONE', *, *, #5982, .F. ) ;
#39545 = CYLINDRICAL_SURFACE ( 'NONE', #29621, 0.01500000000000004628 ) ;
#39546 = DIRECTION ( 'NONE',  ( 0.000000000000000000, 0.000000000000000000, -1.000000000000000000 ) ) ;
#39547 = CALENDAR_DATE ( 2026, 13, 10 ) ;
#39548 = CARTESIAN_POINT ( 'NONE',  ( -0.04308745346420850275, 0.4494111352305566465, -0.2058334250444009417 ) ) ;
#39549 = ORIENTED_EDGE ( 'NONE', *, *, #875, .T. ) ;
#39550 = CARTESIAN_POINT ( 'NONE',  ( 0.1897001248997009504, -1.237817139529930222, 0.5863507469836753971 ) ) ;
#39551 = EDGE_CURVE ( 'NONE', #35716, #4635, #30666, .T. ) ;
#39552 = CARTESIAN_POINT ( 'NONE',  ( 0.2609408554674475522, -0.9584677431853507734, 0.7004531198503530787 ) ) ;
#39553 = EDGE_CURVE ( 'NONE', #9411, #25380, #28754, .T. ) ;
#39554 = CARTESIAN_POINT ( 'NONE',  ( 0.2692473483777980126, -1.497112465990877439, 1.008263284785997804 ) ) ;
#39555 = CARTESIAN_POINT ( 'NONE',  ( 0.4975907999090993794, -1.542531306350466869, 0.5755255995287604787 ) ) ;
#39557 = CARTESIAN_POINT ( 'NONE',  ( -2.070754768975509919, -0.09959325338431655739, 0.1178658435937004478 ) ) ;
#39556 = CARTESIAN_POINT ( 'NONE',  ( 0.1149968254612746543, -0.4588679775494129975, 0.06802948968277178210 ) ) ;
#39558 = CARTESIAN_POINT ( 'NONE',  ( 0.02367353041037730671, -0.9777710647417211520, 0.4475088345234511933 ) ) ;
#39559 = ORIENTED_EDGE ( 'NONE', *, *, #22365, .F. ) ;
#39560 = EDGE_LOOP ( 'NONE', ( #26583, #12270, #11745, #24096 ) ) ;
#39561 = EDGE_CURVE ( 'NONE', #36434, #27541, #17704, .T. ) ;
#39562 = VECTOR ( 'NONE', #24218, 39.37007874015748143 ) ;
#39563 = CARTESIAN_POINT ( 'NONE',  ( -0.05464101615137766793, -2.548345659627495596, -0.2263512047145338768 ) ) ;
#39564 = CARTESIAN_POINT ( 'NONE',  ( 0.4977951372335264746, -1.107966894584811790, 0.8692732641236018409 ) ) ;
#39565 = ADVANCED_FACE ( 'NONE', ( #13109 ), #25670, .T. ) ;
#39566 = DIRECTION ( 'NONE',  ( 0.9823333030490233320, -0.1871397384865000069, 0.000000000000000000 ) ) ;
#39567 = AXIS2_PLACEMENT_3D ( 'NONE', #9833, #6740, #19520 ) ;
#39568 = AXIS2_PLACEMENT_3D ( 'NONE', #29938, #11201, #20681 ) ;
#39569 = CARTESIAN_POINT ( 'NONE',  ( 0.3675325340839428190, -2.037914281822962081, -0.5035866893277683998 ) ) ;
#39570 = CARTESIAN_POINT ( 'NONE',  ( -0.05186792262757027039, -0.4419037732007360386, -0.1624768558011068786 ) ) ;
#39571 = CARTESIAN_POINT ( 'NONE',  ( -0.2746410161513776482, -3.941790907013290823, -0.4709369376873030477 ) ) ;
#39572 = CARTESIAN_POINT ( 'NONE',  ( 0.3866324372511995011, -1.865059148935370503, -0.6965146800415932260 ) ) ;
#39573 = CARTESIAN_POINT ( 'NONE',  ( 0.3540817610093318635, -1.633452470505663667, 0.5182417262812423209 ) ) ;
#39574 = CARTESIAN_POINT ( 'NONE',  ( 0.1906247196645202702, -0.5843772811062371009, 0.1457185332388696020 ) ) ;
#39575 = B_SPLINE_SURFACE_WITH_KNOTS ( 'NONE', 1, 3, ( 
 ( #8906, #40381, #15686, #6418 ),
 ( #21483, #28053, #22096, #15283 ),
 ( #34004, #27444, #28237, #6009 ),
 ( #5808, #2345, #24765, #21669 ) ),
 .UNSPECIFIED., .F., .F., .F.,
 ( 2, 1, 1, 2 ),
 ( 4, 4 ),
 ( -1.012000000000000233, 0.000000000000000000, 1.000000000000000000, 2.018000000000001126 ),
 ( -0.005833846140041338939, 0.005833846140041338071 ),
 .UNSPECIFIED. ) ;
#39576 = LINE ( 'NONE', #23979, #28030 ) ;
#39577 = CIRCLE ( 'NONE', #33677, 0.01500000000000002894 ) ;
#39578 = EDGE_CURVE ( 'NONE', #8227, #8719, #10323, .T. ) ;
#39579 = APPLIED_PERSON_AND_ORGANIZATION_ASSIGNMENT ( #18382, #21502, ( #1014 ) ) ;
#39580 = CARTESIAN_POINT ( 'NONE',  ( 0.1098394514474842348, -1.393562438875942444, -0.3305732284332606463 ) ) ;
#39581 = CARTESIAN_POINT ( 'NONE',  ( 0.4491687606894799178, -1.659573487732471264, -0.3947185122250792544 ) ) ;
#39582 = CARTESIAN_POINT ( 'NONE',  ( 0.4692656535582095945, -1.239599139632956426, 0.6019514904091477492 ) ) ;
#39583 = CARTESIAN_POINT ( 'NONE',  ( -0.04293324258486902467, -0.07181764475132905445, -0.4893676133895085156 ) ) ;
#39584 = CARTESIAN_POINT ( 'NONE',  ( 0.6068869525525029118, -1.480059939399680280, 0.5671080680285526254 ) ) ;
#39585 = EDGE_LOOP ( 'NONE', ( #17848, #14256, #9747, #18062 ) ) ;
#39586 = CARTESIAN_POINT ( 'NONE',  ( -1.502516396515344672E-15, -0.3899999999999999578, 5.463695987328526437E-16 ) ) ;
#39587 = CONICAL_SURFACE ( 'NONE', #17259, 0.1400000000000009570, 1.047197551196600518 ) ;
#39588 = CARTESIAN_POINT ( 'NONE',  ( 0.1876053338355621880, -0.6785855078148245179, 0.1477569985384105666 ) ) ;
#39589 = EDGE_CURVE ( 'NONE', #4481, #16266, #35129, .T. ) ;
#39590 = CARTESIAN_POINT ( 'NONE',  ( 0.1204589479551298192, -1.085572435350046216, 0.7460617499609929482 ) ) ;
#39591 = ORIENTED_EDGE ( 'NONE', *, *, #18209, .F. ) ;
#39592 = CARTESIAN_POINT ( 'NONE',  ( -0.2399999999999999079, -3.739689364820627748, -0.3461216533844236887 ) ) ;
#39593 = AXIS2_PLACEMENT_3D ( 'NONE', #11764, #13490, #29330 ) ;
#39594 = AXIS2_PLACEMENT_3D ( 'NONE', #776, #26060, #20081 ) ;
#39595 = LINE ( 'NONE', #36718, #40122 ) ;
#39596 = CARTESIAN_POINT ( 'NONE',  ( 0.1574750639814709308, -1.391761509719479761, 0.4336789700803105330 ) ) ;
#39597 = CARTESIAN_POINT ( 'NONE',  ( 9.192809626365503817E-18, 0.08637707520836798714, 0.07506498716826678907 ) ) ;
#39598 = VECTOR ( 'NONE', #22675, 39.37007874015748143 ) ;
#39599 = CARTESIAN_POINT ( 'NONE',  ( 0.4787510807856267259, -1.256362448863320269, 0.6027525166291474168 ) ) ;
#39601 = CARTESIAN_POINT ( 'NONE',  ( -1.496393162519607993E-15, -0.3899999999999999578, -0.04999999999999947542 ) ) ;
#39600 = DIRECTION ( 'NONE',  ( -0.05576617209162609834, -0.2535907321156583571, 0.9657027879401052228 ) ) ;
#39602 = CARTESIAN_POINT ( 'NONE',  ( 0.02872242845530344549, -0.3729171224323687417, -0.3802687114177517036 ) ) ;
#39603 = EDGE_LOOP ( 'NONE', ( #11644, #5961 ) ) ;
#39604 = ORIENTED_EDGE ( 'NONE', *, *, #15191, .F. ) ;
#39605 = CARTESIAN_POINT ( 'NONE',  ( 0.07006815180908300411, -1.315301596572415299, 0.5080907171456733318 ) ) ;
#39606 = ORIENTED_EDGE ( 'NONE', *, *, #7735, .F. ) ;
#39607 = EDGE_CURVE ( 'NONE', #4682, #25917, #5692, .T. ) ;
#39608 = CARTESIAN_POINT ( 'NONE',  ( 0.1860373355776311632, -0.4547550531002670371, 0.008518417185872215538 ) ) ;
#39609 = CARTESIAN_POINT ( 'NONE',  ( 0.06201235461866828891, -0.5659405159657984186, 0.2619933746457878687 ) ) ;
#39610 = AXIS2_PLACEMENT_3D ( 'NONE', #22818, #811, #37817 ) ;
#39612 = DIRECTION ( 'NONE',  ( 0.000000000000000000, 0.000000000000000000, 1.000000000000000000 ) ) ;
#39611 = CARTESIAN_POINT ( 'NONE',  ( 0.6889402512469305906, -1.555172295161277196, 0.5968700266842814628 ) ) ;
#39613 = CARTESIAN_POINT ( 'NONE',  ( -0.1172150163383985644, -0.4875187859579053207, 0.1204312767266922934 ) ) ;
#39614 = ORIENTED_EDGE ( 'NONE', *, *, #6855, .T. ) ;
#39615 = EDGE_CURVE ( 'NONE', #12702, #40154, #20209, .T. ) ;
#39616 = ORIENTED_EDGE ( 'NONE', *, *, #19648, .T. ) ;
#39617 = CARTESIAN_POINT ( 'NONE',  ( 0.5640895105453352931, -1.503407492374277510, 0.5358556994421860287 ) ) ;
#39618 = ADVANCED_FACE ( 'NONE', ( #3245 ), #31438, .T. ) ;
#39619 = CARTESIAN_POINT ( 'NONE',  ( 0.5121199761860573130, -1.393593559852499109, 0.7948695422178503334 ) ) ;
#39620 = ORIENTED_EDGE ( 'NONE', *, *, #27361, .T. ) ;
#39621 = CARTESIAN_POINT ( 'NONE',  ( 0.3252720331744159421, -1.756211604028340423, 0.5534074152425280113 ) ) ;
#39622 = CARTESIAN_POINT ( 'NONE',  ( -0.2746410161513776482, -4.218511633990150500, -0.6415916474861803609 ) ) ;
#39623 = CARTESIAN_POINT ( 'NONE',  ( -0.05464101615137787610, -2.504411011601259673, -0.4441669705721119632 ) ) ;
#39624 = CARTESIAN_POINT ( 'NONE',  ( 0.1981403273678030152, -1.252645933650147425, 0.4502181074018651308 ) ) ;
#39625 = CIRCLE ( 'NONE', #917, 0.1033070866141734129 ) ;
#39626 = CARTESIAN_POINT ( 'NONE',  ( -0.2399999999999999079, -1.804235510932644004, -0.1501860188971498311 ) ) ;
#39627 = CARTESIAN_POINT ( 'NONE',  ( 0.3862498284634955925, -1.756282559639558372, -0.4621846277522613233 ) ) ;
#39628 = CARTESIAN_POINT ( 'NONE',  ( 0.7145247768745858208, -1.460049439684881323, 0.6872404240164239342 ) ) ;
#39629 = AXIS2_PLACEMENT_3D ( 'NONE', #5693, #39852, #2422 ) ;
#39630 = TOROIDAL_SURFACE ( 'NONE', #17289, 0.1700000000000000400, 0.02999999999999999889 ) ;
#39631 = DIRECTION ( 'NONE',  ( -7.000205099780314469E-17, -1.000000000000000000, 6.590151126658399604E-16 ) ) ;
#39632 = ADVANCED_FACE ( 'NONE', ( #14517 ), #19516, .F. ) ;
#39633 = CARTESIAN_POINT ( 'NONE',  ( 0.0001243953464272101240, -0.9491217415751835862, 0.2153467644550133564 ) ) ;
#39634 = CARTESIAN_POINT ( 'NONE',  ( 0.6013563731205958662, -1.595925901742404562, -0.5276017758477205000 ) ) ;
#39635 = CARTESIAN_POINT ( 'NONE',  ( 0.4570244656720055532, -1.686924280111764984, -0.6191500722721138272 ) ) ;
#39636 = CARTESIAN_POINT ( 'NONE',  ( 0.02999999999997910935, -2.094376243145855465, -0.2600538233928666454 ) ) ;
#39637 = CYLINDRICAL_SURFACE ( 'NONE', #22539, 0.6115209409081865388 ) ;
#39638 = VECTOR ( 'NONE', #9438, 39.37007874015748143 ) ;
#39639 = CARTESIAN_POINT ( 'NONE',  ( -0.05634307799789459864, 0.4395998308137155086, -0.1320249839695989136 ) ) ;
#39640 = AXIS2_PLACEMENT_3D ( 'NONE', #22159, #37763, #3201 ) ;
#39641 = CARTESIAN_POINT ( 'NONE',  ( 0.09580854502948936424, -0.9100554415251292939, 0.8942175666832257175 ) ) ;
#39642 = FACE_OUTER_BOUND ( 'NONE', #14367, .T. ) ;
#39643 = CARTESIAN_POINT ( 'NONE',  ( -2.070754768975505034, -0.09959325338431362917, 0.3749999999999976130 ) ) ;
#39644 = LINE ( 'NONE', #26910, #16012 ) ;
#39645 = ORIENTED_EDGE ( 'NONE', *, *, #18433, .T. ) ;
#39646 = CARTESIAN_POINT ( 'NONE',  ( 0.4806378395295555772, -1.105637800341301880, -0.6194292131661300882 ) ) ;
#39647 = ORIENTED_EDGE ( 'NONE', *, *, #38305, .T. ) ;
#39648 = CARTESIAN_POINT ( 'NONE',  ( 0.3414116791095713754, -1.169548512706389154, 0.5830580198056709573 ) ) ;
#39649 = CARTESIAN_POINT ( 'NONE',  ( -0.2399999999999999079, -3.751862894713570817, -0.4282819086714443890 ) ) ;
#39650 = CARTESIAN_POINT ( 'NONE',  ( 0.6118928672170725891, -1.553152052717160281, -0.4073905701233934695 ) ) ;
#39651 = AXIS2_PLACEMENT_3D ( 'NONE', #28468, #16146, #3784 ) ;
#39652 = CARTESIAN_POINT ( 'NONE',  ( 0.4204492835407447893, -1.176608965458264322, 0.7497476517331604917 ) ) ;
#39654 = ORIENTED_EDGE ( 'NONE', *, *, #19758, .T. ) ;
#39653 = CARTESIAN_POINT ( 'NONE',  ( -0.03309060444528683087, 0.4608881774262392206, 0.2425132784556342513 ) ) ;
#39655 = CARTESIAN_POINT ( 'NONE',  ( 0.2247355409086003175, -0.8309010600190726015, 0.4364284219733364223 ) ) ;
#39656 = VERTEX_POINT ( 'NONE', #16821 ) ;
#39657 = CARTESIAN_POINT ( 'NONE',  ( 0.02880027917499857273, -1.580366911349619263, -0.3737892410411999822 ) ) ;
#39658 = VERTEX_POINT ( 'NONE', #26278 ) ;
#39659 = DIRECTION ( 'NONE',  ( 0.000000000000000000, 3.330669073875470114E-16, 1.000000000000000000 ) ) ;
#39660 = AXIS2_PLACEMENT_3D ( 'NONE', #30336, #2166, #39799 ) ;
#39661 = AXIS2_PLACEMENT_3D ( 'NONE', #38645, #28791, #650 ) ;
#39662 = CARTESIAN_POINT ( 'NONE',  ( 0.2981414330301035975, -1.451159418586606797, 0.8869886242261938447 ) ) ;
#39664 = CARTESIAN_POINT ( 'NONE',  ( 0.1869923964628150137, -0.6032852809087916324, 0.0007069082392771173411 ) ) ;
#39663 = CARTESIAN_POINT ( 'NONE',  ( 0.6752983665511703704, -1.520205868421071971, 0.4435471312318282622 ) ) ;
#39665 = CARTESIAN_POINT ( 'NONE',  ( -0.2399999999999999079, -3.253295730098268113, -0.6063490597057096254 ) ) ;
#39666 = EDGE_CURVE ( 'NONE', #23391, #8354, #24776, .T. ) ;
#39667 = ORIENTED_EDGE ( 'NONE', *, *, #13739, .F. ) ;
#39668 = VERTEX_POINT ( 'NONE', #29975 ) ;
#39669 = AXIS2_PLACEMENT_3D ( 'NONE', #7791, #18415, #34058 ) ;
#39670 = CARTESIAN_POINT ( 'NONE',  ( 0.1356587054898548694, -1.302826366429101324, -0.6902430740193704617 ) ) ;
#39671 = CARTESIAN_POINT ( 'NONE',  ( -0.2399999999999999079, -3.933118884668405979, -0.4831760564648042711 ) ) ;
#39672 = AXIS2_PLACEMENT_3D ( 'NONE', #6576, #12562, #15857 ) ;
#39673 = CARTESIAN_POINT ( 'NONE',  ( 0.2556509140510369038, -1.160232112247506109, 0.7428221499324000332 ) ) ;
#39674 = DIRECTION ( 'NONE',  ( -1.000000000000000000, 7.000205099780406914E-17, 1.387778780781449620E-15 ) ) ;
#39675 = EDGE_CURVE ( 'NONE', #8795, #5190, #18177, .T. ) ;
#39676 = DIRECTION ( 'NONE',  ( -1.000000000000000000, -0.000000000000000000, -0.000000000000000000 ) ) ;
#39677 = CARTESIAN_POINT ( 'NONE',  ( 0.1109092093543055241, -0.9286325583098424818, 0.1457252011008478843 ) ) ;
#39678 = CARTESIAN_POINT ( 'NONE',  ( -1.040834085586084010E-16, -0.01499999999999992832, -0.07499999999999977518 ) ) ;
#39679 = CARTESIAN_POINT ( 'NONE',  ( 0.3571473637288121172, -1.161317952103357865, 0.4288090205490824314 ) ) ;
#39680 = DIRECTION ( 'NONE',  ( -1.000000000000000000, -2.280301054154495132E-31, 1.664003471950577689E-31 ) ) ;
#39681 = CARTESIAN_POINT ( 'NONE',  ( 0.4093192649698302321, -1.477391824278450061, -0.5625509170971489947 ) ) ;
#39682 = PERSON_AND_ORGANIZATION ( #28500, #32463 ) ;
#39683 = EDGE_CURVE ( 'NONE', #13008, #37512, #26105, .T. ) ;
#39684 = CIRCLE ( 'NONE', #4843, 0.01000000000000002970 ) ;
#39685 = ADVANCED_FACE ( 'NONE', ( #29366 ), #11051, .F. ) ;
#39686 = CARTESIAN_POINT ( 'NONE',  ( 0.4797714183061499438, -1.117321928803942654, 0.5295840580642868778 ) ) ;
#39687 = CARTESIAN_POINT ( 'NONE',  ( 0.04230188431063326704, -0.4429734639576344279, 0.1531098457317283112 ) ) ;
#39688 = FACE_OUTER_BOUND ( 'NONE', #31966, .T. ) ;
#39689 = VECTOR ( 'NONE', #14302, 39.37007874015748854 ) ;
#39690 = AXIS2_PLACEMENT_3D ( 'NONE', #28740, #26076, #13096 ) ;
#39691 = EDGE_CURVE ( 'NONE', #7866, #14928, #35726, .T. ) ;
#39692 = APPLIED_APPROVAL_ASSIGNMENT ( #40085, ( #7895 ) ) ;
#39693 = CARTESIAN_POINT ( 'NONE',  ( 0.0002084515527543570027, -0.5213305055289283452, -0.04052408320813689208 ) ) ;
#39694 = CARTESIAN_POINT ( 'NONE',  ( 0.3979561296664244630, -2.043052950745618990, -0.5098141394919292191 ) ) ;
#39695 = CARTESIAN_POINT ( 'NONE',  ( 0.002064972446937151339, -0.4784520794224960683, 0.3149028691301604121 ) ) ;
#39696 = PLANE ( 'NONE',  #11822 ) ;
#39697 = CIRCLE ( 'NONE', #31203, 0.01499999999999995608 ) ;
#39698 = ORIENTED_EDGE ( 'NONE', *, *, #16281, .F. ) ;
#39699 = ORIENTED_EDGE ( 'NONE', *, *, #7246, .F. ) ;
#39700 = CIRCLE ( 'NONE', #6834, 0.01499999999999999077 ) ;
#39701 = CARTESIAN_POINT ( 'NONE',  ( -0.05464101615137785528, -2.198867511061768809, -0.9423512173156428640 ) ) ;
#39702 = ORIENTED_EDGE ( 'NONE', *, *, #34902, .T. ) ;
#39703 = DIRECTION ( 'NONE',  ( 9.498382610854457704E-16, -0.7692307692307690514, -0.6389710663783134681 ) ) ;
#39705 = ORIENTED_EDGE ( 'NONE', *, *, #12181, .T. ) ;
#39704 = CARTESIAN_POINT ( 'NONE',  ( -0.1044436713285761403, -0.4741860147765892819, 0.1089215716836983705 ) ) ;
#39707 = ORIENTED_EDGE ( 'NONE', *, *, #8735, .F. ) ;
#39706 = CARTESIAN_POINT ( 'NONE',  ( -0.001920489672809163684, -0.8476932489793732595, 0.09397500963053398437 ) ) ;
#39708 = ORIENTED_EDGE ( 'NONE', *, *, #23599, .F. ) ;
#39709 = ORIENTED_EDGE ( 'NONE', *, *, #16428, .F. ) ;
#39710 = CARTESIAN_POINT ( 'NONE',  ( 0.2660823795547838655, -1.675198854444863716, 0.5696963268675777625 ) ) ;
#39712 = CARTESIAN_POINT ( 'NONE',  ( 0.1323828673530924871, -1.257873181764345816, 0.6230388128859498664 ) ) ;
#39711 = DIRECTION ( 'NONE',  ( 1.000000000000000000, 0.000000000000000000, 0.000000000000000000 ) ) ;
#39713 = CARTESIAN_POINT ( 'NONE',  ( 0.3645392532257850093, -1.157254380035450447, 0.4995441290596880912 ) ) ;
#39714 = APPROVAL_DATE_TIME ( #11742, #4473 ) ;
#39715 = EDGE_CURVE ( 'NONE', #28968, #20453, #4449, .T. ) ;
#39716 = EDGE_CURVE ( 'NONE', #31635, #21929, #7425, .T. ) ;
#39717 = DIRECTION ( 'NONE',  ( -0.1871397384865028934, -0.9823333030490228879, 6.429779641674037776E-17 ) ) ;
#39719 = ORIENTED_EDGE ( 'NONE', *, *, #15527, .F. ) ;
#39718 = EDGE_LOOP ( 'NONE', ( #35255, #27937, #21094, #39604, #22587 ) ) ;
#39720 = AXIS2_PLACEMENT_3D ( 'NONE', #12062, #8969, #30374 ) ;
#39721 = CARTESIAN_POINT ( 'NONE',  ( 0.01167029684184067023, -0.7543104828189726163, -0.1044922862589389156 ) ) ;
#39722 = CARTESIAN_POINT ( 'NONE',  ( -0.2299999999999999267, 0.5182417262804744906, 0.3599999999999993205 ) ) ;
#39723 = AXIS2_PLACEMENT_3D ( 'NONE', #33896, #18872, #19065 ) ;
#39724 = CARTESIAN_POINT ( 'NONE',  ( 0.07028185168205175470, -0.5531160948379537645, 0.2188760460452662537 ) ) ;
#39725 = VECTOR ( 'NONE', #3055, 39.37007874015748143 ) ;
#39726 = CARTESIAN_POINT ( 'NONE',  ( 0.1873654698603020585, -0.6959066354592325920, 0.03335868142391257979 ) ) ;
#39727 = DIRECTION ( 'NONE',  ( 0.000000000000000000, 0.000000000000000000, -1.000000000000000000 ) ) ;
#39728 = APPLIED_SECURITY_CLASSIFICATION_ASSIGNMENT ( #33155, ( #19398 ) ) ;
#39729 = DIRECTION ( 'NONE',  ( 0.000000000000000000, -0.9629711830670020234, -0.2696043408080414094 ) ) ;
#39730 = CARTESIAN_POINT ( 'NONE',  ( 0.3857581439227468767, -1.748739094004719163, -0.4525101959494370329 ) ) ;
#39731 = DIRECTION ( 'NONE',  ( 1.000000000000000000, 0.000000000000000000, 0.000000000000000000 ) ) ;
#39732 = AXIS2_PLACEMENT_3D ( 'NONE', #27362, #33304, #5110 ) ;
#39733 = DIRECTION ( 'NONE',  ( -6.162975822039154046E-33, 0.000000000000000000, -1.000000000000000000 ) ) ;
#39734 = CARTESIAN_POINT ( 'NONE',  ( 0.4820730268389710194, -1.120100422993975275, 0.5182417262812748504 ) ) ;
#39735 = CARTESIAN_POINT ( 'NONE',  ( -0.02000000000000000042, -2.183180860297908144, -0.4937760292030871079 ) ) ;
#39736 = CARTESIAN_POINT ( 'NONE',  ( 0.01135114394058200742, -0.9404934803143812916, 0.09104275933669267462 ) ) ;
#39737 = CARTESIAN_POINT ( 'NONE',  ( 0.4363412383469720268, -1.230814285733859315, 0.5836505495634819463 ) ) ;
#39738 = CARTESIAN_POINT ( 'NONE',  ( 0.1549999999999999156, 0.000000000000000000, 0.000000000000000000 ) ) ;
#39739 = CARTESIAN_POINT ( 'NONE',  ( 0.01548846960712814240, 0.2450655194479464116, -0.4674710490748144043 ) ) ;
#39740 = CARTESIAN_POINT ( 'NONE',  ( 0.2949739106045629056, -1.710307911171992323, 0.7406796427396996618 ) ) ;
#39741 = CARTESIAN_POINT ( 'NONE',  ( 0.4319471385618090520, -1.049247276449186916, 0.6348846931381728620 ) ) ;
#39742 = CARTESIAN_POINT ( 'NONE',  ( -0.0007814672454587524896, -0.8642386026234205598, 0.3264423145784848268 ) ) ;
#39743 = APPLICATION_PROTOCOL_DEFINITION ( 'international standard', 'automotive_design', 2000, #39759 ) ;
#39744 = CARTESIAN_POINT ( 'NONE',  ( 0.6630438016670622270, -1.374754038922163080, 0.8377997132616019638 ) ) ;
#39745 = AXIS2_PLACEMENT_3D ( 'NONE', #18009, #30570, #2395 ) ;
#39746 = ADVANCED_FACE ( 'NONE', ( #7745 ), #29756, .F. ) ;
#39747 = CIRCLE ( 'NONE', #24005, 0.1000000000000000194 ) ;
#39748 = DIRECTION ( 'NONE',  ( 1.000000000000000000, -0.000000000000000000, -0.000000000000000000 ) ) ;
#39749 = LINE ( 'NONE', #33779, #14705 ) ;
#39750 = CARTESIAN_POINT ( 'NONE',  ( 0.3622253751127866295, -1.756884464425455761, -0.4902987826081470213 ) ) ;
#39751 = EDGE_LOOP ( 'NONE', ( #4135, #28647, #38052, #20156 ) ) ;
#39752 = CARTESIAN_POINT ( 'NONE',  ( 0.3402959632056916650, -1.632552626064600165, -0.5940485371126216219 ) ) ;
#39753 = APPLIED_APPROVAL_ASSIGNMENT ( #23269, ( #27300 ) ) ;
#39754 = CARTESIAN_POINT ( 'NONE',  ( 0.008711396254904512151, -0.6169322991267630618, 0.4321200063933361424 ) ) ;
#39755 = CARTESIAN_POINT ( 'NONE',  ( 0.5879381176784390650, -1.491229467720181390, 0.5734525147726333705 ) ) ;
#39756 = CARTESIAN_POINT ( 'NONE',  ( 0.3829978824168507878, -1.758159847006225407, -0.4469636835181319268 ) ) ;
#39758 = ORIENTED_EDGE ( 'NONE', *, *, #24263, .F. ) ;
#39757 = CARTESIAN_POINT ( 'NONE',  ( 0.3892048212403190210, -1.924453948264585046, -0.4980904138457005192 ) ) ;
#39759 = APPLICATION_CONTEXT ( 'configuration controlled 3d designs of mechanical parts and assemblies' ) ;
#39760 = AXIS2_PLACEMENT_3D ( 'NONE', #6534, #3466, #31450 ) ;
#39761 = CARTESIAN_POINT ( 'NONE',  ( 0.2674444507101633728, -0.7485333398656358606, 0.5795413912256205391 ) ) ;
#39763 = VERTEX_POINT ( 'NONE', #11451 ) ;
#39762 = ORIENTED_EDGE ( 'NONE', *, *, #16701, .T. ) ;
#39764 = CARTESIAN_POINT ( 'NONE',  ( 0.1517790575129573938, -1.325739146886562247, -0.7195016053274172485 ) ) ;
#39765 =( BOUNDED_SURFACE ( )  B_SPLINE_SURFACE ( 3, 2, ( 
 ( #11711, #36790, #8211 ),
 ( #17668, #39679, #20977 ),
 ( #17273, #21399, #1669 ),
 ( #36187, #11303, #2047 ) ),
 .UNSPECIFIED., .F., .F., .F. ) 
 B_SPLINE_SURFACE_WITH_KNOTS ( ( 4, 4 ),
 ( 3, 3 ),
 ( 0.01563290161724498195, 0.01614380785394589277 ),
 ( 0.8846791454767857221, 1.000000000000000000 ),
 .UNSPECIFIED. ) 
 GEOMETRIC_REPRESENTATION_ITEM ( )  RATIONAL_B_SPLINE_SURFACE ( (
 ( 0.9401556194672928690, 0.9661773532027507772, 1.000000000000000000),
 ( 0.9401609085802409282, 0.9661803424859135569, 1.000000000000000000),
 ( 0.9401662911497292718, 0.9661833845885311467, 1.000000000000000000),
 ( 0.9401715974566158263, 0.9661863835893065300, 1.000000000000000000) ) ) 
 REPRESENTATION_ITEM ( '' )  SURFACE ( )  );
#39766 = VERTEX_POINT ( 'NONE', #1996 ) ;
#39767 = CARTESIAN_POINT ( 'NONE',  ( -0.05464101615137762630, -2.004218822785767795, -0.4035264592197354561 ) ) ;
#39768 = CONTEXT_DEPENDENT_SHAPE_REPRESENTATION ( #19536, #26216 ) ;
#39769 = CARTESIAN_POINT ( 'NONE',  ( -0.2746410161513776482, -3.758594918004649621, -0.06617323996463200797 ) ) ;
#39770 = VERTEX_POINT ( 'NONE', #17620 ) ;
#39771 = CYLINDRICAL_SURFACE ( 'NONE', #13331, 0.1620173459747806799 ) ;
#39772 = CARTESIAN_POINT ( 'NONE',  ( 0.08909969736564220255, -0.7080461655569163515, 0.2259464132569931061 ) ) ;
#39773 = CARTESIAN_POINT ( 'NONE',  ( 0.3012310081014870078, -1.678279676007319310, 0.8715374191053447683 ) ) ;
#39774 = CARTESIAN_POINT ( 'NONE',  ( 0.4975585306863050117, -1.542526060902300822, 0.5750136511568909592 ) ) ;
#39776 = DIRECTION ( 'NONE',  ( 1.000000000000000000, 0.000000000000000000, 0.000000000000000000 ) ) ;
#39775 = DIRECTION ( 'NONE',  ( -1.000000000000000000, -0.000000000000000000, -0.000000000000000000 ) ) ;
#39777 = CARTESIAN_POINT ( 'NONE',  ( 0.03992535094069216833, -1.048059102012378840, 0.5962256563898924444 ) ) ;
#39778 = ORIENTED_EDGE ( 'NONE', *, *, #4117, .F. ) ;
#39779 = ORIENTED_EDGE ( 'NONE', *, *, #2725, .F. ) ;
#39780 = CARTESIAN_POINT ( 'NONE',  ( 0.3169571484440001363, -1.762177905942989398, 0.5412171649221120262 ) ) ;
#39781 = CARTESIAN_POINT ( 'NONE',  ( 0.3565767535945514877, -0.9039810230172339311, 0.7062321383356453541 ) ) ;
#39782 = CARTESIAN_POINT ( 'NONE',  ( 4.898587196589414308E-18, -0.4700000000000001954, -0.04000000000000000777 ) ) ;
#39783 = CARTESIAN_POINT ( 'NONE',  ( 0.3699999999999786793, -2.097675824466503691, -0.5028176662824495047 ) ) ;
#39784 = APPROVAL_PERSON_ORGANIZATION ( #16285, #25245, #37883 ) ;
#39785 = LENGTH_MEASURE_WITH_UNIT ( LENGTH_MEASURE( 0.02539999999999999897 ), #14688 );
#39786 = CARTESIAN_POINT ( 'NONE',  ( 0.06838828474556885029, -1.327737673307782806, 0.5330404844705093348 ) ) ;
#39787 = CARTESIAN_POINT ( 'NONE',  ( 0.2047211543538725864, -1.633415721624318362, -0.6910012992593033143 ) ) ;
#39788 = VECTOR ( 'NONE', #39239, 39.37007874015748854 ) ;
#39789 = CARTESIAN_POINT ( 'NONE',  ( 0.3178934152576730621, -1.184108536564375314, 0.5634386359574784509 ) ) ;
#39790 = CARTESIAN_POINT ( 'NONE',  ( 0.5539006188405288800, -1.190957016459229800, 0.5326915342634773731 ) ) ;
#39791 = PERSON_AND_ORGANIZATION ( #28500, #32463 ) ;
#39792 = CARTESIAN_POINT ( 'NONE',  ( 0.03113248654051816583, 0.000000000000000000, 0.000000000000000000 ) ) ;
#39793 = DIRECTION ( 'NONE',  ( -1.000000000000000000, -2.341930812374887555E-31, 1.664003471950578127E-31 ) ) ;
#39794 = ORIENTED_EDGE ( 'NONE', *, *, #12996, .T. ) ;
#39795 = EDGE_CURVE ( 'NONE', #35302, #28686, #7317, .T. ) ;
#39796 = CARTESIAN_POINT ( 'NONE',  ( 0.4542841342992246512, -1.218320695817829202, 0.6688155487934264176 ) ) ;
#39797 = DIRECTION ( 'NONE',  ( 1.000000000000000000, 0.000000000000000000, 0.000000000000000000 ) ) ;
#39798 = ADVANCED_FACE ( 'NONE', ( #35510 ), #2421, .T. ) ;
#39799 = DIRECTION ( 'NONE',  ( 1.000000000000000000, 1.450082232674701412E-15, -8.188699666868902382E-16 ) ) ;
#39800 = ORIENTED_EDGE ( 'NONE', *, *, #3168, .F. ) ;
#39801 = CARTESIAN_POINT ( 'NONE',  ( 0.1892549258828873926, -0.8411929458066104148, 0.2428197129412378030 ) ) ;
#39802 = EDGE_CURVE ( 'NONE', #7589, #8591, #22144, .T. ) ;
#39803 = CARTESIAN_POINT ( 'NONE',  ( -0.1212602504878775439, -0.5073146173917496560, 0.3749999999999995559 ) ) ;
#39804 = AXIS2_PLACEMENT_3D ( 'NONE', #27887, #12251, #27481 ) ;
#39805 = AXIS2_PLACEMENT_3D ( 'NONE', #31477, #853, #7168 ) ;
#39806 = CARTESIAN_POINT ( 'NONE',  ( -0.04229883635638087558, 0.004358580242005115520, -0.4686119955506233281 ) ) ;
#39807 = EDGE_CURVE ( 'NONE', #33695, #22635, #17012, .T. ) ;
#39808 = CARTESIAN_POINT ( 'NONE',  ( 0.2263037797473778368, -1.351310894833297915, 0.5807374671911091912 ) ) ;
#39809 = ORIENTED_EDGE ( 'NONE', *, *, #2110, .F. ) ;
#39810 = CARTESIAN_POINT ( 'NONE',  ( -0.1129900121204594904, -0.5167580615068187999, 0.1415474730880565690 ) ) ;
#39811 = CARTESIAN_POINT ( 'NONE',  ( -0.02000000000000000042, -1.765869171405739957, -0.8132390237819782097 ) ) ;
#39812 = SECURITY_CLASSIFICATION ( '', '', #18982 ) ;
#39813 = CARTESIAN_POINT ( 'NONE',  ( 0.05268932808079770241, -0.4484995728561511075, -0.1361157601095852043 ) ) ;
#39814 = CARTESIAN_POINT ( 'NONE',  ( 0.1925402117207221098, -1.964586866904750151, -0.2961055278315678496 ) ) ;
#39815 = CARTESIAN_POINT ( 'NONE',  ( 0.4653576118663421690, -1.234380357178559651, 0.6478506215840158511 ) ) ;
#39817 = CARTESIAN_POINT ( 'NONE',  ( 0.1909286924077255032, -1.257064795538239022, -0.5931747813493344346 ) ) ;
#39816 = CARTESIAN_POINT ( 'NONE',  ( 0.04047076529492525665, 0.4923674059679383208, 0.09402950075401000918 ) ) ;
#39818 = FACE_OUTER_BOUND ( 'NONE', #16364, .T. ) ;
#39819 = VERTEX_POINT ( 'NONE', #26697 ) ;
#39820 = CIRCLE ( 'NONE', #23440, 0.03749999999977557397 ) ;
#39821 = CARTESIAN_POINT ( 'NONE',  ( 0.1999999999999789724, -2.183180860297921466, -0.5437760292030870968 ) ) ;
#39822 = ORIENTED_EDGE ( 'NONE', *, *, #38075, .F. ) ;
#39823 = DIRECTION ( 'NONE',  ( 1.000000000000000000, 6.779273404243070203E-32, 4.314083075427408311E-32 ) ) ;
#39824 = CARTESIAN_POINT ( 'NONE',  ( 0.3896793708141981227, -1.455733931370364553, 0.8396294446493801633 ) ) ;
#39825 = ADVANCED_FACE ( 'NONE', ( #1599 ), #23610, .T. ) ;
#39827 = CARTESIAN_POINT ( 'NONE',  ( 0.1876235411046664192, -0.7934053227479342940, 0.2850852003878450169 ) ) ;
#39826 = DIRECTION ( 'NONE',  ( 5.551115123125759899E-17, -4.553079989440443628E-16, -1.000000000000000000 ) ) ;
#39828 = CARTESIAN_POINT ( 'NONE',  ( 0.4952252789729119642, -1.180554010857031599, 0.4224090057976987445 ) ) ;
#39829 = APPLIED_PERSON_AND_ORGANIZATION_ASSIGNMENT ( #15254, #9698, ( #4853 ) ) ;
#39830 = ORIENTED_EDGE ( 'NONE', *, *, #1678, .F. ) ;
#39831 = ORIENTED_EDGE ( 'NONE', *, *, #7422, .F. ) ;
#39832 = CARTESIAN_POINT ( 'NONE',  ( 0.1794004326756924173, -1.813331030036754887, -0.3207468061039889795 ) ) ;
#39833 = CARTESIAN_POINT ( 'NONE',  ( 0.5811665336899081158, -1.491966016390690708, 0.6316321043910979594 ) ) ;
#39834 = CARTESIAN_POINT ( 'NONE',  ( 0.5825649363837883676, -1.621069190649260694, 0.5720958814438571460 ) ) ;
#39835 = DIRECTION ( 'NONE',  ( 0.000000000000000000, 0.000000000000000000, 1.000000000000000000 ) ) ;
#39836 = DIRECTION ( 'NONE',  ( -5.879757087911781259E-34, -0.5877852522924815748, -0.8090169943749412340 ) ) ;
#39837 = CARTESIAN_POINT ( 'NONE',  ( 0.4910727179654820196, -1.657301623184578077, 0.4283731996474700598 ) ) ;
#39838 = CARTESIAN_POINT ( 'NONE',  ( -0.1522836376793811619, 0.4715211068759145308, 0.3601997132473424568 ) ) ;
#39839 = CARTESIAN_POINT ( 'NONE',  ( -0.01548846960707524721, -0.4770632572900429524, 0.2530032579707506835 ) ) ;
#39840 = B_SPLINE_CURVE_WITH_KNOTS ( 'NONE', 3,
 ( #19866, #28731, #19476, #22780, #1184, #19663 ),
 .UNSPECIFIED., .F., .F.,
 ( 4, 2, 4 ),
 ( 0.000000000000000000, 0.0007279435479977064503, 0.001455887095995412901 ),
 .UNSPECIFIED. ) ;
#39841 = AXIS2_PLACEMENT_3D ( 'NONE', #30596, #33460, #5690 ) ;
#39842 = CARTESIAN_POINT ( 'NONE',  ( 0.3632211645871377126, -0.8757803013682723403, 0.7750855204132592879 ) ) ;
#39843 = CARTESIAN_POINT ( 'NONE',  ( 0.1677396061116748216, -1.215651260229680286, 0.5182417262812423209 ) ) ;
#39844 = CARTESIAN_POINT ( 'NONE',  ( 0.003727000072687845170, -0.9627618936687203366, 0.4240455811949819243 ) ) ;
#39845 = LOCAL_TIME ( 0, 53, 7.000000000000000000, #21876 ) ;
#39846 = CARTESIAN_POINT ( 'NONE',  ( 0.6165909760827519293, -1.623179156379430887, -0.5076586781594308873 ) ) ;
#39847 = CARTESIAN_POINT ( 'NONE',  ( 0.03647060353175536618, 0.2291014149038373693, 0.4576769917029342993 ) ) ;
#39848 = ADVANCED_FACE ( 'NONE', ( #20508 ), #28699, .T. ) ;
#39849 = CARTESIAN_POINT ( 'NONE',  ( 0.6292630781544163998, -1.582461550746711909, 0.6099326772577570166 ) ) ;
#39850 = FACE_BOUND ( 'NONE', #23085, .T. ) ;
#39851 = CONICAL_SURFACE ( 'NONE', #3070, 0.5756329413417603513, 1.047197551196602738 ) ;
#39852 = DIRECTION ( 'NONE',  ( 1.000000000000000000, 0.000000000000000000, 0.000000000000000000 ) ) ;
#39853 = ADVANCED_FACE ( 'NONE', ( #8756 ), #25114, .T. ) ;
#39854 = CARTESIAN_POINT ( 'NONE',  ( 0.1818238028002573947, -0.5066057096094660483, 0.1075624334068491922 ) ) ;
#39855 = CARTESIAN_POINT ( 'NONE',  ( 0.3662247033611901181, -1.729352955075043941, -0.6047395896534266679 ) ) ;
#39856 = ADVANCED_FACE ( 'NONE', ( #28712 ), #29322, .T. ) ;
#39857 = CARTESIAN_POINT ( 'NONE',  ( 0.4262438152663739488, -1.592651821845864069, -0.6151431148613255573 ) ) ;
#39858 = CARTESIAN_POINT ( 'NONE',  ( -0.02000000000000000042, -2.644673614468930012, -0.2637721856604205439 ) ) ;
#39859 = EDGE_CURVE ( 'NONE', #8779, #34185, #4152, .T. ) ;
#39860 = EDGE_LOOP ( 'NONE', ( #28746, #29087, #6358, #24354 ) ) ;
#39861 = CARTESIAN_POINT ( 'NONE',  ( 0.4480646913441766466, -1.099213350020603386, -0.6275147848854657484 ) ) ;
#39862 = CARTESIAN_POINT ( 'NONE',  ( 0.3445304142628009547, -1.145137055011931748, 0.5942808790109807004 ) ) ;
#39863 = CARTESIAN_POINT ( 'NONE',  ( 0.1859142959171137532, -0.8501877694175364875, 0.2020740118391618767 ) ) ;
#39864 = CARTESIAN_POINT ( 'NONE',  ( -0.05283102792148818005, 0.3063958269170702353, -0.3541938269410517259 ) ) ;
#39865 = CARTESIAN_POINT ( 'NONE',  ( 0.5221384440520447923, -1.330831645065488456, 0.6091261937352400180 ) ) ;
#39867 = ORIENTED_EDGE ( 'NONE', *, *, #6675, .F. ) ;
#39866 = DIRECTION ( 'NONE',  ( 1.000000000000000000, 6.779273404243070203E-32, 4.314083075427408311E-32 ) ) ;
#39868 = CARTESIAN_POINT ( 'NONE',  ( 0.5137183020217809259, -1.118314259765692764, 0.5770968910244165251 ) ) ;
#39869 = AXIS2_PLACEMENT_3D ( 'NONE', #23984, #17984, #30548 ) ;
#39870 = ORIENTED_EDGE ( 'NONE', *, *, #30240, .T. ) ;
#39871 = CARTESIAN_POINT ( 'NONE',  ( 0.04398552291027794936, -1.506617454199507433, -0.3728714820311309630 ) ) ;
#39872 = VERTEX_POINT ( 'NONE', #19610 ) ;
#39873 = CARTESIAN_POINT ( 'NONE',  ( -0.03868649100028186127, 0.2522293598345317633, -0.4043344736883373036 ) ) ;
#39874 = ORIENTED_EDGE ( 'NONE', *, *, #10505, .F. ) ;
#39875 = CARTESIAN_POINT ( 'NONE',  ( 0.3562241851712061314, -1.622432527926769064, 0.5753824526387549820 ) ) ;
#39876 = EDGE_CURVE ( 'NONE', #9065, #21878, #31723, .T. ) ;
#39878 = CARTESIAN_POINT ( 'NONE',  ( 0.1764858099340315956, -0.5346581714635332272, -0.02636846031365289167 ) ) ;
#39877 = CARTESIAN_POINT ( 'NONE',  ( 0.7051250147666914270, -1.492378199219462465, 0.5174013405292774426 ) ) ;
#39879 = CARTESIAN_POINT ( 'NONE',  ( 0.5264113014007612001, -1.640729993778266893, -0.5166151207188711680 ) ) ;
#39880 = B_SPLINE_CURVE_WITH_KNOTS ( 'NONE', 3,
 ( #7232, #10355, #14032, #4160, #29886, #13630, #20019, #26607, #39141, #32951, #10968, #16727, #14242, #36045, #926, #26002, #38524, #26196 ),
 .UNSPECIFIED., .F., .F.,
 ( 4, 2, 2, 2, 2, 2, 2, 2, 4 ),
 ( 0.006341682393953856911, 0.007137201732907770199, 0.007932721071861683487, 0.008728240410815596775, 0.009523759749769510063, 0.01031927908872342335, 0.01111479842767733664, 0.01191031776663124993, 0.01270583710558516495 ),
 .UNSPECIFIED. ) ;
#39881 = ORIENTED_EDGE ( 'NONE', *, *, #20846, .F. ) ;
#39882 = VERTEX_POINT ( 'NONE', #38713 ) ;
#39883 = CARTESIAN_POINT ( 'NONE',  ( 0.3578131408655606527, -1.083403370911659946, 0.6388820969571129549 ) ) ;
#39884 = ORIENTED_EDGE ( 'NONE', *, *, #33368, .F. ) ;
#39885 = CARTESIAN_POINT ( 'NONE',  ( 0.000000000000000000, 0.000000000000000000, 0.000000000000000000 ) ) ;
#39886 = CARTESIAN_POINT ( 'NONE',  ( -0.02000000000000000042, -2.626773565144302935, -0.2726934094652516127 ) ) ;
#39887 = CARTESIAN_POINT ( 'NONE',  ( 0.3843371407211305657, -1.261522862150258772, 0.5682417262808739933 ) ) ;
#39888 = DIRECTION ( 'NONE',  ( 0.4999551463232371762, -0.8660512985181134660, 0.000000000000000000 ) ) ;
#39889 = CARTESIAN_POINT ( 'NONE',  ( 0.4534978277988769846, -1.047755265242954037, -0.5155029497116575543 ) ) ;
#39890 = CARTESIAN_POINT ( 'NONE',  ( 0.1316017208954911588, -1.248059642665102942, 0.5182417262812423209 ) ) ;
#39891 = DIRECTION ( 'NONE',  ( 1.000000000000000000, 1.118011712966791197E-31, -7.771561172376107616E-16 ) ) ;
#39892 = CARTESIAN_POINT ( 'NONE',  ( 0.05083665881508978718, 0.4330284998000944463, 0.1917934360576652730 ) ) ;
#39893 = CARTESIAN_POINT ( 'NONE',  ( 0.4134740292144571949, -1.130738711115819140, 0.4880408775256062093 ) ) ;
#39894 = CARTESIAN_POINT ( 'NONE',  ( -0.08000000000000000167, -1.944084441611813707, -0.4562887203618206655 ) ) ;
#39895 = CALENDAR_DATE ( 2026, 13, 10 ) ;
#39896 = CARTESIAN_POINT ( 'NONE',  ( 0.4819606849173208030, -1.119673669223240520, 0.5199609940792718765 ) ) ;
#39897 = CARTESIAN_POINT ( 'NONE',  ( 0.01548846960721225047, -0.5203207976464844231, 0.08861466064783186936 ) ) ;
#39898 = DIRECTION ( 'NONE',  ( 1.702140497302374535E-12, 0.000000000000000000, -1.000000000000000000 ) ) ;
#39899 = EDGE_CURVE ( 'NONE', #13346, #3151, #4002, .T. ) ;
#39900 = FACE_OUTER_BOUND ( 'NONE', #4538, .T. ) ;
#39901 = DIRECTION ( 'NONE',  ( 1.000000000000000000, -0.000000000000000000, -0.000000000000000000 ) ) ;
#39902 = EDGE_CURVE ( 'NONE', #36780, #13108, #10052, .T. ) ;
#39903 = CARTESIAN_POINT ( 'NONE',  ( 0.08577121655192940231, -0.8846912944720071170, 0.8606152429655203884 ) ) ;
#39904 = CARTESIAN_POINT ( 'NONE',  ( 0.3702085959188072817, -1.615317497076966813, 0.4882469897972006589 ) ) ;
#39905 = ADVANCED_FACE ( 'NONE', ( #1309 ), #33495, .T. ) ;
#39906 = ORIENTED_EDGE ( 'NONE', *, *, #39294, .F. ) ;
#39907 = ORIENTED_EDGE ( 'NONE', *, *, #23752, .T. ) ;
#39908 = CARTESIAN_POINT ( 'NONE',  ( -0.1103620673373381933, -0.5040504500049264314, 0.1035024533006822928 ) ) ;
#39909 = VERTEX_POINT ( 'NONE', #29266 ) ;
#39910 = EDGE_CURVE ( 'NONE', #2065, #29909, #234, .T. ) ;
#39911 = DIRECTION ( 'NONE',  ( 0.6377491006683481123, 0.000000000000000000, 0.7702441720628031563 ) ) ;
#39912 = LINE ( 'NONE', #24703, #29653 ) ;
#39915 = EDGE_LOOP ( 'NONE', ( #8485, #27216, #24095, #39544 ) ) ;
#39914 = B_SPLINE_CURVE_WITH_KNOTS ( 'NONE', 3,
 ( #6770, #38243, #1444, #9862, #19348, #31886, #22648 ),
 .UNSPECIFIED., .F., .F.,
 ( 4, 3, 4 ),
 ( 0.003048000018042928624, 0.003429000018037117996, 0.003810000018031183770 ),
 .UNSPECIFIED. ) ;
#39913 = CARTESIAN_POINT ( 'NONE',  ( 0.006342365902731740036, -0.8382430779231306861, 0.09710106263402516757 ) ) ;
#39916 = ORIENTED_EDGE ( 'NONE', *, *, #15477, .T. ) ;
#39917 = CARTESIAN_POINT ( 'NONE',  ( -0.2399999999999999079, -3.040459736179910166, -1.372268108520683372 ) ) ;
#39918 = ORIENTED_EDGE ( 'NONE', *, *, #15969, .T. ) ;
#39919 = EDGE_CURVE ( 'NONE', #11732, #17560, #33035, .T. ) ;
#39920 = CARTESIAN_POINT ( 'NONE',  ( -0.0005976636740459253172, -0.5552437863504529059, 0.2653367056401107482 ) ) ;
#39922 = CARTESIAN_POINT ( 'NONE',  ( 0.1617803284656291196, -1.239972288448516702, 0.6007116129271903304 ) ) ;
#39921 = CARTESIAN_POINT ( 'NONE',  ( -0.02000000000000000042, -1.599201040860868339, 0.1642182323853691728 ) ) ;
#39923 = DIRECTION ( 'NONE',  ( 0.000000000000000000, 0.000000000000000000, -1.000000000000000000 ) ) ;
#39924 = ADVANCED_FACE ( 'NONE', ( #38913 ), #5373, .F. ) ;
#39925 = DATE_AND_TIME ( #27184, #20837 ) ;
#39926 = DIRECTION ( 'NONE',  ( -1.000000000000000000, -2.280301054154495132E-31, 1.664003471950577689E-31 ) ) ;
#39928 = VERTEX_POINT ( 'NONE', #30478 ) ;
#39927 = ORIENTED_EDGE ( 'NONE', *, *, #26242, .F. ) ;
#39929 = EDGE_CURVE ( 'NONE', #17084, #2063, #903, .T. ) ;
#39930 = CARTESIAN_POINT ( 'NONE',  ( 0.3648817522660376400, -1.130029036334877279, 0.6215301754536329826 ) ) ;
#39931 = B_SPLINE_SURFACE_WITH_KNOTS ( 'NONE', 3, 1, ( 
 ( #1700, #10945 ),
 ( #33139, #36430 ),
 ( #14218, #23902 ),
 ( #20818, #13614 ) ),
 .UNSPECIFIED., .F., .F., .F.,
 ( 4, 4 ),
 ( 2, 2 ),
 ( 0.000000000000000000, 1.000000000000000000 ),
 ( 0.000000000000000000, 1.000000000000000000 ),
 .UNSPECIFIED. ) ;
#39932 = CARTESIAN_POINT ( 'NONE',  ( 0.2654586657438877673, -0.9403158806777288659, 0.7264623116330005681 ) ) ;
#39933 = CARTESIAN_POINT ( 'NONE',  ( 0.1853458231138309653, -0.8340042177779849464, 0.1270555878011652151 ) ) ;
#39934 = DIRECTION ( 'NONE',  ( 0.8660512985181134660, 0.4999551463232372317, 0.000000000000000000 ) ) ;
#39935 = DIRECTION ( 'NONE',  ( 0.4999551463232372317, -0.8660512985181135770, 0.000000000000000000 ) ) ;
#39936 = CARTESIAN_POINT ( 'NONE',  ( 0.4185715608678379218, -1.702044260100491924, -0.4179452547514317384 ) ) ;
#39937 = CARTESIAN_POINT ( 'NONE',  ( 0.3954090057121530388, -1.720129112149186845, 0.4259808212722830389 ) ) ;
#39938 = DIRECTION ( 'NONE',  ( -0.4999551463232333459, 0.8660512985181156864, 0.000000000000000000 ) ) ;
#39939 = CARTESIAN_POINT ( 'NONE',  ( 0.2409193767872376546, -1.343661558146008073, -0.2869361388274795921 ) ) ;
#39940 = CARTESIAN_POINT ( 'NONE',  ( 0.4190882504452823620, -1.118891637760769830, 0.5995514612943967370 ) ) ;
#39941 = DIRECTION ( 'NONE',  ( 0.8660512985181140211, 0.4999551463232362880, 0.000000000000000000 ) ) ;
#39942 = CARTESIAN_POINT ( 'NONE',  ( -0.02000000000000000042, -1.968175500587574067, -0.6048844944454191408 ) ) ;
#39943 = CARTESIAN_POINT ( 'NONE',  ( 0.03474859143381433396, -0.6982915424597320175, 0.6540940360414806420 ) ) ;
#39944 = CARTESIAN_POINT ( 'NONE',  ( 0.05991778417293673609, -1.332687696286689594, 0.5682717497416263086 ) ) ;
#39945 = COORDINATED_UNIVERSAL_TIME_OFFSET ( 0, 0, .AHEAD. ) ;
#39946 = CARTESIAN_POINT ( 'NONE',  ( 0.7224934542336318710, -1.479659627397842403, 0.5766931279523788145 ) ) ;
#39947 = ADVANCED_FACE ( 'NONE', ( #27801 ), #10697, .F. ) ;
#39948 = CARTESIAN_POINT ( 'NONE',  ( 0.4149016700119600998, -1.651544695139487429, -0.6216189332891878250 ) ) ;
#39949 = EDGE_CURVE ( 'NONE', #23858, #5039, #25592, .T. ) ;
#39950 = CARTESIAN_POINT ( 'NONE',  ( 0.03301162916267656733, 0.08829475514027847194, -0.5134720893088496885 ) ) ;
#39951 = CARTESIAN_POINT ( 'NONE',  ( 0.3526243232178313258, -1.728525448788969410, -0.4459625336182188593 ) ) ;
#39952 = ORIENTED_EDGE ( 'NONE', *, *, #160, .F. ) ;
#39953 = CARTESIAN_POINT ( 'NONE',  ( -0.08000000000000000167, -2.314906514113384883, -0.5881050943081593818 ) ) ;
#39954 = CARTESIAN_POINT ( 'NONE',  ( 0.01685698302946367702, -0.6256804056397152758, 0.4269450335313899059 ) ) ;
#39955 = CARTESIAN_POINT ( 'NONE',  ( 0.1285611044470676978, -0.5511077305290806860, 0.1614518025332021822 ) ) ;
#39956 = CARTESIAN_POINT ( 'NONE',  ( 0.3804922947572159653, -1.758905690526931354, -0.4436857796392575382 ) ) ;
#39958 = VERTEX_POINT ( 'NONE', #30688 ) ;
#39957 = DIRECTION ( 'NONE',  ( 0.4999551463232372317, -0.8660512985181135770, 0.000000000000000000 ) ) ;
#39959 = CARTESIAN_POINT ( 'NONE',  ( 0.1943341254738605584, -0.5992045414336306663, 0.2618067726929366734 ) ) ;
#39961 = ORIENTED_EDGE ( 'NONE', *, *, #13141, .F. ) ;
#39960 = ORIENTED_EDGE ( 'NONE', *, *, #35578, .F. ) ;
#39962 = CARTESIAN_POINT ( 'NONE',  ( 0.6927131938946141654, -1.422842782059151157, 0.6785767152737546271 ) ) ;
#39963 = FACE_BOUND ( 'NONE', #37431, .T. ) ;
#39964 = CARTESIAN_POINT ( 'NONE',  ( 0.000000000000000000, -0.02999999999999995379, 0.000000000000000000 ) ) ;
#39965 = CONTEXT_DEPENDENT_SHAPE_REPRESENTATION ( #32135, #32438 ) ;
#39966 = CARTESIAN_POINT ( 'NONE',  ( -0.05078493045284175611, 0.4330747843660931462, -0.1920285438095961916 ) ) ;
#39967 = ORIENTED_EDGE ( 'NONE', *, *, #18481, .F. ) ;
#39968 = CARTESIAN_POINT ( 'NONE',  ( 0.1645055737317709932, -0.8154898342693455149, 0.5663631941838773720 ) ) ;
#39969 = CARTESIAN_POINT ( 'NONE',  ( 0.3201253347856640175, -1.704124430139120072, 0.8372518665352793876 ) ) ;
#39970 = CARTESIAN_POINT ( 'NONE',  ( 0.09934153309614388028, -0.5690506854145357396, 0.2508956654826926536 ) ) ;
#39972 = CARTESIAN_POINT ( 'NONE',  ( 0.001312449538768875905, -0.5612271264025527895, 0.03476213731316191852 ) ) ;
#39971 = CARTESIAN_POINT ( 'NONE',  ( 0.3352399569063156393, -1.753319872000470792, 0.4596133135264604541 ) ) ;
#39973 = CARTESIAN_POINT ( 'NONE',  ( 0.03908111062118940771, -1.198967014588472102, 0.6667909696853414614 ) ) ;
#39974 = EDGE_LOOP ( 'NONE', ( #31170, #20061, #36167, #9454 ) ) ;
#39975 = VERTEX_POINT ( 'NONE', #20830 ) ;
#39976 = CARTESIAN_POINT ( 'NONE',  ( 0.1499999999999994948, 0.3880410510314791783, 0.3755318131854940567 ) ) ;
#39977 = CARTESIAN_POINT ( 'NONE',  ( 0.3967191919388743382, -0.9324009735222377193, 0.8071385964775494859 ) ) ;
#39978 = DIRECTION ( 'NONE',  ( 1.000000000000000000, 0.000000000000000000, 0.000000000000000000 ) ) ;
#39979 = CARTESIAN_POINT ( 'NONE',  ( 0.4687631324631791330, -1.116557084650701359, 0.5688798658794104179 ) ) ;
#39980 = CARTESIAN_POINT ( 'NONE',  ( 0.6841302653033145553, -1.411212316466117223, 0.6057417262805112612 ) ) ;
#39981 = CARTESIAN_POINT ( 'NONE',  ( 0.07991135521492878646, -1.395945580162383459, -0.6589646420266501714 ) ) ;
#39982 = CARTESIAN_POINT ( 'NONE',  ( 0.3246143735900494653, -1.168538765758894371, 0.4697788401231595690 ) ) ;
#39983 = B_SPLINE_CURVE_WITH_KNOTS ( 'NONE', 3,
 ( #15738, #38352, #10190, #7077, #22758, #1555, #35683, #38751, #13266, #10796, #4204, #7483, #23565, #32182, #29317, #16769, #20062, #35283 ),
 .UNSPECIFIED., .F., .F.,
 ( 4, 2, 2, 2, 2, 2, 2, 2, 4 ),
 ( 0.000000000000000000, 0.0003722439366697991980, 0.0007444878733395983959, 0.001116731810009397594, 0.001488975746679196792, 0.001861219683348995990, 0.002233463620018795188, 0.002605707556688594169, 0.002977951493358393584 ),
 .UNSPECIFIED. ) ;
#39984 = CARTESIAN_POINT ( 'NONE',  ( 0.5505100836374232642, -1.180854739677868359, 0.6191363254822006557 ) ) ;
#39985 = DATE_AND_TIME ( #11623, #37115 ) ;
#39986 = CARTESIAN_POINT ( 'NONE',  ( 0.6184971854324693430, -1.588153737519645281, 0.6167571325555825101 ) ) ;
#39987 = B_SPLINE_CURVE_WITH_KNOTS ( 'NONE', 5,
 ( #8677, #17345, #30286, #29902, #20645, #2119 ),
 .UNSPECIFIED., .F., .F.,
 ( 6, 6 ),
 ( 4.822244625248871763, 7.710395699062019936 ),
 .UNSPECIFIED. ) ;
#39988 = CARTESIAN_POINT ( 'NONE',  ( 0.3699999999999784572, -2.097675824466503691, -0.5196396315034579327 ) ) ;
#39989 = DIRECTION ( 'NONE',  ( -0.4999551463232372317, 0.8660512985181135770, -0.000000000000000000 ) ) ;
#39990 = CARTESIAN_POINT ( 'NONE',  ( -0.03171102739523560393, -0.3312744048890958193, -0.3635303745205933357 ) ) ;
#39991 =( BOUNDED_SURFACE ( )  B_SPLINE_SURFACE ( 3, 2, ( 
 ( #34490, #37368, #27926 ),
 ( #18444, #19067, #37178 ),
 ( #15764, #182, #15977 ),
 ( #30995, #15368, #37983 ),
 ( #9793, #28312, #40465 ),
 ( #37560, #5883, #6303 ),
 ( #18657, #24847, #31603 ),
 ( #12290, #9179, #21747 ),
 ( #34279, #8995, #6088 ),
 ( #9599, #12675, #31216 ) ),
 .UNSPECIFIED., .F., .F., .T. ) 
 B_SPLINE_SURFACE_WITH_KNOTS ( ( 4, 2, 2, 2, 4 ),
 ( 3, 3 ),
 ( -9.757819552369539906E-18, 0.0004973432167690072835, 0.0009946864335380243248, 0.001492029650307041475, 0.001989372867076058624 ),
 ( 0.000000000000000000, 1.000000000000000000 ),
 .UNSPECIFIED. ) 
 GEOMETRIC_REPRESENTATION_ITEM ( )  RATIONAL_B_SPLINE_SURFACE ( (
 ( 1.000000000000000000, 0.8897565210026132654, 1.000000000000000000),
 ( 1.000000000000000000, 0.8899231130074136686, 1.000000000000000000),
 ( 1.000000000000000000, 0.8890122559934640067, 1.000000000000000000),
 ( 1.000000000000000000, 0.8849579905325665186, 1.000000000000000000),
 ( 1.000000000000000000, 0.8818374620091549154, 1.000000000000000000),
 ( 1.000000000000000000, 0.8735256406124205508, 1.000000000000000000),
 ( 1.000000000000000000, 0.8682786441878931338, 1.000000000000000000),
 ( 1.000000000000000000, 0.8559483198610358112, 1.000000000000000000),
 ( 1.000000000000000000, 0.8487295818195398356, 1.000000000000000000),
 ( 1.000000000000000000, 0.8407181564550617603, 1.000000000000000000) ) ) 
 REPRESENTATION_ITEM ( '' )  SURFACE ( )  );
#39992 = ORIENTED_EDGE ( 'NONE', *, *, #19248, .T. ) ;
#39993 = DIRECTION ( 'NONE',  ( 0.8660512985181132439, 0.4999551463232376758, 0.000000000000000000 ) ) ;
#39994 = CARTESIAN_POINT ( 'NONE',  ( 0.08510361377861434817, -0.8106636051554854117, 0.1454306519311501233 ) ) ;
#39995 = ORIENTED_EDGE ( 'NONE', *, *, #39802, .T. ) ;
#39996 = CARTESIAN_POINT ( 'NONE',  ( -0.03877220711930245978, -0.03321538116298394100, -0.4752084053751546855 ) ) ;
#39997 = CARTESIAN_POINT ( 'NONE',  ( 0.1533772736604412101, -1.181689746394253726, 0.7533906142735892209 ) ) ;
#39999 = ORIENTED_EDGE ( 'NONE', *, *, #40410, .T. ) ;
#39998 = ORIENTED_EDGE ( 'NONE', *, *, #14433, .F. ) ;
#40000 = CARTESIAN_POINT ( 'NONE',  ( -0.03662792686184391383, 0.2484399233013421804, 0.4119056456069879468 ) ) ;
#40001 = CARTESIAN_POINT ( 'NONE',  ( 0.01896931156525286447, -0.07379981600433808964, 0.5147676832640479816 ) ) ;
#40002 = CARTESIAN_POINT ( 'NONE',  ( 0.05561375719525332717, -0.4442396019574900712, -0.1228845301467967194 ) ) ;
#40003 = CARTESIAN_POINT ( 'NONE',  ( 0.3690773559837012274, -2.063460311930843449, -0.4759771606218671236 ) ) ;
#40004 = CARTESIAN_POINT ( 'NONE',  ( 0.4711122148191352887, -1.243347910189986916, 0.6355297091942355703 ) ) ;
#40006 = CARTESIAN_POINT ( 'NONE',  ( -0.0004431470427073231017, -0.9367128829938298207, 0.1457185332388704069 ) ) ;
#40005 = CARTESIAN_POINT ( 'NONE',  ( 0.02238765564325780749, 0.5044129532808500072, 0.09031612285224414893 ) ) ;
#40007 = CARTESIAN_POINT ( 'NONE',  ( -0.2746410161513779258, -2.139295658456680904, -0.2024034539465678073 ) ) ;
#40008 = VERTEX_POINT ( 'NONE', #26981 ) ;
#40009 = ORIENTED_EDGE ( 'NONE', *, *, #15699, .F. ) ;
#40010 = CARTESIAN_POINT ( 'NONE',  ( 0.06545186104482746126, -1.329499349160038868, 0.5176190731536282064 ) ) ;
#40011 = VERTEX_POINT ( 'NONE', #2307 ) ;
#40012 = CARTESIAN_POINT ( 'NONE',  ( 0.1861675601333642183, -0.7337134285967986669, -0.03797464539687132185 ) ) ;
#40013 = CARTESIAN_POINT ( 'NONE',  ( 0.3382961071825119070, -1.342601817737219205, 0.8746150539162650395 ) ) ;
#40015 = CARTESIAN_POINT ( 'NONE',  ( -0.02953079040095700838, 0.000000000000000000, 0.000000000000000000 ) ) ;
#40014 = DIRECTION ( 'NONE',  ( 0.9966814372958092694, 0.000000000000000000, 0.08140093703367154432 ) ) ;
#40016 = CARTESIAN_POINT ( 'NONE',  ( -0.08978098643734171158, -7.148474850891705974E-16, -0.3698489655878013371 ) ) ;
#40017 = VERTEX_POINT ( 'NONE', #218 ) ;
#40018 = CARTESIAN_POINT ( 'NONE',  ( -0.2746410161513782033, -2.323257895298838971, -0.7902071827178637209 ) ) ;
#40019 = ORIENTED_EDGE ( 'NONE', *, *, #13923, .F. ) ;
#40020 = CARTESIAN_POINT ( 'NONE',  ( 0.4011831001776828831, -1.742810116944001786, -0.5289609113168958210 ) ) ;
#40021 = CARTESIAN_POINT ( 'NONE',  ( 0.1311121416671343076, -0.6135371899443636812, 0.3487476746206483735 ) ) ;
#40022 = CARTESIAN_POINT ( 'NONE',  ( 0.4696177048947446919, -1.669690955150979095, 0.4747328526538268645 ) ) ;
#40023 = CARTESIAN_POINT ( 'NONE',  ( -0.1088121136105144049, -0.4964308608213456875, 0.1000000000000000194 ) ) ;
#40024 = CARTESIAN_POINT ( 'NONE',  ( -0.03664605387828157035, 0.4684681574363449008, 0.1090337349854993559 ) ) ;
#40025 = CARTESIAN_POINT ( 'NONE',  ( 0.2147974912797966929, -1.231358751133227347, 0.5546678855025314325 ) ) ;
#40026 = CARTESIAN_POINT ( 'NONE',  ( 0.2135845999631697523, -1.238000303071007613, 0.5636751376830327898 ) ) ;
#40027 = B_SPLINE_CURVE_WITH_KNOTS ( 'NONE', 3,
 ( #16982, #38370, #35298, #38982, #589, #38579, #10398, #22563, #35481, #25638, #26446, #19268, #23389, #16788, #1181, #31808, #3623, #16188 ),
 .UNSPECIFIED., .F., .F.,
 ( 4, 2, 2, 2, 2, 2, 2, 2, 4 ),
 ( 0.0003425652276237324957, 0.001007165397454245050, 0.001671765567284757767, 0.002336365737115270267, 0.003000965906945782767, 0.003665566076776295267, 0.004330166246606808635, 0.004994766416437320701, 0.005659366586267833635 ),
 .UNSPECIFIED. ) ;
#40028 = CYLINDRICAL_SURFACE ( 'NONE', #38465, 0.02999999999999998848 ) ;
#40029 = CARTESIAN_POINT ( 'NONE',  ( 0.1969702849860160421, -0.5469408226469265610, 0.3272831088336244365 ) ) ;
#40030 = CARTESIAN_POINT ( 'NONE',  ( -0.03478556507500542988, 0.3590471004907105912, 0.3712136264428257948 ) ) ;
#40031 = CARTESIAN_POINT ( 'NONE',  ( -0.1667650433730323567, 0.4848728453260168769, 0.3315300532330299199 ) ) ;
#40032 = CARTESIAN_POINT ( 'NONE',  ( 0.6536459824712800293, -1.536535929646544618, -0.4156460142788562795 ) ) ;
#40033 = CARTESIAN_POINT ( 'NONE',  ( 0.4781934768423676818, -1.682642038360962600, -0.6151431148613257793 ) ) ;
#40034 = CARTESIAN_POINT ( 'NONE',  ( 0.5996218235215466930, -1.599608852905763712, 0.6078077878447281091 ) ) ;
#40035 = CARTESIAN_POINT ( 'NONE',  ( 0.6568730927750874304, -1.460570608776338597, 0.4224083929475443977 ) ) ;
#40036 = CARTESIAN_POINT ( 'NONE',  ( 0.3748245490824459458, -1.104718531341411625, -0.5155029497116575543 ) ) ;
#40037 = ADVANCED_FACE ( 'NONE', ( #17713 ), #1907, .T. ) ;
#40038 = ORIENTED_EDGE ( 'NONE', *, *, #38870, .T. ) ;
#40039 = APPROVAL ( #20868, 'UNKNOWN' ) ;
#40040 = CARTESIAN_POINT ( 'NONE',  ( 0.3653812862022917662, -1.748582203572395466, -0.5147731941186001192 ) ) ;
#40041 = CARTESIAN_POINT ( 'NONE',  ( 0.4132813002760061249, -1.705586778321113384, -0.6106085670228335038 ) ) ;
#40042 = DIRECTION ( 'NONE',  ( 0.000000000000000000, 0.000000000000000000, -1.000000000000000000 ) ) ;
#40043 = CARTESIAN_POINT ( 'NONE',  ( 0.3699999999999786238, -2.086845765202261394, -0.4708431600348449431 ) ) ;
#40044 = ORIENTED_EDGE ( 'NONE', *, *, #32634, .T. ) ;
#40045 = CARTESIAN_POINT ( 'NONE',  ( 0.4145109374026955673, -1.110466390532955927, 0.6153597435504403190 ) ) ;
#40046 = CARTESIAN_POINT ( 'NONE',  ( 0.3332542364016487513, -1.159914367434109694, 0.5808425792736833237 ) ) ;
#40047 = CARTESIAN_POINT ( 'NONE',  ( 0.07414957964017190872, -1.324282773101342459, 0.5611483367411455037 ) ) ;
#40048 = FACE_OUTER_BOUND ( 'NONE', #38741, .T. ) ;
#40049 = CARTESIAN_POINT ( 'NONE',  ( 0.4819304095161658363, -1.265165726648666666, 0.7071056013453563827 ) ) ;
#40051 = CARTESIAN_POINT ( 'NONE',  ( -0.2399999999999999079, -4.320736256378554963, -0.8145269479932405465 ) ) ;
#40050 = DIRECTION ( 'NONE',  ( 0.000000000000000000, 2.731847993664262824E-15, -1.000000000000000000 ) ) ;
#40052 = CARTESIAN_POINT ( 'NONE',  ( 0.5055437690763310288, -1.106959495255247505, 0.6108412925465283028 ) ) ;
#40053 = EDGE_LOOP ( 'NONE', ( #26419, #7748 ) ) ;
#40054 = DATE_AND_TIME ( #5711, #38495 ) ;
#40055 = CARTESIAN_POINT ( 'NONE',  ( 0.4634712904840416203, -1.711704060178988129, -0.5155029497116575543 ) ) ;
#40056 = ORIENTED_EDGE ( 'NONE', *, *, #7371, .F. ) ;
#40057 = CARTESIAN_POINT ( 'NONE',  ( -0.01548846960721238578, 0.2450655194478933985, -0.4674710490746305513 ) ) ;
#40058 = CARTESIAN_POINT ( 'NONE',  ( 0.03564512600577746798, -0.5402024432579285440, 0.1944966300737278331 ) ) ;
#40060 = CARTESIAN_POINT ( 'NONE',  ( 0.1754821060578101444, -0.7911127963077850822, -0.05965230147901675467 ) ) ;
#40059 = CARTESIAN_POINT ( 'NONE',  ( -0.2746410161513779258, -2.423474325126674156, -0.5576739111151496342 ) ) ;
#40061 = CARTESIAN_POINT ( 'NONE',  ( 0.1768282059192854694, -1.460166703081138273, -0.3235079468584903251 ) ) ;
#40062 = VECTOR ( 'NONE', #36993, 39.37007874015748854 ) ;
#40063 = ORIENTED_EDGE ( 'NONE', *, *, #2201, .T. ) ;
#40064 = CARTESIAN_POINT ( 'NONE',  ( 0.4532541167939423410, -1.052918095400384502, 0.6353596524208835472 ) ) ;
#40065 = CARTESIAN_POINT ( 'NONE',  ( 0.5530491884521703261, -1.511199273475291704, 0.5743520122765221059 ) ) ;
#40066 = VERTEX_POINT ( 'NONE', #27197 ) ;
#40067 = CARTESIAN_POINT ( 'NONE',  ( -0.2399999999999999079, -3.318147336744930342, -0.6877918253319055264 ) ) ;
#40068 = ADVANCED_FACE ( 'NONE', ( #17528 ), #12713, .T. ) ;
#40069 = FACE_OUTER_BOUND ( 'NONE', #513, .T. ) ;
#40070 = CIRCLE ( 'NONE', #34814, 0.01500000000000002200 ) ;
#40071 = CARTESIAN_POINT ( 'NONE',  ( 0.02901502440408285088, -1.579081040833445249, -0.3765017618882691153 ) ) ;
#40072 = EDGE_CURVE ( 'NONE', #10513, #2583, #6093, .T. ) ;
#40073 = CARTESIAN_POINT ( 'NONE',  ( -0.1208133668958207424, -0.5051731972035693463, 0.3159170889047836495 ) ) ;
#40074 = ADVANCED_FACE ( 'NONE', ( #11564 ), #13797, .F. ) ;
#40075 = EDGE_CURVE ( 'NONE', #2630, #2835, #23196, .T. ) ;
#40076 = DIRECTION ( 'NONE',  ( -0.7451425084519979203, 0.000000000000000000, -0.6669052722072786876 ) ) ;
#40077 = CARTESIAN_POINT ( 'NONE',  ( 0.5698035129313328007, -1.613887348078733019, 0.3667417262808780887 ) ) ;
#40078 = FACE_OUTER_BOUND ( 'NONE', #31565, .T. ) ;
#40079 = DIRECTION ( 'NONE',  ( 0.000000000000000000, 0.000000000000000000, 1.000000000000000000 ) ) ;
#40080 = APPLICATION_PROTOCOL_DEFINITION ( 'international standard', 'automotive_design', 2000, #15854 ) ;
#40081 = CARTESIAN_POINT ( 'NONE',  ( 0.4254375920900159702, -1.133939855871281654, 0.4364855428459707976 ) ) ;
#40082 = CARTESIAN_POINT ( 'NONE',  ( 0.02231181081520441575, -0.4612879682509028467, 0.2235517164227180942 ) ) ;
#40083 = PLANE ( 'NONE',  #31739 ) ;
#40084 = ADVANCED_FACE ( 'NONE', ( #29373 ), #12652, .T. ) ;
#40085 = APPROVAL ( #7388, 'UNSPECIFIED' ) ;
#40086 = CARTESIAN_POINT ( 'NONE',  ( 0.01185072000139549518, -0.5792930532549652733, -0.08974618506422621378 ) ) ;
#40087 = CARTESIAN_POINT ( 'NONE',  ( -0.2399999999999999079, -3.335205990917129881, -0.4042613180508733972 ) ) ;
#40088 = CARTESIAN_POINT ( 'NONE',  ( 0.003526303896849130280, -0.4943637263100597035, 0.3555042333582821845 ) ) ;
#40089 = CARTESIAN_POINT ( 'NONE',  ( 0.3625960434667531151, -1.762758894398492204, -0.5926935080085831142 ) ) ;
#40090 = ORIENTED_EDGE ( 'NONE', *, *, #35307, .T. ) ;
#40091 = ORIENTED_EDGE ( 'NONE', *, *, #27560, .T. ) ;
#40092 = CIRCLE ( 'NONE', #15798, 0.1000000000000000194 ) ;
#40093 = CARTESIAN_POINT ( 'NONE',  ( -0.1055448275397422725, -0.4799318856336941552, 0.3601683063145876273 ) ) ;
#40094 = ORIENTED_EDGE ( 'NONE', *, *, #277, .F. ) ;
#40095 = DIRECTION ( 'NONE',  ( 0.000000000000000000, 0.000000000000000000, 1.000000000000000000 ) ) ;
#40096 = CARTESIAN_POINT ( 'NONE',  ( -0.1154362047091238019, -0.5278818619436607129, 0.1319635891398989735 ) ) ;
#40098 = ORIENTED_EDGE ( 'NONE', *, *, #4969, .T. ) ;
#40097 = CARTESIAN_POINT ( 'NONE',  ( 0.002240231740626892794, -0.5288788276447421444, 0.1275514325127009851 ) ) ;
#40099 = ADVANCED_FACE ( 'NONE', ( #32043 ), #21874, .F. ) ;
#40100 = EDGE_CURVE ( 'NONE', #17948, #27939, #29106, .T. ) ;
#40101 = VERTEX_POINT ( 'NONE', #623 ) ;
#40102 = DIRECTION ( 'NONE',  ( -2.686534417925922091E-31, 0.5877852522924700285, -0.8090169943749496717 ) ) ;
#40103 = SHAPE_REPRESENTATION ( 'Parallelogram front_FRONT', ( #27819 ), #33063 ) ;
#40104 = EDGE_LOOP ( 'NONE', ( #27659, #11083, #8035, #16991 ) ) ;
#40105 = CARTESIAN_POINT ( 'NONE',  ( 0.002070590758578906478, -0.5820978177397124753, 0.3347319319685872485 ) ) ;
#40107 = CARTESIAN_POINT ( 'NONE',  ( 0.1519872515161661553, -1.248741164724253894, 0.6214439643266400637 ) ) ;
#40106 = CARTESIAN_POINT ( 'NONE',  ( 0.4351293263873937667, -1.231514889939106849, 0.5832342842089121016 ) ) ;
#40108 = CARTESIAN_POINT ( 'NONE',  ( 0.2776126715564697367, -1.634751399283275175, -0.3585985592053876903 ) ) ;
#40109 = DATE_AND_TIME ( #39313, #34593 ) ;
#40110 = CARTESIAN_POINT ( 'NONE',  ( 0.4778170654558047126, -1.668016138613298560, 0.5682417262808788783 ) ) ;
#40112 = ORIENTED_EDGE ( 'NONE', *, *, #33769, .T. ) ;
#40111 = VERTEX_POINT ( 'NONE', #29160 ) ;
#40113 = CARTESIAN_POINT ( 'NONE',  ( 0.3289569715009816875, -1.175130748077982012, 0.5862253151572544008 ) ) ;
#40114 = CARTESIAN_POINT ( 'NONE',  ( 0.3681699996139363162, -1.734736572097494323, 0.4293946410173364869 ) ) ;
#40115 = CARTESIAN_POINT ( 'NONE',  ( -0.03174036153403787114, -0.5170813853140128202, 0.08825077997795215123 ) ) ;
#40116 = EDGE_CURVE ( 'NONE', #13190, #37440, #35005, .T. ) ;
#40117 = CARTESIAN_POINT ( 'NONE',  ( 0.5267604045959165537, -1.342330622345534685, 0.7955128641744203533 ) ) ;
#40118 = CARTESIAN_POINT ( 'NONE',  ( 0.1871516419350925109, -0.7106192216159855635, 0.03078494767255909870 ) ) ;
#40119 = DIRECTION ( 'NONE',  ( -7.771561172376107616E-16, 7.170354002788761615E-17, -1.000000000000000000 ) ) ;
#40120 = CARTESIAN_POINT ( 'NONE',  ( 0.2435586465554056279, -1.522308288314433655, 0.8982978177552802812 ) ) ;
#40121 = ADVANCED_FACE ( 'NONE', ( #16225 ), #25151, .T. ) ;
#40122 = VECTOR ( 'NONE', #30345, 39.37007874015748143 ) ;
#40123 = CARTESIAN_POINT ( 'NONE',  ( 0.2534765463136028352, -1.439939349519022693, 1.023019129304256758 ) ) ;
#40124 = CARTESIAN_POINT ( 'NONE',  ( 0.4070925130139965153, -1.744250469367210288, -0.5784223492323977700 ) ) ;
#40125 = EDGE_CURVE ( 'NONE', #15479, #10881, #10437, .T. ) ;
#40126 = CARTESIAN_POINT ( 'NONE',  ( 0.3811251628308546802, -1.654782503697128870, -0.6335434503995712729 ) ) ;
#40127 = CARTESIAN_POINT ( 'NONE',  ( -0.2399999999999999079, -3.941790907013290823, -0.4709369376873030477 ) ) ;
#40128 = AXIS2_PLACEMENT_3D ( 'NONE', #25923, #29190, #28974 ) ;
#40129 = DIRECTION ( 'NONE',  ( 0.8660512985181134660, 0.4999551463232372317, 0.000000000000000000 ) ) ;
#40130 = DIRECTION ( 'NONE',  ( 0.000000000000000000, 0.000000000000000000, -1.000000000000000000 ) ) ;
#40131 = DIRECTION ( 'NONE',  ( -1.000000000000000000, -7.857794173099924470E-32, -8.628166150854818811E-32 ) ) ;
#40132 = AXIS2_PLACEMENT_3D ( 'NONE', #17451, #4880, #36968 ) ;
#40133 = CIRCLE ( 'NONE', #15829, 0.01500000000000002373 ) ;
#40134 = DIRECTION ( 'NONE',  ( -1.000000000000000000, -0.000000000000000000, -0.000000000000000000 ) ) ;
#40135 = CARTESIAN_POINT ( 'NONE',  ( 0.1835387414513457993, -1.269102812158692473, 1.002600033288329140 ) ) ;
#40136 = CARTESIAN_POINT ( 'NONE',  ( 0.09673638787972767272, -1.284069476777787822, 0.7393371349209389987 ) ) ;
#40137 = APPROVAL_ROLE ( '' ) ;
#40138 = CARTESIAN_POINT ( 'NONE',  ( 0.7188893830798498419, -1.468416639873279861, 0.6609592937859087858 ) ) ;
#40139 = EDGE_CURVE ( 'NONE', #17084, #1239, #31082, .T. ) ;
#40140 = EDGE_CURVE ( 'NONE', #11376, #35222, #19101, .T. ) ;
#40141 = CARTESIAN_POINT ( 'NONE',  ( 0.7063157497510277327, -1.525259356795145127, 0.5664836816230577332 ) ) ;
#40142 = CARTESIAN_POINT ( 'NONE',  ( 0.04285640132274089187, -0.07199195674533706568, -0.4895487002729275727 ) ) ;
#40143 = DIRECTION ( 'NONE',  ( 0.000000000000000000, 0.000000000000000000, -1.000000000000000000 ) ) ;
#40144 = EDGE_LOOP ( 'NONE', ( #25514, #4406, #34648, #20401 ) ) ;
#40145 = CARTESIAN_POINT ( 'NONE',  ( -0.1499999999999996336, 5.828670879282072084E-17, 0.1749999999999999889 ) ) ;
#40146 = CARTESIAN_POINT ( 'NONE',  ( 0.2051436026844577765, -1.420721181919286646, 0.9359180069770434152 ) ) ;
#40147 = VECTOR ( 'NONE', #4031, 39.37007874015748143 ) ;
#40148 = CARTESIAN_POINT ( 'NONE',  ( 0.5887033537614668743, -1.489407499613006003, 0.6187394134856357697 ) ) ;
#40150 = EDGE_LOOP ( 'NONE', ( #844, #33737, #35507, #10605, #25804, #15383, #32763 ) ) ;
#40149 = FACE_OUTER_BOUND ( 'NONE', #34398, .T. ) ;
#40151 = CIRCLE ( 'NONE', #32933, 0.01499999999999996649 ) ;
#40152 = CARTESIAN_POINT ( 'NONE',  ( 0.1927699586607699855, -0.5931527414817471255, 0.2350819919684725701 ) ) ;
#40154 = VERTEX_POINT ( 'NONE', #31640 ) ;
#40153 = VERTEX_POINT ( 'NONE', #25275 ) ;
#40155 = CARTESIAN_POINT ( 'NONE',  ( 0.3676236827432866061, -0.9197762930895730937, 0.7185230970922997784 ) ) ;
#40156 = AXIS2_PLACEMENT_3D ( 'NONE', #20869, #21054, #33390 ) ;
#40157 = DIRECTION ( 'NONE',  ( 0.000000000000000000, 0.000000000000000000, -1.000000000000000000 ) ) ;
#40158 = CARTESIAN_POINT ( 'NONE',  ( 0.3186313696869653711, -1.760405484422319367, 0.5654039123650882459 ) ) ;
#40159 = PERSON_AND_ORGANIZATION_ROLE ( 'classification_officer' ) ;
#40160 = VECTOR ( 'NONE', #17554, 39.37007874015748143 ) ;
#40161 = CARTESIAN_POINT ( 'NONE',  ( 0.000000000000000000, 0.1369749717427355129, -0.1457321416712075435 ) ) ;
#40162 = ORIENTED_EDGE ( 'NONE', *, *, #37872, .F. ) ;
#40163 = CARTESIAN_POINT ( 'NONE',  ( 0.08755603795678691681, -0.7055197249887150690, 0.1887500319921082692 ) ) ;
#40164 = CARTESIAN_POINT ( 'NONE',  ( 0.3100815786102045224, -1.704140726556199192, 0.8491805645699977978 ) ) ;
#40165 = CARTESIAN_POINT ( 'NONE',  ( 0.1062697735069367821, -0.5760192370515179183, 0.2670765053398264643 ) ) ;
#40167 = CARTESIAN_POINT ( 'NONE',  ( 0.08016251834805442067, -1.309203902574839207, 0.5631135398343307674 ) ) ;
#40166 = CARTESIAN_POINT ( 'NONE',  ( 0.3246612779430983475, -1.768063379345279795, 0.5167178742723262941 ) ) ;
#40168 = CARTESIAN_POINT ( 'NONE',  ( -0.03650581953630603615, -0.3643937567481967954, 0.3592734714612051961 ) ) ;
#40169 = EDGE_LOOP ( 'NONE', ( #39506, #17461, #24979, #25778 ) ) ;
#40170 = ORIENTED_EDGE ( 'NONE', *, *, #35400, .T. ) ;
#40171 = ADVANCED_FACE ( 'NONE', ( #9826 ), #32349, .T. ) ;
#40172 = CARTESIAN_POINT ( 'NONE',  ( 0.3467295405477267001, -1.741324348151121360, 0.4554588174254002308 ) ) ;
#40173 = CARTESIAN_POINT ( 'NONE',  ( 0.6552418622445979057, -1.362413096819954594, 0.8455477964343599551 ) ) ;
#40174 = CARTESIAN_POINT ( 'NONE',  ( 0.1399999999999994582, 0.000000000000000000, 0.000000000000000000 ) ) ;
#40175 = DIRECTION ( 'NONE',  ( 0.3181970600707382246, -0.9480245940703960761, 3.970578237956065974E-16 ) ) ;
#40176 = CIRCLE ( 'NONE', #15904, 0.06000000000000031697 ) ;
#40177 = CARTESIAN_POINT ( 'NONE',  ( 0.3798895702152447762, -1.759032899055416266, -0.4429027949815931287 ) ) ;
#40178 = CARTESIAN_POINT ( 'NONE',  ( 0.2719170612657579311, -1.671617796861691874, 0.5389836619028499642 ) ) ;
#40179 = CARTESIAN_POINT ( 'NONE',  ( 0.3387784160096277142, -1.171947433235863700, 0.4559352600701537805 ) ) ;
#40180 = CARTESIAN_POINT ( 'NONE',  ( 0.5367554652047751285, -1.159747519872984300, 0.6504567231333411303 ) ) ;
#40181 = APPROVAL_DATE_TIME ( #12416, #14697 ) ;
#40182 = AXIS2_PLACEMENT_3D ( 'NONE', #13014, #2944, #35008 ) ;
#40183 = TOROIDAL_SURFACE ( 'NONE', #38224, 0.1333070866141732314, 0.02999999999999999889 ) ;
#40184 = CARTESIAN_POINT ( 'NONE',  ( -0.2746410161513782033, -1.962518963160043706, -0.3791801492432049780 ) ) ;
#40185 = EDGE_CURVE ( 'NONE', #38637, #22034, #20576, .T. ) ;
#40186 = AXIS2_PLACEMENT_3D ( 'NONE', #22680, #19765, #28830 ) ;
#40187 = APPROVAL ( #10946, 'UNKNOWN' ) ;
#40188 = CARTESIAN_POINT ( 'NONE',  ( 0.3665398960025421093, -2.019035390486545900, -0.6774619758396681624 ) ) ;
#40189 = ADVANCED_FACE ( 'NONE', ( #19695 ), #12022, .T. ) ;
#40190 = CARTESIAN_POINT ( 'NONE',  ( 2.048885995248197414E-16, 0.2900000000000004796, -5.122214988120493288E-16 ) ) ;
#40191 = DIRECTION ( 'NONE',  ( -0.9378410757839558132, 0.3470650033817761493, 0.000000000000000000 ) ) ;
#40192 = ORIENTED_EDGE ( 'NONE', *, *, #34631, .T. ) ;
#40193 = CARTESIAN_POINT ( 'NONE',  ( -0.2900000000000002576, 0.5182417262804744906, 0.09999999999999993616 ) ) ;
#40194 = CARTESIAN_POINT ( 'NONE',  ( -0.03474824846560015112, -0.3591470389155407283, 0.3712557345097503569 ) ) ;
#40195 = CARTESIAN_POINT ( 'NONE',  ( -0.01548846960721259221, -0.2450655194478906784, 0.4674710490746316616 ) ) ;
#40196 = EDGE_LOOP ( 'NONE', ( #4531, #24674, #9628, #26413 ) ) ;
#40197 = CARTESIAN_POINT ( 'NONE',  ( -0.02242905165738916587, -0.06991915049797610415, -0.5075494376218483428 ) ) ;
#40198 = CARTESIAN_POINT ( 'NONE',  ( 0.04446389708692845971, -0.9676817186006311244, 0.6578482448476006272 ) ) ;
#40200 = ORIENTED_EDGE ( 'NONE', *, *, #35990, .F. ) ;
#40199 = ORIENTED_EDGE ( 'NONE', *, *, #9781, .T. ) ;
#40201 = CARTESIAN_POINT ( 'NONE',  ( -2.115421433687637455E-14, -2.107936428766274073, -0.7005084057759867200 ) ) ;
#40202 = CARTESIAN_POINT ( 'NONE',  ( 0.1857430203655688061, -0.8056635886342108366, 0.2698372336795828996 ) ) ;
#40203 = CARTESIAN_POINT ( 'NONE',  ( 0.03875673594170444408, -0.4416908594619144979, -0.1785163973046066388 ) ) ;
#40204 = CARTESIAN_POINT ( 'NONE',  ( 0.3607082371247617436, -1.790100760104569311, -0.5255749062586634324 ) ) ;
#40205 = CARTESIAN_POINT ( 'NONE',  ( 0.3926032618789407347, -1.756026311479913948, -0.5284552501753293496 ) ) ;
#40206 = VECTOR ( 'NONE', #3068, 39.37007874015748143 ) ;
#40208 = CARTESIAN_POINT ( 'NONE',  ( -0.2399999999999999079, -1.774602679190314669, -0.1233179098656094347 ) ) ;
#40207 = DIRECTION ( 'NONE',  ( -0.4999551463232349002, 0.8660512985181147982, 0.000000000000000000 ) ) ;
#40209 = CARTESIAN_POINT ( 'NONE',  ( -2.775557561562891351E-16, -0.02999999999999982195, -0.1999999999999994837 ) ) ;
#40210 = VERTEX_POINT ( 'NONE', #4047 ) ;
#40211 = DIRECTION ( 'NONE',  ( -0.8660254037844401509, 0.2957393706636063380, 0.4031602964572422731 ) ) ;
#40212 = VERTEX_POINT ( 'NONE', #38617 ) ;
#40213 = CIRCLE ( 'NONE', #15261, 0.1749999999999999889 ) ;
#40214 = CARTESIAN_POINT ( 'NONE',  ( 0.000000000000000000, 0.000000000000000000, 0.000000000000000000 ) ) ;
#40215 = AXIS2_PLACEMENT_3D ( 'NONE', #7006, #14194, #19573 ) ;
#40216 = CARTESIAN_POINT ( 'NONE',  ( 0.4418554096259977859, -1.573809027168237229, 0.5761839767669477697 ) ) ;
#40218 = CARTESIAN_POINT ( 'NONE',  ( 0.5911745308593184811, -1.601329302922394060, 0.4457227088930317827 ) ) ;
#40217 = CARTESIAN_POINT ( 'NONE',  ( -0.2399999999999999079, -2.407646569606659792, -0.8438593182631384249 ) ) ;
#40219 = FACE_OUTER_BOUND ( 'NONE', #18462, .T. ) ;
#40220 = CARTESIAN_POINT ( 'NONE',  ( 0.3699999999999786793, -2.143487347926988917, -0.5325376609224018454 ) ) ;
#40221 = VERTEX_POINT ( 'NONE', #19900 ) ;
#40222 = EDGE_CURVE ( 'NONE', #31015, #37794, #10877, .T. ) ;
#40223 = CARTESIAN_POINT ( 'NONE',  ( 0.06444297064315794576, -0.8352831487901670737, 0.1457185332388703236 ) ) ;
#40224 = CARTESIAN_POINT ( 'NONE',  ( 0.3958974862128058492, -2.004956072359079133, -0.2856428411439917436 ) ) ;
#40225 = CARTESIAN_POINT ( 'NONE',  ( 0.1237348556611498201, -0.5762697135983080310, 0.2583543961155602697 ) ) ;
#40226 = CARTESIAN_POINT ( 'NONE',  ( 0.4325092394784135763, -1.691959258954059964, 0.4228211183897995218 ) ) ;
#40227 = CARTESIAN_POINT ( 'NONE',  ( 0.5264113014007820723, -1.640729993778254014, 0.5682417262808777680 ) ) ;
#40228 = ORIENTED_EDGE ( 'NONE', *, *, #39578, .F. ) ;
#40229 = DIRECTION ( 'NONE',  ( -1.000000000000000000, -2.280301054154495132E-31, 1.664003471950577689E-31 ) ) ;
#40230 = CARTESIAN_POINT ( 'NONE',  ( 0.2059273467974223892, -1.283046334493782137, -0.3404751839154473436 ) ) ;
#40231 = CARTESIAN_POINT ( 'NONE',  ( -0.1530296545635674021, 0.4740172026173952724, 0.3600612075995240913 ) ) ;
#40232 = DIRECTION ( 'NONE',  ( 0.000000000000000000, 0.000000000000000000, -1.000000000000000000 ) ) ;
#40233 = CARTESIAN_POINT ( 'NONE',  ( 0.6809224168725948045, -1.405736369044236378, 0.6042223006942389896 ) ) ;
#40234 =( BOUNDED_SURFACE ( )  B_SPLINE_SURFACE ( 3, 2, ( 
 ( #6381, #18524, #34154 ),
 ( #37653, #40115, #5965 ),
 ( #3106, #31485, #5772 ),
 ( #22049, #27405, #34577 ),
 ( #24917, #18949, #18327 ),
 ( #5564, #3292, #27795 ),
 ( #40539, #18127, #33969 ),
 ( #36829, #31079, #2901 ),
 ( #11747, #15451, #24304 ),
 ( #30682, #2498, #11946 ),
 ( #8642, #24509, #28004 ),
 ( #40329, #12361, #15649 ),
 ( #37444, #37041, #28198 ),
 ( #15235, #21442, #30873 ),
 ( #2691, #9255, #12159 ),
 ( #21833, #6174, #18743 ),
 ( #38469, #13156, #482 ),
 ( #3508, #12766, #26147 ),
 ( #32483, #12977, #38253 ),
 ( #3716, #15847, #16064 ),
 ( #6991, #38661, #22249 ),
 ( #16456, #25327, #10083 ) ),
 .UNSPECIFIED., .F., .F., .F. ) 
 B_SPLINE_SURFACE_WITH_KNOTS ( ( 4, 2, 2, 2, 2, 2, 2, 2, 2, 2, 4 ),
 ( 3, 3 ),
 ( 0.002013519961495850458, 0.002780892266055759107, 0.003548264570615668190, 0.004315636875175577272, 0.004699323027455531814, 0.005083009179735486355, 0.005466695332015440896, 0.005850381484295395437, 0.006617753788855304520, 0.007385126093415213602, 0.008152498397975122685 ),
 ( 0.000000000000000000, 1.000000000000000000 ),
 .UNSPECIFIED. ) 
 GEOMETRIC_REPRESENTATION_ITEM ( )  RATIONAL_B_SPLINE_SURFACE ( (
 ( 1.000000000000000000, 0.7283825911960394306, 1.000000000000000000),
 ( 1.000000000000000000, 0.7404375345927917129, 1.000000000000000000),
 ( 1.000000000000000000, 0.7521483142434843838, 1.000000000000000000),
 ( 1.000000000000000000, 0.7744460733777613903, 1.000000000000000000),
 ( 1.000000000000000000, 0.7845612039381936187, 1.000000000000000000),
 ( 1.000000000000000000, 0.8022035258262242285, 1.000000000000000000),
 ( 1.000000000000000000, 0.8093965293321873089, 1.000000000000000000),
 ( 1.000000000000000000, 0.8169028692725408547, 1.000000000000000000),
 ( 1.000000000000000000, 0.8188329634862903106, 1.000000000000000000),
 ( 1.000000000000000000, 0.8214004505364509434, 1.000000000000000000),
 ( 1.000000000000000000, 0.8220602406260716366, 1.000000000000000000),
 ( 1.000000000000000000, 0.8220736605435879918, 1.000000000000000000),
 ( 1.000000000000000000, 0.8214126668415060450, 1.000000000000000000),
 ( 1.000000000000000000, 0.8188520474558917961, 1.000000000000000000),
 ( 1.000000000000000000, 0.8169545908334260309, 1.000000000000000000),
 ( 1.000000000000000000, 0.8094771004219962762, 1.000000000000000000),
 ( 1.000000000000000000, 0.8022723753805990343, 1.000000000000000000),
 ( 1.000000000000000000, 0.7845733350638980363, 1.000000000000000000),
 ( 1.000000000000000000, 0.7744472902492880451, 1.000000000000000000),
 ( 1.000000000000000000, 0.7522916829163881491, 1.000000000000000000),
 ( 1.000000000000000000, 0.7403553004665528459, 1.000000000000000000),
 ( 1.000000000000000000, 0.7283825911960415400, 1.000000000000000000) ) ) 
 REPRESENTATION_ITEM ( '' )  SURFACE ( )  );
#40235 = CARTESIAN_POINT ( 'NONE',  ( -0.05634115714581192091, 0.2655021207500444236, 0.3743162705049740135 ) ) ;
#40236 = DIRECTION ( 'NONE',  ( 0.4999551463232372317, -0.8660512985181135770, 0.000000000000000000 ) ) ;
#40237 = AXIS2_PLACEMENT_3D ( 'NONE', #1909, #26986, #30481 ) ;
#40238 = CARTESIAN_POINT ( 'NONE',  ( 0.6348547142568438106, -1.593451324377852751, -0.4417161348974741886 ) ) ;
#40239 = DIRECTION ( 'NONE',  ( -0.4999551463232373427, 0.8660512985181134660, -0.000000000000000000 ) ) ;
#40240 = CARTESIAN_POINT ( 'NONE',  ( 0.6038480862555802853, -1.597583055984439504, 0.5993263282456581242 ) ) ;
#40241 = DIRECTION ( 'NONE',  ( 0.000000000000000000, 0.000000000000000000, -1.000000000000000000 ) ) ;
#40242 = CARTESIAN_POINT ( 'NONE',  ( 0.1499999999999996336, -0.2372406987223574237, 0.4850946823762633531 ) ) ;
#40243 = AXIS2_PLACEMENT_3D ( 'NONE', #8835, #5318, #11918 ) ;
#40244 = ORIENTED_EDGE ( 'NONE', *, *, #7018, .F. ) ;
#40245 = CARTESIAN_POINT ( 'NONE',  ( 0.3597460184446273357, -1.737228056197862802, -0.5031880851714581881 ) ) ;
#40246 = CARTESIAN_POINT ( 'NONE',  ( 0.3711010767056441284, -1.714876091213238807, -0.6102747157238272990 ) ) ;
#40247 = CIRCLE ( 'NONE', #12647, 0.02999999999999995726 ) ;
#40248 = CARTESIAN_POINT ( 'NONE',  ( 0.2772481421372381960, -1.634119940283012662, -0.3262497153171022291 ) ) ;
#40249 = ADVANCED_FACE ( 'NONE', ( #22398 ), #18008, .F. ) ;
#40250 = CARTESIAN_POINT ( 'NONE',  ( -0.05464101615137796630, -1.682484669133182953, -0.03683853088544706417 ) ) ;
#40252 = ORIENTED_EDGE ( 'NONE', *, *, #11210, .F. ) ;
#40251 = B_SPLINE_SURFACE_WITH_KNOTS ( 'NONE', 3, 3, ( 
 ( #22941, #10378, #10175, #3795, #20050, #13253, #25610 ),
 ( #35059, #38140, #28696, #23358, #9964, #38553, #13654 ),
 ( #16350, #955, #19445, #13466, #3984, #35457, #28886 ),
 ( #22744, #6868, #35669, #35272, #31981, #10568, #747 ),
 ( #26031, #7259, #7691, #7068, #7472, #19833, #25821 ),
 ( #32582, #19639, #31775, #16159, #29306, #1153, #26220 ),
 ( #38742, #4398, #16954, #26420, #29499, #1339, #38955 ) ),
 .UNSPECIFIED., .F., .F., .F.,
 ( 4, 1, 1, 1, 4 ),
 ( 4, 1, 1, 1, 4 ),
 ( 0.000000000000000000, 0.2500000000000000000, 0.5000000000000000000, 0.7500000000000000000, 1.000000000000000000 ),
 ( 0.000000000000000000, 0.05000000000000037748, 0.1666666666666666574, 0.5555555555555555802, 1.000000000000000000 ),
 .UNSPECIFIED. ) ;
#40253 = DIRECTION ( 'NONE',  ( 1.000000000000000000, 1.448788479720436075E-15, -8.229804381843896237E-16 ) ) ;
#40254 = CIRCLE ( 'NONE', #4106, 0.02999999999999994685 ) ;
#40255 = CARTESIAN_POINT ( 'NONE',  ( -0.2399999999999999079, -3.609310082097819894, -0.4498340178114252352 ) ) ;
#40256 = CARTESIAN_POINT ( 'NONE',  ( 0.3267351042122170202, -1.764838374829281742, 0.4935885800319553263 ) ) ;
#40257 = CARTESIAN_POINT ( 'NONE',  ( 0.05561375719525540190, 0.2541477197272165589, -0.3845235600768820428 ) ) ;
#40258 = CARTESIAN_POINT ( 'NONE',  ( 0.5271251199429588530, -1.338340238819080819, 0.6479144337828351974 ) ) ;
#40260 = CARTESIAN_POINT ( 'NONE',  ( 0.4997267776899617653, -1.607290330535514178, -0.6302284990903240791 ) ) ;
#40259 = CARTESIAN_POINT ( 'NONE',  ( -0.1638686671686047092, 0.5092269732922271031, 0.1413937977834339998 ) ) ;
#40261 = CARTESIAN_POINT ( 'NONE',  ( 0.2392493758066867593, -0.9067917679836680067, 0.4646394045636887959 ) ) ;
#40262 = ORIENTED_EDGE ( 'NONE', *, *, #26595, .T. ) ;
#40263 = PERSON_AND_ORGANIZATION ( #28500, #32463 ) ;
#40264 = CARTESIAN_POINT ( 'NONE',  ( 0.1239988516143644831, -1.317835488908686292, -0.3462032427497062081 ) ) ;
#40265 = EDGE_LOOP ( 'NONE', ( #10979, #7065, #5756, #12242 ) ) ;
#40266 = CARTESIAN_POINT ( 'NONE',  ( 0.009983477080391305741, -0.5455653694289525069, 0.07572401711799378599 ) ) ;
#40267 = CARTESIAN_POINT ( 'NONE',  ( 0.03656494915825564407, -0.5581536149038067718, 0.2534570078657710224 ) ) ;
#40269 = CARTESIAN_POINT ( 'NONE',  ( 0.1759098769117282413, -0.6728151866080555044, -0.08429024728173926950 ) ) ;
#40268 = CYLINDRICAL_SURFACE ( 'NONE', #4646, 0.2200000000000000566 ) ;
#40270 = LINE ( 'NONE', #30821, #27378 ) ;
#40271 = B_SPLINE_CURVE_WITH_KNOTS ( 'NONE', 3,
 ( #4099, #32486, #26332, #16666 ),
 .UNSPECIFIED., .F., .F.,
 ( 4, 4 ),
 ( 0.000000000000000000, 0.0002307501183058325222 ),
 .UNSPECIFIED. ) ;
#40272 = VECTOR ( 'NONE', #31253, 39.37007874015748854 ) ;
#40273 = ORIENTED_EDGE ( 'NONE', *, *, #20957, .F. ) ;
#40274 = ORIENTED_EDGE ( 'NONE', *, *, #25629, .F. ) ;
#40275 = CARTESIAN_POINT ( 'NONE',  ( 0.3144151427965208301, -1.049253354087126500, 0.6307772725301707961 ) ) ;
#40276 = CARTESIAN_POINT ( 'NONE',  ( 0.5541385590046753462, -1.509386730049579572, 0.6214236857019725946 ) ) ;
#40277 = ORIENTED_EDGE ( 'NONE', *, *, #32789, .T. ) ;
#40278 = CARTESIAN_POINT ( 'NONE',  ( 0.2145146395178117171, -1.464440183438808774, -0.3485064432216347097 ) ) ;
#40279 = DIRECTION ( 'NONE',  ( 0.000000000000000000, 0.000000000000000000, 1.000000000000000000 ) ) ;
#40280 = AXIS2_PLACEMENT_3D ( 'NONE', #24692, #37223, #9041 ) ;
#40281 = CIRCLE ( 'NONE', #14673, 0.07999999999999996003 ) ;
#40282 = CARTESIAN_POINT ( 'NONE',  ( 0.2842326993135958491, -1.549395603922553155, -0.7208999815284671264 ) ) ;
#40283 = CARTESIAN_POINT ( 'NONE',  ( 0.5963593927077359691, -1.484732018227884254, -0.3901058962264565833 ) ) ;
#40284 = CIRCLE ( 'NONE', #268, 0.1000000000000000194 ) ;
#40285 = DIRECTION ( 'NONE',  ( 0.8660512985181133550, 0.4999551463232373982, 0.000000000000000000 ) ) ;
#40286 = CARTESIAN_POINT ( 'NONE',  ( 0.3912168351225406848, -1.712565751828606153, 0.4687417262808791230 ) ) ;
#40287 = DIRECTION ( 'NONE',  ( 0.000000000000000000, 0.6595282642760668113, 0.7516797646744246553 ) ) ;
#40288 = CIRCLE ( 'NONE', #6781, 0.5302738246768101682 ) ;
#40289 = CARTESIAN_POINT ( 'NONE',  ( 0.2484857473122376870, -1.339293634572156000, -0.5155029497116575543 ) ) ;
#40290 = CARTESIAN_POINT ( 'NONE',  ( 0.08096179802327445330, -1.367098532309424685, 0.5880770290185818316 ) ) ;
#40291 = PERSON_AND_ORGANIZATION ( #28500, #32463 ) ;
#40292 = CARTESIAN_POINT ( 'NONE',  ( 0.4561653094204668468, -1.131358138958592718, 0.4538444256416698241 ) ) ;
#40293 = CARTESIAN_POINT ( 'NONE',  ( 0.4670621156540841756, -1.236494891586305211, 0.6057417262809811076 ) ) ;
#40294 = CARTESIAN_POINT ( 'NONE',  ( -0.3000000000000000999, -2.109195954094405856, -0.3137251058216021793 ) ) ;
#40295 = CARTESIAN_POINT ( 'NONE',  ( 0.01926973937230214845, -1.027504089262102349, 0.6199911605063174180 ) ) ;
#40296 = CARTESIAN_POINT ( 'NONE',  ( 0.3369441150334460677, -1.754019818956965127, 0.4603468005407844177 ) ) ;
#40297 = VECTOR ( 'NONE', #18507, 39.37007874015748143 ) ;
#40298 = CARTESIAN_POINT ( 'NONE',  ( 0.3161418316428721287, -1.757545499489290286, 0.4995718330220786374 ) ) ;
#40299 = B_SPLINE_CURVE_WITH_KNOTS ( 'NONE', 3,
 ( #19524, #29778, #20133, #4466, #17226, #10446, #16418, #823, #39243, #7335, #23625, #32661, #38426, #13546, #4273, #13334, #38818, #26293, #10647, #10267, #22830, #29383, #23438, #35349, #1037, #35532, #23222, #35747, #3865, #7559, #29573, #7761, #7141, #1619 ),
 .UNSPECIFIED., .F., .F.,
 ( 4, 2, 2, 2, 2, 2, 2, 2, 2, 2, 2, 2, 2, 2, 2, 2, 4 ),
 ( 0.001574216056284313391, 0.002349730643885267114, 0.003125245231486220836, 0.003900759819087174559, 0.004676274406688128715, 0.005451788994289081570, 0.006227303581890041365, 0.007002818169491000291, 0.007778332757091959218, 0.008553847344692918145, 0.009329361932293877072, 0.01010487651989483773, 0.01088039110749579666, 0.01165590569509675559, 0.01243142028269771451, 0.01320693487029867517, 0.01398244945789963410 ),
 .UNSPECIFIED. ) ;
#40300 = CARTESIAN_POINT ( 'NONE',  ( 0.3827388732655720438, -1.608087253622227042, 0.5083331137473884320 ) ) ;
#40301 = EDGE_CURVE ( 'NONE', #14410, #10166, #39577, .T. ) ;
#40302 = ORIENTED_EDGE ( 'NONE', *, *, #15770, .T. ) ;
#40303 = EDGE_CURVE ( 'NONE', #22699, #2897, #40254, .T. ) ;
#40304 = AXIS2_PLACEMENT_3D ( 'NONE', #26061, #4812, #26859 ) ;
#40305 = ORIENTED_EDGE ( 'NONE', *, *, #22571, .F. ) ;
#40306 = VECTOR ( 'NONE', #21759, 39.37007874015748143 ) ;
#40307 = CARTESIAN_POINT ( 'NONE',  ( -0.1150001097501270886, -0.4761628310996519065, 0.1178658437129749409 ) ) ;
#40308 = VERTEX_POINT ( 'NONE', #12457 ) ;
#40309 = CARTESIAN_POINT ( 'NONE',  ( -0.1455608194604306738, -0.5249067277714107860, 0.3749999999999996669 ) ) ;
#40310 = DIRECTION ( 'NONE',  ( 1.000000000000000000, 0.000000000000000000, 0.000000000000000000 ) ) ;
#40311 = EDGE_CURVE ( 'NONE', #7871, #21046, #27117, .T. ) ;
#40312 = CARTESIAN_POINT ( 'NONE',  ( -0.1105199412302043521, -0.5049077968913552317, 0.1209919789212128283 ) ) ;
#40314 = ORIENTED_EDGE ( 'NONE', *, *, #37343, .F. ) ;
#40313 = CARTESIAN_POINT ( 'NONE',  ( 0.001331136673900325858, -0.5599312581362586583, 0.03624264176424291106 ) ) ;
#40315 = EDGE_CURVE ( 'NONE', #34414, #7674, #3014, .T. ) ;
#40316 = ORIENTED_EDGE ( 'NONE', *, *, #28021, .F. ) ;
#40317 = FACE_OUTER_BOUND ( 'NONE', #21438, .T. ) ;
#40318 = ORIENTED_EDGE ( 'NONE', *, *, #13039, .T. ) ;
#40319 = AXIS2_PLACEMENT_3D ( 'NONE', #27673, #1696, #10515 ) ;
#40320 = CARTESIAN_POINT ( 'NONE',  ( 0.005043818368537927865, -0.6038779608865681992, 0.3826815526081347452 ) ) ;
#40322 = CARTESIAN_POINT ( 'NONE',  ( 0.09680642637387373850, -1.309618686966848466, 0.5813006354277100440 ) ) ;
#40321 = CARTESIAN_POINT ( 'NONE',  ( 0.1021712152378831950, -0.8583302296959987032, 0.4405693860677040719 ) ) ;
#40323 = CARTESIAN_POINT ( 'NONE',  ( -0.05464101615137761936, -2.041899626011815183, -0.6359449730384926225 ) ) ;
#40324 = CARTESIAN_POINT ( 'NONE',  ( -0.05464101615137796630, -1.622350287959229087, -0.009600792027532436754 ) ) ;
#40326 = ORIENTED_EDGE ( 'NONE', *, *, #8172, .F. ) ;
#40325 = ORIENTED_EDGE ( 'NONE', *, *, #16488, .F. ) ;
#40327 = CARTESIAN_POINT ( 'NONE',  ( 0.4492124018919768091, -1.095000438762474770, -0.4070882247511642960 ) ) ;
#40328 = DIRECTION ( 'NONE',  ( -1.000000000000000000, 0.000000000000000000, 0.000000000000000000 ) ) ;
#40329 = CARTESIAN_POINT ( 'NONE',  ( -0.04230258372739791051, -0.4443637212174513795, 0.1488268768076328463 ) ) ;
#40330 = CARTESIAN_POINT ( 'NONE',  ( 0.2258291083026367774, -0.8976967229642250912, 0.6721174698541964032 ) ) ;
#40331 = ADVANCED_FACE ( 'NONE', ( #8972 ), #5140, .T. ) ;
#40332 = CARTESIAN_POINT ( 'NONE',  ( -0.01548846960707477016, 0.4770632572900484480, 0.2530032579707400253 ) ) ;
#40333 = CARTESIAN_POINT ( 'NONE',  ( 0.5136163780680810254, -1.682756243065421264, -0.4473473192910925600 ) ) ;
#40334 = APPROVAL ( #30, 'UNSPECIFIED' ) ;
#40335 = CIRCLE ( 'NONE', #27219, 0.1020173459747800854 ) ;
#40336 = CARTESIAN_POINT ( 'NONE',  ( -0.1112019842995528446, -0.5080904053907921991, 0.3498664773290688923 ) ) ;
#40337 = CIRCLE ( 'NONE', #25918, 0.08000000000000002942 ) ;
#40338 = CARTESIAN_POINT ( 'NONE',  ( 0.4500303265696325439, -1.093663202047157501, -0.4076127662389720796 ) ) ;
#40339 = CARTESIAN_POINT ( 'NONE',  ( 0.5698035129313328007, -1.613887348078733019, 0.3667417262808780887 ) ) ;
#40340 = VECTOR ( 'NONE', #28979, 39.37007874015748143 ) ;
#40341 = CARTESIAN_POINT ( 'NONE',  ( -0.2399999999999999079, -3.196602950345407645, -0.1969487268370971322 ) ) ;
#40342 = FACE_OUTER_BOUND ( 'NONE', #19978, .T. ) ;
#40343 = DIRECTION ( 'NONE',  ( 0.8660512985181126888, 0.4999551463232385085, 0.000000000000000000 ) ) ;
#40344 = CARTESIAN_POINT ( 'NONE',  ( 0.02242113575389428556, -0.7151737931810984161, 0.5646644402375310401 ) ) ;
#40345 = B_SPLINE_CURVE_WITH_KNOTS ( 'NONE', 3,
 ( #11850, #15746, #39838, #40231, #11661, #24220, #24417 ),
 .UNSPECIFIED., .F., .F.,
 ( 4, 3, 4 ),
 ( 0.000000000000000000, 0.0001987961317490854899, 0.0002262042107145686282 ),
 .UNSPECIFIED. ) ;
#40346 = VECTOR ( 'NONE', #19477, 39.37007874015748143 ) ;
#40347 = CARTESIAN_POINT ( 'NONE',  ( 0.06590158485999333959, -1.101506299248170118, 0.7509233284053542512 ) ) ;
#40348 = APPROVAL_STATUS ( 'not_yet_approved' ) ;
#40349 = CARTESIAN_POINT ( 'NONE',  ( 0.5877184641988779656, -1.252861897328551022, 0.8491679911058225283 ) ) ;
#40350 = AXIS2_PLACEMENT_3D ( 'NONE', #4914, #7997, #20574 ) ;
#40351 = CARTESIAN_POINT ( 'NONE',  ( 0.6834792670387838109, -1.548921872613369777, 0.5978341875930145433 ) ) ;
#40352 = CARTESIAN_POINT ( 'NONE',  ( 0.03875673594170000319, 0.03328920108827214397, -0.4752375706209732154 ) ) ;
#40353 = ADVANCED_FACE ( 'NONE', ( #30979 ), #2803, .T. ) ;
#40354 =( BOUNDED_SURFACE ( )  B_SPLINE_SURFACE ( 3, 2, ( 
 ( #11595, #36682, #24158 ),
 ( #8488, #5389, #17950 ),
 ( #15074, #27627, #8901 ),
 ( #10467, #28982, #24758 ),
 ( #13354, #26134, #2939 ),
 ( #31336, #12590, #10287 ),
 ( #23034, #18568, #16647 ),
 ( #32261, #21663, #37474 ),
 ( #25930, #12391, #40372 ),
 ( #94, #37280, #12199 ),
 ( #25150, #15681, #18978 ),
 ( #3321, #7161, #22089 ),
 ( #34190, #13567, #28044 ),
 ( #19728, #35560, #4080 ) ),
 .UNSPECIFIED., .F., .F., .F. ) 
 B_SPLINE_SURFACE_WITH_KNOTS ( ( 4, 2, 2, 2, 2, 2, 4 ),
 ( 3, 3 ),
 ( -4.206704429243757204E-17, 0.0004898451933843076282, 0.0009796903867686573234, 0.001959380773537356714, 0.002939071160306055887, 0.003428916353690405691, 0.003918761547074755061 ),
 ( 0.000000000000000000, 1.000000000000000000 ),
 .UNSPECIFIED. ) 
 GEOMETRIC_REPRESENTATION_ITEM ( )  RATIONAL_B_SPLINE_SURFACE ( (
 ( 1.000000000000000000, 0.9252764552802091869, 1.000000000000000000),
 ( 1.000000000000000000, 0.9190038079521950509, 1.000000000000000000),
 ( 1.000000000000000000, 0.9096443980271025076, 1.000000000000000000),
 ( 1.000000000000000000, 0.8863278643288117209, 1.000000000000000000),
 ( 1.000000000000000000, 0.8722306840293051478, 1.000000000000000000),
 ( 1.000000000000000000, 0.8255155620659062610, 1.000000000000000000),
 ( 1.000000000000000000, 0.7882493034320124936, 1.000000000000000000),
 ( 1.000000000000000000, 0.7036029670101283662, 1.000000000000000000),
 ( 1.000000000000000000, 0.6557983909466532646, 1.000000000000000000),
 ( 1.000000000000000000, 0.5799777945462297746, 1.000000000000000000),
 ( 1.000000000000000000, 0.5540012513858809662, 1.000000000000000000),
 ( 1.000000000000000000, 0.5013758867234165972, 1.000000000000000000),
 ( 1.000000000000000000, 0.4747208180995389215, 1.000000000000000000),
 ( 1.000000000000000000, 0.4483291926237085723, 1.000000000000000000) ) ) 
 REPRESENTATION_ITEM ( '' )  SURFACE ( )  );
#40355 = CARTESIAN_POINT ( 'NONE',  ( 0.3397077535880360100, -1.654685348432988645, -0.3858274525146624390 ) ) ;
#40356 = VERTEX_POINT ( 'NONE', #28110 ) ;
#40357 = DIRECTION ( 'NONE',  ( -1.387778780781449423E-15, 6.590151126658376924E-16, -1.000000000000000000 ) ) ;
#40358 = CARTESIAN_POINT ( 'NONE',  ( 0.2492448580361798227, -1.564264300073486602, 0.8870779812646237827 ) ) ;
#40359 = CONICAL_SURFACE ( 'NONE', #10801, 0.1400000000000007350, 1.047197551196601184 ) ;
#40360 = EDGE_CURVE ( 'NONE', #24591, #34235, #27797, .T. ) ;
#40361 = CARTESIAN_POINT ( 'NONE',  ( 0.5881849326769416075, -1.491250579143394317, 0.5780151184862688529 ) ) ;
#40363 = ORIENTED_EDGE ( 'NONE', *, *, #40593, .F. ) ;
#40362 = DIRECTION ( 'NONE',  ( 0.000000000000000000, 0.000000000000000000, -1.000000000000000000 ) ) ;
#40364 = CIRCLE ( 'NONE', #32489, 0.1000000000000000194 ) ;
#40365 = EDGE_CURVE ( 'NONE', #38006, #26267, #14623, .T. ) ;
#40366 = CARTESIAN_POINT ( 'NONE',  ( 0.5530797604979859061, -1.185210387710321944, 0.6074893116751658440 ) ) ;
#40368 = ORIENTED_EDGE ( 'NONE', *, *, #17783, .T. ) ;
#40367 = ORIENTED_EDGE ( 'NONE', *, *, #22268, .F. ) ;
#40369 = CARTESIAN_POINT ( 'NONE',  ( 0.1653577314264058906, -1.273224196838065314, -0.7336113246882153271 ) ) ;
#40370 = AXIS2_PLACEMENT_3D ( 'NONE', #6085, #28125, #18655 ) ;
#40371 = AXIS2_PLACEMENT_3D ( 'NONE', #36974, #5706, #31230 ) ;
#40372 = CARTESIAN_POINT ( 'NONE',  ( 0.3408647536708550585, -1.672462434926486941, -0.5723210365178634795 ) ) ;
#40373 = AXIS2_PLACEMENT_3D ( 'NONE', #15465, #21847, #3115 ) ;
#40374 = DIRECTION ( 'NONE',  ( -1.000000000000000000, -2.341930812374887555E-31, 1.664003471950578127E-31 ) ) ;
#40375 = APPROVAL_ROLE ( '' ) ;
#40376 = DIRECTION ( 'NONE',  ( -1.540743955509787314E-32, 0.8709776783778059306, -0.4913225862583634473 ) ) ;
#40377 = VERTEX_POINT ( 'NONE', #21725 ) ;
#40378 = CARTESIAN_POINT ( 'NONE',  ( 0.09783940332773917448, -0.7228957342152418919, 0.3200629931280229434 ) ) ;
#40379 = AXIS2_PLACEMENT_3D ( 'NONE', #23915, #8257, #21020 ) ;
#40380 = B_SPLINE_CURVE_WITH_KNOTS ( 'NONE', 3,
 ( #2365, #33832, #18188, #6244 ),
 .UNSPECIFIED., .F., .F.,
 ( 4, 4 ),
 ( 2.016909803241189850E-16, 0.0003300623014047657277 ),
 .UNSPECIFIED. ) ;
#40381 = CARTESIAN_POINT ( 'NONE',  ( 0.1757500541653520265, -1.230771478115229245, -0.5931747813493342125 ) ) ;
#40382 = CARTESIAN_POINT ( 'NONE',  ( 0.1397249117745774649, -0.7016623770517458336, 0.5057382675813436590 ) ) ;
#40384 = CARTESIAN_POINT ( 'NONE',  ( 0.02999999999997886302, -2.183180860297921466, -0.4937760292030871079 ) ) ;
#40383 = FACE_OUTER_BOUND ( 'NONE', #18066, .T. ) ;
#40385 = ADVANCED_FACE ( 'NONE', ( #30586, #21944, #2409 ), #24415, .F. ) ;
#40386 = CARTESIAN_POINT ( 'NONE',  ( 0.05670245286071558255, -1.312040770489931729, 0.6142165760128855956 ) ) ;
#40387 = VERTEX_POINT ( 'NONE', #7081 ) ;
#40388 = CARTESIAN_POINT ( 'NONE',  ( 0.4611826087952243247, -1.678346039424960523, 0.5931467301849101537 ) ) ;
#40389 = CARTESIAN_POINT ( 'NONE',  ( 0.4821892592075923134, -1.087465116796244802, 0.8049660430408165368 ) ) ;
#40390 = DIRECTION ( 'NONE',  ( 0.000000000000000000, 0.5877852522924367218, -0.8090169943749738746 ) ) ;
#40391 = CARTESIAN_POINT ( 'NONE',  ( 0.02953079040095690777, -0.4684706630666085614, 0.2484463060367459175 ) ) ;
#40392 = DIRECTION ( 'NONE',  ( 0.4999551463232372317, -0.8660512985181134660, 0.000000000000000000 ) ) ;
#40393 = VECTOR ( 'NONE', #11936, 39.37007874015748854 ) ;
#40394 = CARTESIAN_POINT ( 'NONE',  ( 0.3826622209723776757, -1.758353618053019041, -0.4465348687276735062 ) ) ;
#40395 = VECTOR ( 'NONE', #5623, 39.37007874015748143 ) ;
#40396 = CARTESIAN_POINT ( 'NONE',  ( 0.09587768265485864527, -1.362549125761861823, -0.6668472307072548233 ) ) ;
#40397 = CARTESIAN_POINT ( 'NONE',  ( 0.3088330115105235030, -1.189194436044654912, 0.5067259279166422825 ) ) ;
#40398 = CARTESIAN_POINT ( 'NONE',  ( 0.4714567382560805875, -1.076664716445512093, 0.6912835816774075548 ) ) ;
#40399 = AXIS2_PLACEMENT_3D ( 'NONE', #35909, #26669, #7718 ) ;
#40400 = APPROVAL_ROLE ( '' ) ;
#40401 = DIRECTION ( 'NONE',  ( 1.000000000000000000, 0.000000000000000000, 0.000000000000000000 ) ) ;
#40402 = APPROVAL_PERSON_ORGANIZATION ( #1223, #22763, #4463 ) ;
#40403 = CARTESIAN_POINT ( 'NONE',  ( 0.3697988629570628794, -1.737277537897635948, -0.6804030624709919151 ) ) ;
#40404 = TOROIDAL_SURFACE ( 'NONE', #6890, 0.05330708661417342398, 0.01000000000000000021 ) ;
#40405 = CARTESIAN_POINT ( 'NONE',  ( -0.03171893264489181880, -0.3665010048041572599, -0.3753642664050083066 ) ) ;
#40406 = EDGE_CURVE ( 'NONE', #31712, #1392, #379, .T. ) ;
#40407 = EDGE_LOOP ( 'NONE', ( #7772, #34309, #642, #690, #3103, #18102 ) ) ;
#40408 = CARTESIAN_POINT ( 'NONE',  ( 0.4121964764379724144, -1.591045810388358905, -0.3442890830420804460 ) ) ;
#40409 = CARTESIAN_POINT ( 'NONE',  ( 0.1999999999999789724, -2.183180860297921466, -0.4937760292030871079 ) ) ;
#40410 = EDGE_CURVE ( 'NONE', #4670, #28266, #7384, .T. ) ;
#40411 = CARTESIAN_POINT ( 'NONE',  ( 0.08978320868449755909, -0.5653313875429684110, 0.1301661300597059812 ) ) ;
#40412 = ORIENTED_EDGE ( 'NONE', *, *, #7708, .T. ) ;
#40413 = CARTESIAN_POINT ( 'NONE',  ( -0.03171893264488560849, -0.07587196131163935486, -0.5190999561769865656 ) ) ;
#40414 = CARTESIAN_POINT ( 'NONE',  ( -0.01435986368806844819, -0.8524412751134723409, 0.2543499331468145330 ) ) ;
#40416 = ORIENTED_EDGE ( 'NONE', *, *, #21376, .F. ) ;
#40415 = EDGE_LOOP ( 'NONE', ( #6519, #31330, #31440, #7413, #33992, #27767, #3649, #4944, #29508, #28587, #37141, #38053, #17742 ) ) ;
#40417 = CARTESIAN_POINT ( 'NONE',  ( -1.502516396515344672E-15, -0.3899999999999999578, 5.463695987328526437E-16 ) ) ;
#40418 = CARTESIAN_POINT ( 'NONE',  ( 0.02872242845529804703, -0.07817994906157445245, 0.5268390348591310834 ) ) ;
#40419 = FACE_OUTER_BOUND ( 'NONE', #34925, .T. ) ;
#40420 = CARTESIAN_POINT ( 'NONE',  ( 0.3663367775733478715, -2.020566543745489607, -0.4857000487067979488 ) ) ;
#40421 = DIRECTION ( 'NONE',  ( 4.930380657631323784E-32, 0.7472307839325098566, 0.6645646360916346307 ) ) ;
#40423 = CARTESIAN_POINT ( 'NONE',  ( 0.1757500541653520265, -1.230771478115229245, -0.7462941026102624109 ) ) ;
#40422 = CARTESIAN_POINT ( 'NONE',  ( 0.03170752374382720951, 0.4816921673044493035, 0.09938322573836459728 ) ) ;
#40424 = CARTESIAN_POINT ( 'NONE',  ( -0.3000000000000000999, -2.853330612949663170, -0.7088139570729240502 ) ) ;
#40425 = B_SPLINE_CURVE_WITH_KNOTS ( 'NONE', 3,
 ( #11330, #33525, #26966, #7824, #39115, #20606, #20395, #33334, #20816, #39499, #8632, #5143, #8439, #39309, #14830, #36428, #32923, #4733 ),
 .UNSPECIFIED., .F., .F.,
 ( 4, 2, 2, 2, 2, 2, 2, 2, 4 ),
 ( -0.002633528389679640983, -0.001975271857855670846, -0.001317015326031701142, -0.0006587587942077310042, -5.022623837613003628E-07, 0.0006577542694402084035, 0.001316010801264178975, 0.001974267333088148679, 0.002632523864912118382 ),
 .UNSPECIFIED. ) ;
#40426 = EDGE_LOOP ( 'NONE', ( #11646, #32643, #10567, #25556 ) ) ;
#40427 = AXIS2_PLACEMENT_3D ( 'NONE', #26104, #19515, #16829 ) ;
#40428 = CARTESIAN_POINT ( 'NONE',  ( 0.08031759231403769184, -1.309115413162167396, 0.5634110904151367061 ) ) ;
#40429 = ORIENTED_EDGE ( 'NONE', *, *, #32958, .F. ) ;
#40430 = FACE_OUTER_BOUND ( 'NONE', #19063, .T. ) ;
#40431 = CARTESIAN_POINT ( 'NONE',  ( 0.09166549204113492999, -0.6531214586304496805, 0.4451350988387396401 ) ) ;
#40432 = EDGE_CURVE ( 'NONE', #34649, #24445, #22551, .T. ) ;
#40434 = CARTESIAN_POINT ( 'NONE',  ( 0.5534895568977906688, -1.623564024766104508, 0.5247869855815567863 ) ) ;
#40433 = CARTESIAN_POINT ( 'NONE',  ( 0.1876095839365585771, -1.270310460104812744, 0.4282417262808775882 ) ) ;
#40435 = CARTESIAN_POINT ( 'NONE',  ( 0.01548846960707306146, 0.2306506793133153710, 0.4716198300880833916 ) ) ;
#40436 = DIRECTION ( 'NONE',  ( 0.4999551463232373427, -0.8660512985181134660, 0.000000000000000000 ) ) ;
#40437 = LOCAL_TIME ( 0, 53, 7.000000000000000000, #36050 ) ;
#40438 = ADVANCED_FACE ( 'NONE', ( #16560 ), #15954, .T. ) ;
#40439 = UNCERTAINTY_MEASURE_WITH_UNIT (LENGTH_MEASURE( 1.000000000000000082E-05 ), #16884, 'distance_accuracy_value', 'NONE');
#40440 = LINE ( 'NONE', #24821, #12112 ) ;
#40441 = ADVANCED_FACE ( 'NONE', ( #3401 ), #579, .T. ) ;
#40442 = CARTESIAN_POINT ( 'NONE',  ( 0.3887841298280355073, -1.916107351281247873, -0.3024084733865095020 ) ) ;
#40443 = CARTESIAN_POINT ( 'NONE',  ( 0.5736464802932748075, -1.499188840390029975, 0.5681326666576531625 ) ) ;
#40444 = CIRCLE ( 'NONE', #32534, 0.1600000000000006417 ) ;
#40445 = CARTESIAN_POINT ( 'NONE',  ( 0.4776203807509608046, -1.679318457215359883, 0.5575138488100176426 ) ) ;
#40446 = CARTESIAN_POINT ( 'NONE',  ( -0.2267371898560520682, -0.4872893062166330780, 0.3749999999999990008 ) ) ;
#40447 = CARTESIAN_POINT ( 'NONE',  ( -0.01895884884825297517, 0.4667865995382938227, 0.2292744456225711547 ) ) ;
#40448 = CARTESIAN_POINT ( 'NONE',  ( -0.02000000000000000042, -2.032088213807425880, -0.4352898549974345555 ) ) ;
#40449 = CARTESIAN_POINT ( 'NONE',  ( 0.000000000000000000, 0.000000000000000000, 0.000000000000000000 ) ) ;
#40450 = CARTESIAN_POINT ( 'NONE',  ( 0.1840567930975518796, -0.8547793429265486687, 0.1477568935609660794 ) ) ;
#40451 = CARTESIAN_POINT ( 'NONE',  ( 0.3560095073596968307, -0.8726986411092064744, 0.7484988241699506162 ) ) ;
#40452 = CARTESIAN_POINT ( 'NONE',  ( -0.02953079040095600918, 0.2329676531120531691, 0.4763574306556323523 ) ) ;
#40453 = CARTESIAN_POINT ( 'NONE',  ( -0.1710642718812883378, 0.4986889572247745761, 0.3079501053856181780 ) ) ;
#40454 = VECTOR ( 'NONE', #21707, 39.37007874015748143 ) ;
#40455 = CARTESIAN_POINT ( 'NONE',  ( 0.6002617396867515609, -1.576047946042514525, -0.4213240105477804587 ) ) ;
#40456 = AXIS2_PLACEMENT_3D ( 'NONE', #15960, #6888, #4000 ) ;
#40457 = CARTESIAN_POINT ( 'NONE',  ( 0.1959265899308195724, -1.288818386415671036, -0.7414046965098800568 ) ) ;
#40458 = FACE_OUTER_BOUND ( 'NONE', #23194, .T. ) ;
#40459 = CARTESIAN_POINT ( 'NONE',  ( 0.3993723638686003108, -1.146829347344676453, 0.4244434305191919776 ) ) ;
#40460 = LINE ( 'NONE', #24426, #31098 ) ;
#40461 = APPLIED_APPROVAL_ASSIGNMENT ( #28494, ( #22077 ) ) ;
#40462 = ORIENTED_EDGE ( 'NONE', *, *, #27502, .F. ) ;
#40463 = CARTESIAN_POINT ( 'NONE',  ( -0.3000000000000000999, -1.835749455202394298, -0.3938319975228649072 ) ) ;
#40464 = LINE ( 'NONE', #18443, #8158 ) ;
#40465 = CARTESIAN_POINT ( 'NONE',  ( 0.6589248908660086945, -1.495897505468516853, 0.4182417262808776903 ) ) ;
#40466 = EDGE_CURVE ( 'NONE', #32724, #32720, #38356, .T. ) ;
#40467 = CARTESIAN_POINT ( 'NONE',  ( 0.4108473310524629052, -1.676356312003210780, -0.6312918840655212804 ) ) ;
#40468 = ADVANCED_FACE ( 'NONE', ( #35286 ), #36969, .F. ) ;
#40469 = CIRCLE ( 'NONE', #28001, 0.03000000000000029379 ) ;
#40470 = ORIENTED_EDGE ( 'NONE', *, *, #20282, .T. ) ;
#40471 = CARTESIAN_POINT ( 'NONE',  ( 0.5068534190187480304, -1.686660372286016729, -0.6047723693427432545 ) ) ;
#40472 = DIRECTION ( 'NONE',  ( 0.000000000000000000, 0.000000000000000000, 1.000000000000000000 ) ) ;
#40473 = CARTESIAN_POINT ( 'NONE',  ( 0.3327923242355236289, -1.761774052064265295, 0.4761320618463714127 ) ) ;
#40474 = CARTESIAN_POINT ( 'NONE',  ( 0.05201782277453608633, 0.2909620873304535893, -0.3697179445082223181 ) ) ;
#40475 = CARTESIAN_POINT ( 'NONE',  ( 0.5035873862616617735, -1.298196369232728076, 0.6491550123535173578 ) ) ;
#40477 = FACE_OUTER_BOUND ( 'NONE', #1878, .T. ) ;
#40476 = CARTESIAN_POINT ( 'NONE',  ( -0.1679467284717053865, 0.5217198260999535986, 0.1377606880063677042 ) ) ;
#40478 = CARTESIAN_POINT ( 'NONE',  ( 0.2117717001728993131, -0.8880493388543053701, 0.3804667941236127282 ) ) ;
#40479 = ORIENTED_EDGE ( 'NONE', *, *, #6421, .F. ) ;
#40480 = SECURITY_CLASSIFICATION_LEVEL ( 'unclassified' ) ;
#40481 = CARTESIAN_POINT ( 'NONE',  ( 0.1041180756838251814, -1.398163384010766785, 0.6248096187470618679 ) ) ;
#40482 = ORIENTED_EDGE ( 'NONE', *, *, #32260, .F. ) ;
#40483 = ORIENTED_EDGE ( 'NONE', *, *, #18810, .T. ) ;
#40484 = CARTESIAN_POINT ( 'NONE',  ( 0.04822329218285972136, -0.5481102735168966733, 0.2156808200189340163 ) ) ;
#40486 = CARTESIAN_POINT ( 'NONE',  ( 0.1121164433129688554, -0.8360957577110439409, -0.04471693353407518723 ) ) ;
#40485 = DIRECTION ( 'NONE',  ( -0.4999551463232377313, 0.8660512985181132439, -0.000000000000000000 ) ) ;
#40487 = PLANE ( 'NONE',  #2412 ) ;
#40488 = VERTEX_POINT ( 'NONE', #35081 ) ;
#40489 = ORIENTED_EDGE ( 'NONE', *, *, #16187, .T. ) ;
#40490 = AXIS2_PLACEMENT_3D ( 'NONE', #34304, #6111, #18678 ) ;
#40491 = CARTESIAN_POINT ( 'NONE',  ( 0.3927997951677614785, -1.109372561784171873, 0.6250621135928259298 ) ) ;
#40492 = CARTESIAN_POINT ( 'NONE',  ( 0.5532976880032102196, -1.511228520888749927, 0.5786546175993648733 ) ) ;
#40493 = ORIENTED_EDGE ( 'NONE', *, *, #16701, .F. ) ;
#40494 = CARTESIAN_POINT ( 'NONE',  ( 0.02953079040095687308, 0.09152108205202039160, -0.5223162075576429642 ) ) ;
#40495 = DIRECTION ( 'NONE',  ( -0.4261641068392704734, 0.000000000000000000, -0.9046458721742374198 ) ) ;
#40496 = APPLIED_SECURITY_CLASSIFICATION_ASSIGNMENT ( #6983, ( #40651 ) ) ;
#40497 = CARTESIAN_POINT ( 'NONE',  ( 0.5616069494768038961, -1.585551047948461578, -0.5092418914868334090 ) ) ;
#40498 = LINE ( 'NONE', #11899, #35799 ) ;
#40499 = AXIS2_PLACEMENT_3D ( 'NONE', #10808, #20275, #14477 ) ;
#40500 = CARTESIAN_POINT ( 'NONE',  ( 0.3538719729184750529, -1.624715450675502826, 0.4182417262808776903 ) ) ;
#40501 = CARTESIAN_POINT ( 'NONE',  ( 0.4790130493689879199, -1.660633143797948241, 0.5197417262808792238 ) ) ;
#40502 = DIRECTION ( 'NONE',  ( 0.8724162812079789830, -0.4887635750372981702, 0.000000000000000000 ) ) ;
#40503 = CARTESIAN_POINT ( 'NONE',  ( 0.1865135932075447367, -1.586003729253250283, -0.6557087401434340546 ) ) ;
#40504 = CARTESIAN_POINT ( 'NONE',  ( 0.07539036843641495900, -1.329185100875404313, 0.6514330093269139477 ) ) ;
#40505 = PERSON_AND_ORGANIZATION_ROLE ( 'creator' ) ;
#40506 = B_SPLINE_CURVE_WITH_KNOTS ( 'NONE', 3,
 ( #12300, #24858, #11874, #15166, #6099, #40260, #31009, #31424, #12093, #24659, #34092, #9191, #5895, #3227 ),
 .UNSPECIFIED., .F., .F.,
 ( 4, 2, 2, 2, 2, 2, 4 ),
 ( 4.300435128097903527E-16, 0.001060840485211818384, 0.001591260727817513879, 0.002121680970423209592, 0.002652101213028904871, 0.003182521455634601017, 0.004243361940845996778 ),
 .UNSPECIFIED. ) ;
#40507 = CARTESIAN_POINT ( 'NONE',  ( 0.2098534808732534784, -0.9273921219866952947, 0.3620977009047463002 ) ) ;
#40508 = CARTESIAN_POINT ( 'NONE',  ( 0.4726093400148664303, -1.113121474480951889, 0.5480980819454659425 ) ) ;
#40509 = CARTESIAN_POINT ( 'NONE',  ( 0.5594238137014129197, -1.182849275086621521, 0.6057417262809816627 ) ) ;
#40510 = DIRECTION ( 'NONE',  ( 8.628166150854818811E-32, -0.1402348365093016580, -0.9901182710308954471 ) ) ;
#40511 = CARTESIAN_POINT ( 'NONE',  ( 0.004566372195762857279, -0.8656213538948328567, 0.4622093217984943880 ) ) ;
#40512 = CARTESIAN_POINT ( 'NONE',  ( -0.1999999999999998446, 0.5182417262804734914, 0.3749999999999999445 ) ) ;
#40513 = CARTESIAN_POINT ( 'NONE',  ( 0.6928668329258086400, -1.429029060959297937, 0.5420566053040769550 ) ) ;
#40514 = AXIS2_PLACEMENT_3D ( 'NONE', #14863, #27424, #7671 ) ;
#40515 = CARTESIAN_POINT ( 'NONE',  ( -0.2399999999999999079, -2.853330612949663170, -0.7688139570729241035 ) ) ;
#40516 = VERTEX_POINT ( 'NONE', #25215 ) ;
#40517 = ORIENTED_EDGE ( 'NONE', *, *, #20567, .T. ) ;
#40518 = CARTESIAN_POINT ( 'NONE',  ( -0.1142670043590602175, -0.4723146173917087687, 0.1178658435937002397 ) ) ;
#40519 = ORIENTED_EDGE ( 'NONE', *, *, #27792, .T. ) ;
#40520 = APPLIED_SECURITY_CLASSIFICATION_ASSIGNMENT ( #31348, ( #40660 ) ) ;
#40521 = DIRECTION ( 'NONE',  ( -4.930380657631323784E-32, -0.7472307839325098566, -0.6645646360916346307 ) ) ;
#40522 = CARTESIAN_POINT ( 'NONE',  ( -0.03654364704248874718, -0.5058694728073482860, -0.07650507870001360677 ) ) ;
#40523 = CARTESIAN_POINT ( 'NONE',  ( 0.5969700620808515712, -1.458905189709731154, 0.6310679806792612867 ) ) ;
#40525 = ORIENTED_EDGE ( 'NONE', *, *, #8751, .T. ) ;
#40524 = CARTESIAN_POINT ( 'NONE',  ( 0.6054889487767985967, -1.479703267939684874, 0.5856070495615782745 ) ) ;
#40526 = AXIS2_PLACEMENT_3D ( 'NONE', #4844, #32430, #13904 ) ;
#40527 = ORIENTED_EDGE ( 'NONE', *, *, #39190, .F. ) ;
#40528 = CARTESIAN_POINT ( 'NONE',  ( -0.02000000000000000042, -1.599201040860868339, 0.1642182323853691728 ) ) ;
#40529 = ORIENTED_EDGE ( 'NONE', *, *, #26141, .F. ) ;
#40530 = CARTESIAN_POINT ( 'NONE',  ( 0.1847070558194194301, -1.276978442851412154, 0.9301116397864819252 ) ) ;
#40532 = CARTESIAN_POINT ( 'NONE',  ( -0.01548846960721252282, -0.4730347584884301293, 0.2341461249027971259 ) ) ;
#40531 = CARTESIAN_POINT ( 'NONE',  ( 0.3416240168993061044, -1.109164787499526961, 0.7393468023686904367 ) ) ;
#40533 = CARTESIAN_POINT ( 'NONE',  ( 0.3663975874019590462, -1.157438136726378408, 0.4269148889825721827 ) ) ;
#40534 = CARTESIAN_POINT ( 'NONE',  ( 0.1909286924077255032, -1.257064795538239022, -0.2869361388274795921 ) ) ;
#40536 = VERTEX_POINT ( 'NONE', #29107 ) ;
#40535 = ORIENTED_EDGE ( 'NONE', *, *, #27885, .T. ) ;
#40537 = CARTESIAN_POINT ( 'NONE',  ( 0.4469283285619457535, -1.099869350908817101, -0.4033480720695141741 ) ) ;
#40538 = CARTESIAN_POINT ( 'NONE',  ( 0.4121862343158209652, -1.741309959742503244, -0.4470289626379757575 ) ) ;
#40539 = CARTESIAN_POINT ( 'NONE',  ( -0.03874953289575334275, -0.4622846869243766310, 0.1151793484519262750 ) ) ;
#40540 = CARTESIAN_POINT ( 'NONE',  ( 0.2098138332575895104, -0.8876503706691467599, 0.7004616250147996936 ) ) ;
#40541 = CARTESIAN_POINT ( 'NONE',  ( 0.1383678021865805130, -0.8347292794016092365, 0.3450883820417707804 ) ) ;
#40542 = DIRECTION ( 'NONE',  ( -1.000000000000000000, -0.000000000000000000, -0.000000000000000000 ) ) ;
#40543 = CARTESIAN_POINT ( 'NONE',  ( -0.1157923916715208196, -0.5295015842444287246, 0.3181161673586317962 ) ) ;
#40544 = VECTOR ( 'NONE', #19381, 39.37007874015748143 ) ;
#40545 = APPLICATION_CONTEXT ( 'configuration controlled 3d designs of mechanical parts and assemblies' ) ;
#40546 = CARTESIAN_POINT ( 'NONE',  ( 0.4168539117269804417, -1.242125193379584935, 0.5412798315864792986 ) ) ;
#40547 = DIRECTION ( 'NONE',  ( -0.8660254037844404840, -0.3535533905932716769, 0.3535533905932716769 ) ) ;
#40548 = CARTESIAN_POINT ( 'NONE',  ( 0.3476487115878558187, -1.071941005786004819, 0.7622982368131399067 ) ) ;
#40549 = DIRECTION ( 'NONE',  ( 0.000000000000000000, -0.2513338844154403007, 0.9679004486746795033 ) ) ;
#40550 = EDGE_CURVE ( 'NONE', #22378, #6266, #26471, .T. ) ;
#40551 = CARTESIAN_POINT ( 'NONE',  ( 0.02953079040095489896, -0.2329676531120505323, 0.4763574306556353499 ) ) ;
#40552 = CARTESIAN_POINT ( 'NONE',  ( 0.03506116283237684095, -0.6633195576212149724, 0.6677130251333698308 ) ) ;
#40553 = CARTESIAN_POINT ( 'NONE',  ( 0.05525033686093953900, -1.048202366712872147, 0.7271762683524501947 ) ) ;
#40554 = DATE_AND_TIME ( #9275, #15481 ) ;
#40555 = CARTESIAN_POINT ( 'NONE',  ( 0.6859459673519229250, -1.411154268469613227, 0.7682993476293730195 ) ) ;
#40556 = CARTESIAN_POINT ( 'NONE',  ( 0.3222894045021684195, -1.758215778056678724, 0.5682417262808792113 ) ) ;
#40557 = FACE_OUTER_BOUND ( 'NONE', #12204, .T. ) ;
#40558 = CARTESIAN_POINT ( 'NONE',  ( 0.05562144613422614903, -0.2870684680408724931, 0.3605846877396505223 ) ) ;
#40559 = EDGE_CURVE ( 'NONE', #38965, #36975, #35033, .T. ) ;
#40560 = DIRECTION ( 'NONE',  ( 0.000000000000000000, 0.7071067811865474617, 0.7071067811865475727 ) ) ;
#40561 = EDGE_LOOP ( 'NONE', ( #11816, #15936, #10559, #10509 ) ) ;
#40562 = CARTESIAN_POINT ( 'NONE',  ( -0.1731185243557763487, 0.5373335498847187086, 0.3749999999999995559 ) ) ;
#40563 = PRODUCT_DEFINITION ( 'UNKNOWN', '', #39117, #29430 ) ;
#40564 = CARTESIAN_POINT ( 'NONE',  ( 0.2128671618955360612, -1.417862351214104200, 0.9322687174078309047 ) ) ;
#40565 = CARTESIAN_POINT ( 'NONE',  ( 0.4825082729884774269, -1.333409512969114141, 0.8153832532642322217 ) ) ;
#40567 = ORIENTED_EDGE ( 'NONE', *, *, #13486, .T. ) ;
#40566 = PLANE ( 'NONE',  #28976 ) ;
#40568 = CARTESIAN_POINT ( 'NONE',  ( 0.2495280903959155583, -0.7823963870098056272, 0.5160991521645093005 ) ) ;
#40570 = ORIENTED_EDGE ( 'NONE', *, *, #10752, .F. ) ;
#40569 = ORIENTED_EDGE ( 'NONE', *, *, #15503, .T. ) ;
#40571 = DIRECTION ( 'NONE',  ( 0.4999551463232372317, -0.8660512985181134660, -6.869252350113302335E-17 ) ) ;
#40572 = CARTESIAN_POINT ( 'NONE',  ( -2.112273405726188513E-14, -2.183180860297921466, -0.4937760292030871079 ) ) ;
#40573 = FACE_OUTER_BOUND ( 'NONE', #21354, .T. ) ;
#40574 = DATE_TIME_ROLE ( 'classification_date' ) ;
#40575 = DIRECTION ( 'NONE',  ( 0.5000000000000003331, 6.162975822039154730E-31, 0.8660254037844383745 ) ) ;
#40576 = ORIENTED_EDGE ( 'NONE', *, *, #9989, .T. ) ;
#40577 = CARTESIAN_POINT ( 'NONE',  ( 0.1281083501185726337, -0.8152981500214998567, 0.4630848436273822810 ) ) ;
#40578 = AXIS2_PLACEMENT_3D ( 'NONE', #7415, #39116, #140 ) ;
#40579 = CARTESIAN_POINT ( 'NONE',  ( 0.3164777849907467466, -1.747345822248904668, 0.7454006856945649684 ) ) ;
#40580 = CARTESIAN_POINT ( 'NONE',  ( 0.5043263792969816528, -1.486040407161054233, 0.7488984814174186599 ) ) ;
#40581 = CARTESIAN_POINT ( 'NONE',  ( -0.1999999999999997891, 0.5182417262804744906, 0.3749999999999995559 ) ) ;
#40582 = CARTESIAN_POINT ( 'NONE',  ( -0.1684323895664760207, 0.5231977504175434612, 0.1528658435937284565 ) ) ;
#40583 = ORIENTED_EDGE ( 'NONE', *, *, #12396, .F. ) ;
#40584 = CARTESIAN_POINT ( 'NONE',  ( 0.4439201956396305326, -1.688295707146957758, 0.5959241158817605299 ) ) ;
#40585 = CARTESIAN_POINT ( 'NONE',  ( 0.7052107660210322759, -1.443684245437774294, 0.7850599799250342903 ) ) ;
#40586 = EDGE_CURVE ( 'NONE', #15711, #31816, #10085, .T. ) ;
#40587 = DIRECTION ( 'NONE',  ( -1.000000000000000000, -0.000000000000000000, -0.000000000000000000 ) ) ;
#40588 = ADVANCED_FACE ( 'NONE', ( #25625 ), #10724, .F. ) ;
#40589 = CARTESIAN_POINT ( 'NONE',  ( 0.05283710938261019369, -0.4560492058803811144, 0.1064717188025609967 ) ) ;
#40590 = LINE ( 'NONE', #12219, #22578 ) ;
#40591 = ADVANCED_FACE ( 'NONE', ( #15744 ), #20189, .T. ) ;
#40592 = CARTESIAN_POINT ( 'NONE',  ( 0.3853411735687863326, -1.756807109041631509, -0.4499573014711771846 ) ) ;
#40593 = EDGE_CURVE ( 'NONE', #28482, #16052, #26848, .T. ) ;
#40594 = CARTESIAN_POINT ( 'NONE',  ( -0.3000000000000000999, -3.985676108854518507, -0.7623095129438225426 ) ) ;
#40595 = EDGE_CURVE ( 'NONE', #12691, #12319, #35895, .T. ) ;
#40596 = DIRECTION ( 'NONE',  ( 0.000000000000000000, -7.757484229545264892E-16, -1.000000000000000000 ) ) ;
#40597 = CARTESIAN_POINT ( 'NONE',  ( 0.4100600194349330319, -1.011029760475403494, 0.6817144834752139060 ) ) ;
#40598 = APPROVAL_ROLE ( '' ) ;
#40599 =( BOUNDED_SURFACE ( )  B_SPLINE_SURFACE ( 3, 2, ( 
 ( #26485, #2206, #33257 ),
 ( #35736, #36551, #17219 ),
 ( #4855, #39022, #17427 ),
 ( #5067, #20730, #23429 ),
 ( #27092, #29982, #8362 ),
 ( #32839, #27311, #5259 ) ),
 .UNSPECIFIED., .F., .F., .T. ) 
 B_SPLINE_SURFACE_WITH_KNOTS ( ( 4, 2, 4 ),
 ( 3, 3 ),
 ( 3.385963384672230347E-16, 0.0006229787267328064718, 0.001245957453465274239 ),
 ( 0.000000000000000000, 1.000000000000000000 ),
 .UNSPECIFIED. ) 
 GEOMETRIC_REPRESENTATION_ITEM ( )  RATIONAL_B_SPLINE_SURFACE ( (
 ( 1.000000000000000000, 0.9231872052445554422, 1.000000000000000000),
 ( 1.000000000000000000, 0.9271591560550311861, 1.000000000000000000),
 ( 1.000000000000000000, 0.9286221054271613928, 1.000000000000000000),
 ( 1.000000000000000000, 0.9259746644423475503, 1.000000000000000000),
 ( 1.000000000000000000, 0.9219504995353200449, 1.000000000000000000),
 ( 1.000000000000000000, 0.9159177456829653563, 1.000000000000000000) ) ) 
 REPRESENTATION_ITEM ( '' )  SURFACE ( )  );
#40600 = CARTESIAN_POINT ( 'NONE',  ( 0.3578407435306584228, -1.776530764634635551, -0.5202682414489888663 ) ) ;
#40601 = ORIENTED_EDGE ( 'NONE', *, *, #5765, .T. ) ;
#40602 = CARTESIAN_POINT ( 'NONE',  ( 0.3959951078739687436, -1.707197240620605738, 0.4182417262808776903 ) ) ;
#40603 = AXIS2_PLACEMENT_3D ( 'NONE', #36937, #28283, #9572 ) ;
#40604 = CARTESIAN_POINT ( 'NONE',  ( -0.04285534776242042043, -0.07199417564834888206, 0.4895512033229395543 ) ) ;
#40605 = EDGE_CURVE ( 'NONE', #10331, #4952, #19279, .T. ) ;
#40606 = VERTEX_POINT ( 'NONE', #20269 ) ;
#40607 = CARTESIAN_POINT ( 'NONE',  ( -0.1212602504878817211, -0.5073146173917503221, 0.3048175120576748220 ) ) ;
#40608 = LINE ( 'NONE', #27872, #18398 ) ;
#40609 = LINE ( 'NONE', #21301, #3546 ) ;
#40610 = VERTEX_POINT ( 'NONE', #14471 ) ;
#40611 = CARTESIAN_POINT ( 'NONE',  ( -0.05281452789367557105, -0.03978571835446843147, -0.4666805157975096874 ) ) ;
#40612 = CARTESIAN_POINT ( 'NONE',  ( 0.1363060833980020425, -1.291389234375735384, 0.7246493219598814095 ) ) ;
#40614 = VERTEX_POINT ( 'NONE', #1351 ) ;
#40613 = ORIENTED_EDGE ( 'NONE', *, *, #3635, .F. ) ;
#40615 = CARTESIAN_POINT ( 'NONE',  ( -0.01548846960707545191, -0.5346638663566677385, -0.07572681171513533094 ) ) ;
#40616 = CARTESIAN_POINT ( 'NONE',  ( -0.02000000000000000042, -2.379949255320110257, -0.6346823614705312533 ) ) ;
#40617 = CARTESIAN_POINT ( 'NONE',  ( 0.1844765520120722202, -1.888974760190525570, -0.3406829697689818248 ) ) ;
#40618 = CARTESIAN_POINT ( 'NONE',  ( 0.3539619486986738672, -1.095399617261031411, 0.7051293634830863022 ) ) ;
#40620 = CARTESIAN_POINT ( 'NONE',  ( 0.01220508677664999299, -0.4284039737085656996, 0.1457185332388702959 ) ) ;
#40619 = CARTESIAN_POINT ( 'NONE',  ( -0.07216878364870250862, 0.05141091571461216952, 0.1249999999999993477 ) ) ;
#40621 = CARTESIAN_POINT ( 'NONE',  ( 0.05561375719525302880, -0.2871676730027881153, -0.3605331597494366713 ) ) ;
#40622 = ORIENTED_EDGE ( 'NONE', *, *, #27283, .F. ) ;
#40623 = CARTESIAN_POINT ( 'NONE',  ( 0.08996436532983868861, -0.5633779834408316756, 0.1624145888708820040 ) ) ;
#40624 = ORIENTED_EDGE ( 'NONE', *, *, #12408, .T. ) ;
#40625 = ORIENTED_EDGE ( 'NONE', *, *, #36892, .F. ) ;
#40626 = DIRECTION ( 'NONE',  ( 0.8724162812079758744, -0.4887635750373036103, 0.000000000000000000 ) ) ;
#40627 = CARTESIAN_POINT ( 'NONE',  ( 0.4415431555067652059, -1.573721655358518268, 0.5715020639883481302 ) ) ;
#40629 = LINE ( 'NONE', #28491, #18270 ) ;
#40628 = CARTESIAN_POINT ( 'NONE',  ( -0.05082303569918699554, -0.4631054925596483351, 0.09932635337952169796 ) ) ;
#40630 = CARTESIAN_POINT ( 'NONE',  ( -0.02000000000000000042, -2.314906514113384883, -0.5881050943081593818 ) ) ;
#40631 = CARTESIAN_POINT ( 'NONE',  ( -0.1684323895664670556, 0.5231977504175358007, 0.3749999999999990008 ) ) ;
#40632 = CARTESIAN_POINT ( 'NONE',  ( -0.01548846960712817709, -0.4730347584885852830, -0.2341461249029094249 ) ) ;
#40633 = CARTESIAN_POINT ( 'NONE',  ( 0.1885375905025258314, -1.930959840804365335, -0.3029267234423492772 ) ) ;
#40634 = CARTESIAN_POINT ( 'NONE',  ( 0.1253475045672584887, -0.5634446532171664135, 0.2188656290601465049 ) ) ;
#40635 = CARTESIAN_POINT ( 'NONE',  ( 0.4798443520715884869, -1.677655393100440318, 0.5509470553349121724 ) ) ;
#40636 = CARTESIAN_POINT ( 'NONE',  ( -0.01548846960707418556, 0.3688619771572939632, -0.3775276577326990290 ) ) ;
#40637 = EDGE_CURVE ( 'NONE', #40066, #13700, #18627, .T. ) ;
#40638 = DIRECTION ( 'NONE',  ( 0.9998941247116546194, -0.01455087607601020412, 0.0001066420868422379362 ) ) ;
#40639 = CARTESIAN_POINT ( 'NONE',  ( 0.2316897038216818305, -1.233203694889816404, 0.5465952261361649578 ) ) ;
#40640 = EDGE_CURVE ( 'NONE', #33728, #32971, #23374, .T. ) ;
#40641 = CARTESIAN_POINT ( 'NONE',  ( 0.2114942970145866630, -1.236211323811057694, 0.5631196975457352094 ) ) ;
#40642 = DIRECTION ( 'NONE',  ( -2.563099466555627715E-12, 0.000000000000000000, 1.000000000000000000 ) ) ;
#40643 = ADVANCED_FACE ( 'NONE', ( #6020 ), #37301, .T. ) ;
#40644 = CARTESIAN_POINT ( 'NONE',  ( 0.6775446752225827707, -1.407456786189307696, 0.5068639979343774193 ) ) ;
#40645 = CARTESIAN_POINT ( 'NONE',  ( -0.02242905165739062651, 0.3548958552285692569, 0.3695186750059857306 ) ) ;
#40646 = CARTESIAN_POINT ( 'NONE',  ( 0.02238204800581933274, -1.092291325666332469, 0.6350144242741103673 ) ) ;
#40647 = CARTESIAN_POINT ( 'NONE',  ( 0.05269111014006346017, 0.2828051265736298281, -0.3737594984297845646 ) ) ;
#40648 = NEXT_ASSEMBLY_USAGE_OCCURRENCE ( 'NAUO1', ' ', ' ', #7895, #38779, $ ) ;
#40649 = NEXT_ASSEMBLY_USAGE_OCCURRENCE ( 'NAUO2', ' ', ' ', #7895, #11907, $ ) ;
#40650 = NEXT_ASSEMBLY_USAGE_OCCURRENCE ( 'NAUO3', ' ', ' ', #7895, #8373, $ ) ;
#40651 = NEXT_ASSEMBLY_USAGE_OCCURRENCE ( 'NAUO4', ' ', ' ', #7895, #6386, $ ) ;
#40652 = NEXT_ASSEMBLY_USAGE_OCCURRENCE ( 'NAUO5', ' ', ' ', #7895, #35536, $ ) ;
#40653 = NEXT_ASSEMBLY_USAGE_OCCURRENCE ( 'NAUO6', ' ', ' ', #7895, #40563, $ ) ;
#40654 = NEXT_ASSEMBLY_USAGE_OCCURRENCE ( 'NAUO7', ' ', ' ', #7895, #37836, $ ) ;
#40655 = NEXT_ASSEMBLY_USAGE_OCCURRENCE ( 'NAUO8', ' ', ' ', #7895, #1177, $ ) ;
#40656 = NEXT_ASSEMBLY_USAGE_OCCURRENCE ( 'NAUO9', ' ', ' ', #7895, #1177, $ ) ;
#40657 = NEXT_ASSEMBLY_USAGE_OCCURRENCE ( 'NAUO10', ' ', ' ', #7895, #1177, $ ) ;
#40658 = NEXT_ASSEMBLY_USAGE_OCCURRENCE ( 'NAUO11', ' ', ' ', #7895, #1177, $ ) ;
#40659 = NEXT_ASSEMBLY_USAGE_OCCURRENCE ( 'NAUO12', ' ', ' ', #7895, #37836, $ ) ;
#40660 = NEXT_ASSEMBLY_USAGE_OCCURRENCE ( 'NAUO13', ' ', ' ', #7895, #20515, $ ) ;
#40661 = NEXT_ASSEMBLY_USAGE_OCCURRENCE ( 'NAUO14', ' ', ' ', #7895, #11166, $ ) ;
#40662 = NEXT_ASSEMBLY_USAGE_OCCURRENCE ( 'NAUO15', ' ', ' ', #37836, #2626, $ ) ;
#40663 = NEXT_ASSEMBLY_USAGE_OCCURRENCE ( 'NAUO16', ' ', ' ', #37836, #25768, $ ) ;
#40664 = NEXT_ASSEMBLY_USAGE_OCCURRENCE ( 'NAUO17', ' ', ' ', #37836, #17711, $ ) ;
#40665 = NEXT_ASSEMBLY_USAGE_OCCURRENCE ( 'NAUO18', ' ', ' ', #37836, #17711, $ ) ;
#40666 = NEXT_ASSEMBLY_USAGE_OCCURRENCE ( 'NAUO19', ' ', ' ', #37836, #11166, $ ) ;
#40667=COLOUR_RGB('Dark Blue',0.08,0.2,0.34);
#40668=FILL_AREA_STYLE_COLOUR('',#40667);
#40669=FILL_AREA_STYLE('',(#40668));
#40670=SURFACE_STYLE_FILL_AREA(#40669);
#40671=SURFACE_SIDE_STYLE('',(#40670));
#40672=SURFACE_STYLE_USAGE(.BOTH.,#40671);
#40673=PRESENTATION_STYLE_ASSIGNMENT((#40672));
#40674=COLOUR_RGB('Light Blue',0.38,0.62,0.78);
#40675=FILL_AREA_STYLE_COLOUR('',#40674);
#40676=FILL_AREA_STYLE('',(#40675));
#40677=SURFACE_STYLE_FILL_AREA(#40676);
#40678=SURFACE_SIDE_STYLE('',(#40677));
#40679=SURFACE_STYLE_USAGE(.BOTH.,#40678);
#40680=PRESENTATION_STYLE_ASSIGNMENT((#40679));
#40681=COLOUR_RGB('Sky Blue',0.24,0.69,0.87);
#40682=FILL_AREA_STYLE_COLOUR('',#40681);
#40683=FILL_AREA_STYLE('',(#40682));
#40684=SURFACE_STYLE_FILL_AREA(#40683);
#40685=SURFACE_SIDE_STYLE('',(#40684));
#40686=SURFACE_STYLE_USAGE(.BOTH.,#40685);
#40687=PRESENTATION_STYLE_ASSIGNMENT((#40686));
#40688=COLOUR_RGB('Grey',0.48,0.52,0.57);
#40689=FILL_AREA_STYLE_COLOUR('',#40688);
#40690=FILL_AREA_STYLE('',(#40689));
#40691=SURFACE_STYLE_FILL_AREA(#40690);
#40692=SURFACE_SIDE_STYLE('',(#40691));
#40693=SURFACE_STYLE_USAGE(.BOTH.,#40692);
#40694=PRESENTATION_STYLE_ASSIGNMENT((#40693));
#40695=COLOUR_RGB('Black',0.12,0.14,0.17);
#40696=FILL_AREA_STYLE_COLOUR('',#40695);
#40697=FILL_AREA_STYLE('',(#40696));
#40698=SURFACE_STYLE_FILL_AREA(#40697);
#40699=SURFACE_SIDE_STYLE('',(#40698));
#40700=SURFACE_STYLE_USAGE(.BOTH.,#40699);
#40701=PRESENTATION_STYLE_ASSIGNMENT((#40700));
#40702=COLOUR_RGB('Off White',0.89,0.88,0.83);
#40703=FILL_AREA_STYLE_COLOUR('',#40702);
#40704=FILL_AREA_STYLE('',(#40703));
#40705=SURFACE_STYLE_FILL_AREA(#40704);
#40706=SURFACE_SIDE_STYLE('',(#40705));
#40707=SURFACE_STYLE_USAGE(.BOTH.,#40706);
#40708=PRESENTATION_STYLE_ASSIGNMENT((#40707));
#40709=STYLED_ITEM('',(#40673),#4903);
#40710=STYLED_ITEM('',(#40687),#19265);
#40711=STYLED_ITEM('',(#40708),#32841);
#40712=STYLED_ITEM('',(#40673),#32173);
#40713=STYLED_ITEM('',(#40708),#18866);
#40714=STYLED_ITEM('',(#40680),#32046);
#40715=STYLED_ITEM('',(#40687),#19057);
#40716=STYLED_ITEM('',(#40687),#4819);
#40717=STYLED_ITEM('',(#40673),#18583);
#40718=STYLED_ITEM('',(#40701),#31982);
#40719=STYLED_ITEM('',(#40687),#18435);
#40720=STYLED_ITEM('',(#40680),#5167);
#40721=MECHANICAL_DESIGN_GEOMETRIC_PRESENTATION_REPRESENTATION('',(#40709,#40710,#40711,#40712,#40713,#40714,#40715,#40716,#40717,#40718,#40719,#40720),#11399);
ENDSEC;
END-ISO-10303-21;
